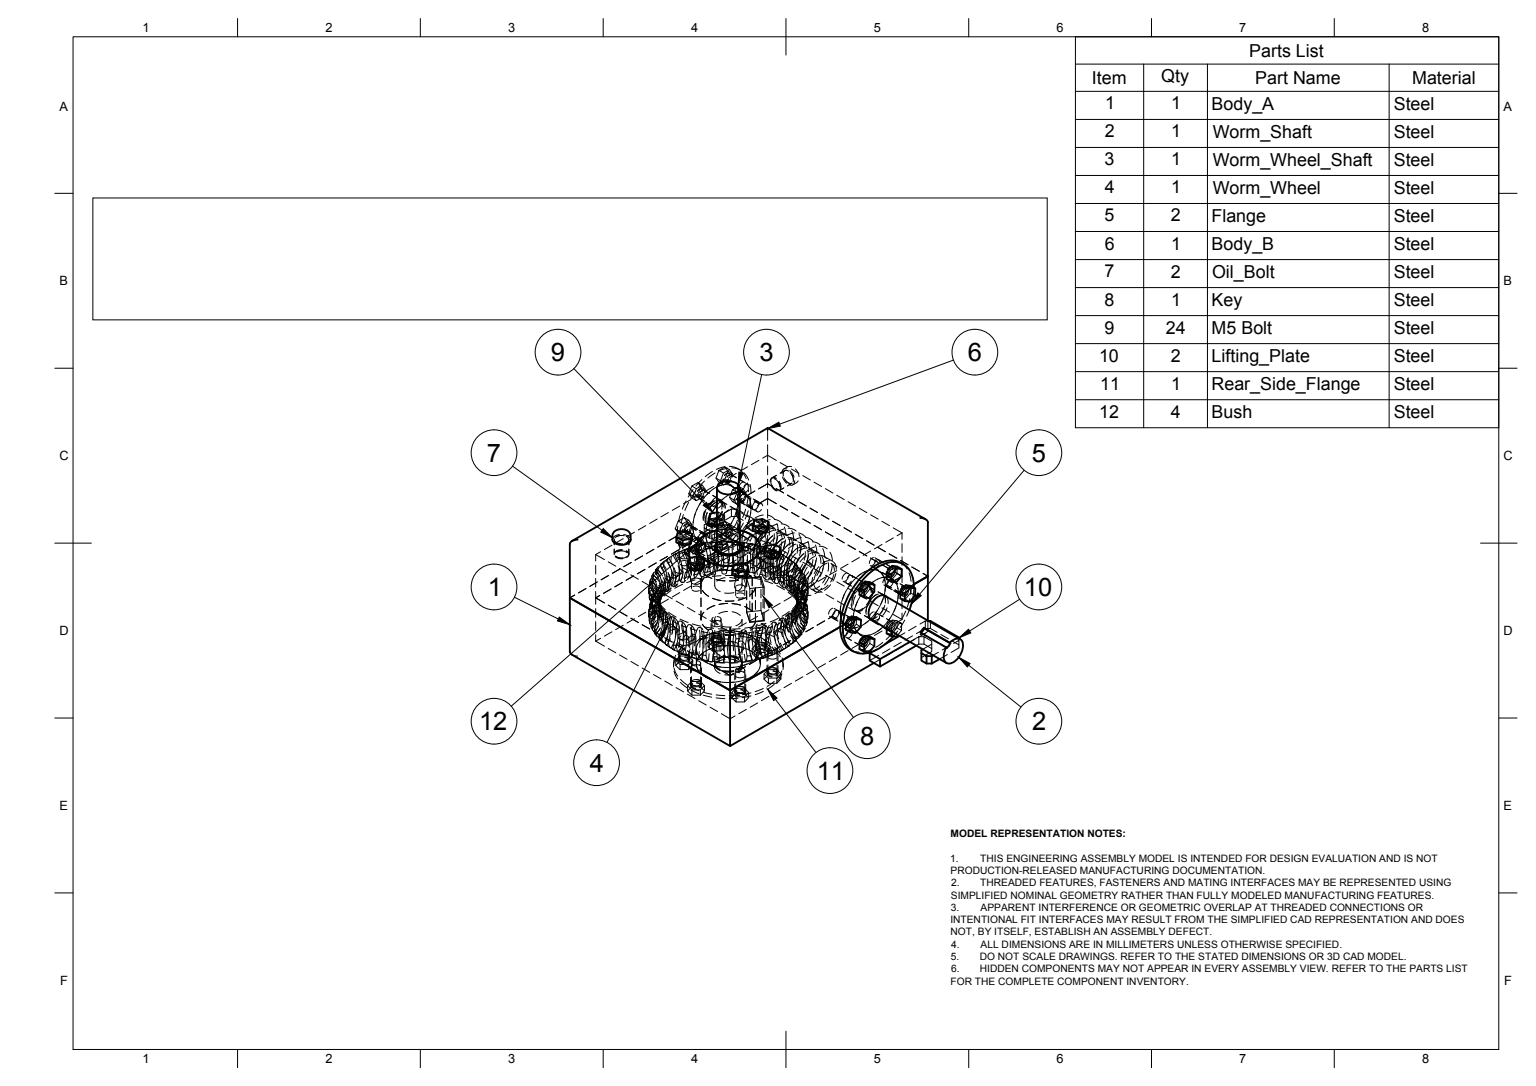
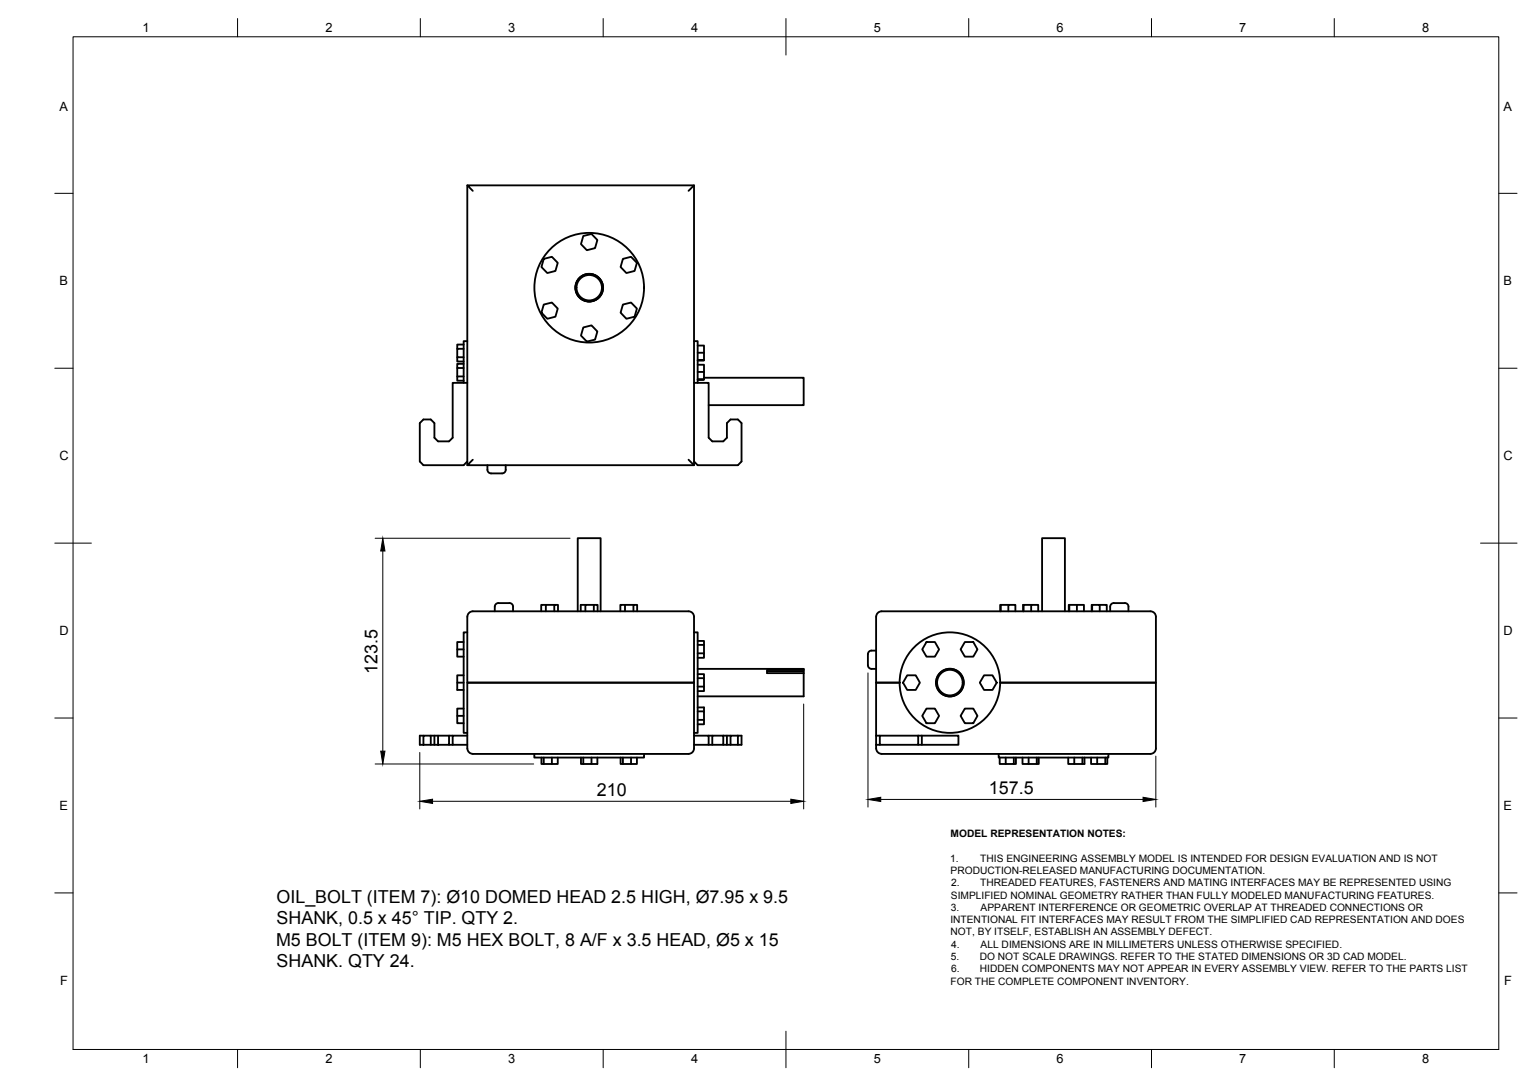
ISO-10303-21;
HEADER;
/* Generated by software containing ST-Developer
 * from STEP Tools, Inc. (www.steptools.com) 
 */

FILE_DESCRIPTION(
/* description */ ('STEP AP214'),
/* implementation_level */ '2;1');

FILE_NAME(
/* name */ 'MAS-619',
/* time_stamp */ '2026-10-05T13:15:56-07:00',
/* author */ (''),
/* organization */ (''),
/* preprocessor_version */ 'ST-DEVELOPER v20.2',
/* originating_system */ 'Autodesk Translation Framework v15.15.0.0',
/* authorisation */ '');

FILE_SCHEMA (('AUTOMOTIVE_DESIGN { 1 0 10303 214 3 1 1 }'));
ENDSEC;

DATA;
#10=MECHANICAL_DESIGN_GEOMETRIC_PRESENTATION_REPRESENTATION('',(#1345,#1346,
#1347,#1348,#1349,#1350,#1351,#1352,#1353,#1354,#1355,#1356),#37881);
#11=ITEM_DEFINED_TRANSFORMATION($,$,#10965,#11849);
#12=ITEM_DEFINED_TRANSFORMATION($,$,#11041,#11850);
#13=ITEM_DEFINED_TRANSFORMATION($,$,#11080,#11851);
#14=ITEM_DEFINED_TRANSFORMATION($,$,#11110,#11852);
#15=ITEM_DEFINED_TRANSFORMATION($,$,#11767,#11853);
#16=ITEM_DEFINED_TRANSFORMATION($,$,#11607,#11854);
#17=ITEM_DEFINED_TRANSFORMATION($,$,#11794,#11855);
#18=ITEM_DEFINED_TRANSFORMATION($,$,#11689,#11856);
#19=ITEM_DEFINED_TRANSFORMATION($,$,#11810,#11857);
#20=ITEM_DEFINED_TRANSFORMATION($,$,#11823,#11858);
#21=ITEM_DEFINED_TRANSFORMATION($,$,#11740,#11859);
#22=ITEM_DEFINED_TRANSFORMATION($,$,#11840,#11860);
#23=ITEM_DEFINED_TRANSFORMATION($,$,#11767,#11861);
#24=ITEM_DEFINED_TRANSFORMATION($,$,#11794,#11862);
#25=ITEM_DEFINED_TRANSFORMATION($,$,#11810,#11863);
#26=ITEM_DEFINED_TRANSFORMATION($,$,#11810,#11864);
#27=ITEM_DEFINED_TRANSFORMATION($,$,#11810,#11865);
#28=ITEM_DEFINED_TRANSFORMATION($,$,#11810,#11866);
#29=ITEM_DEFINED_TRANSFORMATION($,$,#11810,#11867);
#30=ITEM_DEFINED_TRANSFORMATION($,$,#11810,#11868);
#31=ITEM_DEFINED_TRANSFORMATION($,$,#11810,#11869);
#32=ITEM_DEFINED_TRANSFORMATION($,$,#11810,#11870);
#33=ITEM_DEFINED_TRANSFORMATION($,$,#11810,#11871);
#34=ITEM_DEFINED_TRANSFORMATION($,$,#11810,#11872);
#35=ITEM_DEFINED_TRANSFORMATION($,$,#11810,#11873);
#36=ITEM_DEFINED_TRANSFORMATION($,$,#11810,#11874);
#37=ITEM_DEFINED_TRANSFORMATION($,$,#11810,#11875);
#38=ITEM_DEFINED_TRANSFORMATION($,$,#11810,#11876);
#39=ITEM_DEFINED_TRANSFORMATION($,$,#11810,#11877);
#40=ITEM_DEFINED_TRANSFORMATION($,$,#11810,#11878);
#41=ITEM_DEFINED_TRANSFORMATION($,$,#11810,#11879);
#42=ITEM_DEFINED_TRANSFORMATION($,$,#11810,#11880);
#43=ITEM_DEFINED_TRANSFORMATION($,$,#11810,#11881);
#44=ITEM_DEFINED_TRANSFORMATION($,$,#11810,#11882);
#45=ITEM_DEFINED_TRANSFORMATION($,$,#11810,#11883);
#46=ITEM_DEFINED_TRANSFORMATION($,$,#11810,#11884);
#47=ITEM_DEFINED_TRANSFORMATION($,$,#11810,#11885);
#48=ITEM_DEFINED_TRANSFORMATION($,$,#11823,#11886);
#49=ITEM_DEFINED_TRANSFORMATION($,$,#11840,#11887);
#50=ITEM_DEFINED_TRANSFORMATION($,$,#11840,#11888);
#51=ITEM_DEFINED_TRANSFORMATION($,$,#11840,#11889);
#52=(
REPRESENTATION_RELATIONSHIP($,$,#37954,#37953)
REPRESENTATION_RELATIONSHIP_WITH_TRANSFORMATION(#11)
SHAPE_REPRESENTATION_RELATIONSHIP()
);
#53=(
REPRESENTATION_RELATIONSHIP($,$,#37955,#37953)
REPRESENTATION_RELATIONSHIP_WITH_TRANSFORMATION(#12)
SHAPE_REPRESENTATION_RELATIONSHIP()
);
#54=(
REPRESENTATION_RELATIONSHIP($,$,#37956,#37953)
REPRESENTATION_RELATIONSHIP_WITH_TRANSFORMATION(#13)
SHAPE_REPRESENTATION_RELATIONSHIP()
);
#55=(
REPRESENTATION_RELATIONSHIP($,$,#37957,#37953)
REPRESENTATION_RELATIONSHIP_WITH_TRANSFORMATION(#14)
SHAPE_REPRESENTATION_RELATIONSHIP()
);
#56=(
REPRESENTATION_RELATIONSHIP($,$,#37961,#37953)
REPRESENTATION_RELATIONSHIP_WITH_TRANSFORMATION(#15)
SHAPE_REPRESENTATION_RELATIONSHIP()
);
#57=(
REPRESENTATION_RELATIONSHIP($,$,#37958,#37953)
REPRESENTATION_RELATIONSHIP_WITH_TRANSFORMATION(#16)
SHAPE_REPRESENTATION_RELATIONSHIP()
);
#58=(
REPRESENTATION_RELATIONSHIP($,$,#37962,#37953)
REPRESENTATION_RELATIONSHIP_WITH_TRANSFORMATION(#17)
SHAPE_REPRESENTATION_RELATIONSHIP()
);
#59=(
REPRESENTATION_RELATIONSHIP($,$,#37959,#37953)
REPRESENTATION_RELATIONSHIP_WITH_TRANSFORMATION(#18)
SHAPE_REPRESENTATION_RELATIONSHIP()
);
#60=(
REPRESENTATION_RELATIONSHIP($,$,#37963,#37953)
REPRESENTATION_RELATIONSHIP_WITH_TRANSFORMATION(#19)
SHAPE_REPRESENTATION_RELATIONSHIP()
);
#61=(
REPRESENTATION_RELATIONSHIP($,$,#37964,#37953)
REPRESENTATION_RELATIONSHIP_WITH_TRANSFORMATION(#20)
SHAPE_REPRESENTATION_RELATIONSHIP()
);
#62=(
REPRESENTATION_RELATIONSHIP($,$,#37960,#37953)
REPRESENTATION_RELATIONSHIP_WITH_TRANSFORMATION(#21)
SHAPE_REPRESENTATION_RELATIONSHIP()
);
#63=(
REPRESENTATION_RELATIONSHIP($,$,#37965,#37953)
REPRESENTATION_RELATIONSHIP_WITH_TRANSFORMATION(#22)
SHAPE_REPRESENTATION_RELATIONSHIP()
);
#64=(
REPRESENTATION_RELATIONSHIP($,$,#37961,#37953)
REPRESENTATION_RELATIONSHIP_WITH_TRANSFORMATION(#23)
SHAPE_REPRESENTATION_RELATIONSHIP()
);
#65=(
REPRESENTATION_RELATIONSHIP($,$,#37962,#37953)
REPRESENTATION_RELATIONSHIP_WITH_TRANSFORMATION(#24)
SHAPE_REPRESENTATION_RELATIONSHIP()
);
#66=(
REPRESENTATION_RELATIONSHIP($,$,#37963,#37953)
REPRESENTATION_RELATIONSHIP_WITH_TRANSFORMATION(#25)
SHAPE_REPRESENTATION_RELATIONSHIP()
);
#67=(
REPRESENTATION_RELATIONSHIP($,$,#37963,#37953)
REPRESENTATION_RELATIONSHIP_WITH_TRANSFORMATION(#26)
SHAPE_REPRESENTATION_RELATIONSHIP()
);
#68=(
REPRESENTATION_RELATIONSHIP($,$,#37963,#37953)
REPRESENTATION_RELATIONSHIP_WITH_TRANSFORMATION(#27)
SHAPE_REPRESENTATION_RELATIONSHIP()
);
#69=(
REPRESENTATION_RELATIONSHIP($,$,#37963,#37953)
REPRESENTATION_RELATIONSHIP_WITH_TRANSFORMATION(#28)
SHAPE_REPRESENTATION_RELATIONSHIP()
);
#70=(
REPRESENTATION_RELATIONSHIP($,$,#37963,#37953)
REPRESENTATION_RELATIONSHIP_WITH_TRANSFORMATION(#29)
SHAPE_REPRESENTATION_RELATIONSHIP()
);
#71=(
REPRESENTATION_RELATIONSHIP($,$,#37963,#37953)
REPRESENTATION_RELATIONSHIP_WITH_TRANSFORMATION(#30)
SHAPE_REPRESENTATION_RELATIONSHIP()
);
#72=(
REPRESENTATION_RELATIONSHIP($,$,#37963,#37953)
REPRESENTATION_RELATIONSHIP_WITH_TRANSFORMATION(#31)
SHAPE_REPRESENTATION_RELATIONSHIP()
);
#73=(
REPRESENTATION_RELATIONSHIP($,$,#37963,#37953)
REPRESENTATION_RELATIONSHIP_WITH_TRANSFORMATION(#32)
SHAPE_REPRESENTATION_RELATIONSHIP()
);
#74=(
REPRESENTATION_RELATIONSHIP($,$,#37963,#37953)
REPRESENTATION_RELATIONSHIP_WITH_TRANSFORMATION(#33)
SHAPE_REPRESENTATION_RELATIONSHIP()
);
#75=(
REPRESENTATION_RELATIONSHIP($,$,#37963,#37953)
REPRESENTATION_RELATIONSHIP_WITH_TRANSFORMATION(#34)
SHAPE_REPRESENTATION_RELATIONSHIP()
);
#76=(
REPRESENTATION_RELATIONSHIP($,$,#37963,#37953)
REPRESENTATION_RELATIONSHIP_WITH_TRANSFORMATION(#35)
SHAPE_REPRESENTATION_RELATIONSHIP()
);
#77=(
REPRESENTATION_RELATIONSHIP($,$,#37963,#37953)
REPRESENTATION_RELATIONSHIP_WITH_TRANSFORMATION(#36)
SHAPE_REPRESENTATION_RELATIONSHIP()
);
#78=(
REPRESENTATION_RELATIONSHIP($,$,#37963,#37953)
REPRESENTATION_RELATIONSHIP_WITH_TRANSFORMATION(#37)
SHAPE_REPRESENTATION_RELATIONSHIP()
);
#79=(
REPRESENTATION_RELATIONSHIP($,$,#37963,#37953)
REPRESENTATION_RELATIONSHIP_WITH_TRANSFORMATION(#38)
SHAPE_REPRESENTATION_RELATIONSHIP()
);
#80=(
REPRESENTATION_RELATIONSHIP($,$,#37963,#37953)
REPRESENTATION_RELATIONSHIP_WITH_TRANSFORMATION(#39)
SHAPE_REPRESENTATION_RELATIONSHIP()
);
#81=(
REPRESENTATION_RELATIONSHIP($,$,#37963,#37953)
REPRESENTATION_RELATIONSHIP_WITH_TRANSFORMATION(#40)
SHAPE_REPRESENTATION_RELATIONSHIP()
);
#82=(
REPRESENTATION_RELATIONSHIP($,$,#37963,#37953)
REPRESENTATION_RELATIONSHIP_WITH_TRANSFORMATION(#41)
SHAPE_REPRESENTATION_RELATIONSHIP()
);
#83=(
REPRESENTATION_RELATIONSHIP($,$,#37963,#37953)
REPRESENTATION_RELATIONSHIP_WITH_TRANSFORMATION(#42)
SHAPE_REPRESENTATION_RELATIONSHIP()
);
#84=(
REPRESENTATION_RELATIONSHIP($,$,#37963,#37953)
REPRESENTATION_RELATIONSHIP_WITH_TRANSFORMATION(#43)
SHAPE_REPRESENTATION_RELATIONSHIP()
);
#85=(
REPRESENTATION_RELATIONSHIP($,$,#37963,#37953)
REPRESENTATION_RELATIONSHIP_WITH_TRANSFORMATION(#44)
SHAPE_REPRESENTATION_RELATIONSHIP()
);
#86=(
REPRESENTATION_RELATIONSHIP($,$,#37963,#37953)
REPRESENTATION_RELATIONSHIP_WITH_TRANSFORMATION(#45)
SHAPE_REPRESENTATION_RELATIONSHIP()
);
#87=(
REPRESENTATION_RELATIONSHIP($,$,#37963,#37953)
REPRESENTATION_RELATIONSHIP_WITH_TRANSFORMATION(#46)
SHAPE_REPRESENTATION_RELATIONSHIP()
);
#88=(
REPRESENTATION_RELATIONSHIP($,$,#37963,#37953)
REPRESENTATION_RELATIONSHIP_WITH_TRANSFORMATION(#47)
SHAPE_REPRESENTATION_RELATIONSHIP()
);
#89=(
REPRESENTATION_RELATIONSHIP($,$,#37964,#37953)
REPRESENTATION_RELATIONSHIP_WITH_TRANSFORMATION(#48)
SHAPE_REPRESENTATION_RELATIONSHIP()
);
#90=(
REPRESENTATION_RELATIONSHIP($,$,#37965,#37953)
REPRESENTATION_RELATIONSHIP_WITH_TRANSFORMATION(#49)
SHAPE_REPRESENTATION_RELATIONSHIP()
);
#91=(
REPRESENTATION_RELATIONSHIP($,$,#37965,#37953)
REPRESENTATION_RELATIONSHIP_WITH_TRANSFORMATION(#50)
SHAPE_REPRESENTATION_RELATIONSHIP()
);
#92=(
REPRESENTATION_RELATIONSHIP($,$,#37965,#37953)
REPRESENTATION_RELATIONSHIP_WITH_TRANSFORMATION(#51)
SHAPE_REPRESENTATION_RELATIONSHIP()
);
#93=CONTEXT_DEPENDENT_SHAPE_REPRESENTATION(#52,#37912);
#94=CONTEXT_DEPENDENT_SHAPE_REPRESENTATION(#53,#37913);
#95=CONTEXT_DEPENDENT_SHAPE_REPRESENTATION(#54,#37914);
#96=CONTEXT_DEPENDENT_SHAPE_REPRESENTATION(#55,#37915);
#97=CONTEXT_DEPENDENT_SHAPE_REPRESENTATION(#56,#37916);
#98=CONTEXT_DEPENDENT_SHAPE_REPRESENTATION(#57,#37917);
#99=CONTEXT_DEPENDENT_SHAPE_REPRESENTATION(#58,#37918);
#100=CONTEXT_DEPENDENT_SHAPE_REPRESENTATION(#59,#37919);
#101=CONTEXT_DEPENDENT_SHAPE_REPRESENTATION(#60,#37920);
#102=CONTEXT_DEPENDENT_SHAPE_REPRESENTATION(#61,#37921);
#103=CONTEXT_DEPENDENT_SHAPE_REPRESENTATION(#62,#37922);
#104=CONTEXT_DEPENDENT_SHAPE_REPRESENTATION(#63,#37923);
#105=CONTEXT_DEPENDENT_SHAPE_REPRESENTATION(#64,#37924);
#106=CONTEXT_DEPENDENT_SHAPE_REPRESENTATION(#65,#37925);
#107=CONTEXT_DEPENDENT_SHAPE_REPRESENTATION(#66,#37926);
#108=CONTEXT_DEPENDENT_SHAPE_REPRESENTATION(#67,#37927);
#109=CONTEXT_DEPENDENT_SHAPE_REPRESENTATION(#68,#37928);
#110=CONTEXT_DEPENDENT_SHAPE_REPRESENTATION(#69,#37929);
#111=CONTEXT_DEPENDENT_SHAPE_REPRESENTATION(#70,#37930);
#112=CONTEXT_DEPENDENT_SHAPE_REPRESENTATION(#71,#37931);
#113=CONTEXT_DEPENDENT_SHAPE_REPRESENTATION(#72,#37932);
#114=CONTEXT_DEPENDENT_SHAPE_REPRESENTATION(#73,#37933);
#115=CONTEXT_DEPENDENT_SHAPE_REPRESENTATION(#74,#37934);
#116=CONTEXT_DEPENDENT_SHAPE_REPRESENTATION(#75,#37935);
#117=CONTEXT_DEPENDENT_SHAPE_REPRESENTATION(#76,#37936);
#118=CONTEXT_DEPENDENT_SHAPE_REPRESENTATION(#77,#37937);
#119=CONTEXT_DEPENDENT_SHAPE_REPRESENTATION(#78,#37938);
#120=CONTEXT_DEPENDENT_SHAPE_REPRESENTATION(#79,#37939);
#121=CONTEXT_DEPENDENT_SHAPE_REPRESENTATION(#80,#37940);
#122=CONTEXT_DEPENDENT_SHAPE_REPRESENTATION(#81,#37941);
#123=CONTEXT_DEPENDENT_SHAPE_REPRESENTATION(#82,#37942);
#124=CONTEXT_DEPENDENT_SHAPE_REPRESENTATION(#83,#37943);
#125=CONTEXT_DEPENDENT_SHAPE_REPRESENTATION(#84,#37944);
#126=CONTEXT_DEPENDENT_SHAPE_REPRESENTATION(#85,#37945);
#127=CONTEXT_DEPENDENT_SHAPE_REPRESENTATION(#86,#37946);
#128=CONTEXT_DEPENDENT_SHAPE_REPRESENTATION(#87,#37947);
#129=CONTEXT_DEPENDENT_SHAPE_REPRESENTATION(#88,#37948);
#130=CONTEXT_DEPENDENT_SHAPE_REPRESENTATION(#89,#37949);
#131=CONTEXT_DEPENDENT_SHAPE_REPRESENTATION(#90,#37950);
#132=CONTEXT_DEPENDENT_SHAPE_REPRESENTATION(#91,#37951);
#133=CONTEXT_DEPENDENT_SHAPE_REPRESENTATION(#92,#37952);
#134=NEXT_ASSEMBLY_USAGE_OCCURRENCE('Body_A:1','Body_A:1','Body_A:1',#37967,
#37968,'Body_A:1');
#135=NEXT_ASSEMBLY_USAGE_OCCURRENCE('Worm_Shaft:1','Worm_Shaft:1',
'Worm_Shaft:1',#37967,#37969,'Worm_Shaft:1');
#136=NEXT_ASSEMBLY_USAGE_OCCURRENCE('Worm_Wheel_Shaft:1',
'Worm_Wheel_Shaft:1','Worm_Wheel_Shaft:1',#37967,#37970,
'Worm_Wheel_Shaft:1');
#137=NEXT_ASSEMBLY_USAGE_OCCURRENCE('Worm_Wheel:1','Worm_Wheel:1',
'Worm_Wheel:1',#37967,#37971,'Worm_Wheel:1');
#138=NEXT_ASSEMBLY_USAGE_OCCURRENCE('Flange:1','Flange:1','Flange:1',#37967,
#37975,'Flange:1');
#139=NEXT_ASSEMBLY_USAGE_OCCURRENCE('Body_B:1','Body_B:1','Body_B:1',#37967,
#37972,'Body_B:1');
#140=NEXT_ASSEMBLY_USAGE_OCCURRENCE('Oil_Bolt:1','Oil_Bolt:1',
'Oil_Bolt:1',#37967,#37976,'Oil_Bolt:1');
#141=NEXT_ASSEMBLY_USAGE_OCCURRENCE('Key:1','Key:1','Key:1',#37967,#37973,
'Key:1');
#142=NEXT_ASSEMBLY_USAGE_OCCURRENCE('M5 Bolt:1','M5 Bolt:1','M5 Bolt:1',
#37967,#37977,'M5 Bolt:1');
#143=NEXT_ASSEMBLY_USAGE_OCCURRENCE('Lifting_Plate:1','Lifting_Plate:1',
'Lifting_Plate:1',#37967,#37978,'Lifting_Plate:1');
#144=NEXT_ASSEMBLY_USAGE_OCCURRENCE('Rear_Side_Flange:1',
'Rear_Side_Flange:1','Rear_Side_Flange:1',#37967,#37974,
'Rear_Side_Flange:1');
#145=NEXT_ASSEMBLY_USAGE_OCCURRENCE('Bush:1','Bush:1','Bush:1',#37967,#37979,
'Bush:1');
#146=NEXT_ASSEMBLY_USAGE_OCCURRENCE('Flange:2','Flange:2','Flange:2',#37967,
#37975,'Flange:2');
#147=NEXT_ASSEMBLY_USAGE_OCCURRENCE('Oil_Bolt:2','Oil_Bolt:2',
'Oil_Bolt:2',#37967,#37976,'Oil_Bolt:2');
#148=NEXT_ASSEMBLY_USAGE_OCCURRENCE('M5 Bolt:2','M5 Bolt:2','M5 Bolt:2',
#37967,#37977,'M5 Bolt:2');
#149=NEXT_ASSEMBLY_USAGE_OCCURRENCE('M5 Bolt:3','M5 Bolt:3','M5 Bolt:3',
#37967,#37977,'M5 Bolt:3');
#150=NEXT_ASSEMBLY_USAGE_OCCURRENCE('M5 Bolt:4','M5 Bolt:4','M5 Bolt:4',
#37967,#37977,'M5 Bolt:4');
#151=NEXT_ASSEMBLY_USAGE_OCCURRENCE('M5 Bolt:5','M5 Bolt:5','M5 Bolt:5',
#37967,#37977,'M5 Bolt:5');
#152=NEXT_ASSEMBLY_USAGE_OCCURRENCE('M5 Bolt:6','M5 Bolt:6','M5 Bolt:6',
#37967,#37977,'M5 Bolt:6');
#153=NEXT_ASSEMBLY_USAGE_OCCURRENCE('M5 Bolt:7','M5 Bolt:7','M5 Bolt:7',
#37967,#37977,'M5 Bolt:7');
#154=NEXT_ASSEMBLY_USAGE_OCCURRENCE('M5 Bolt:8','M5 Bolt:8','M5 Bolt:8',
#37967,#37977,'M5 Bolt:8');
#155=NEXT_ASSEMBLY_USAGE_OCCURRENCE('M5 Bolt:9','M5 Bolt:9','M5 Bolt:9',
#37967,#37977,'M5 Bolt:9');
#156=NEXT_ASSEMBLY_USAGE_OCCURRENCE('M5 Bolt:10','M5 Bolt:10',
'M5 Bolt:10',#37967,#37977,'M5 Bolt:10');
#157=NEXT_ASSEMBLY_USAGE_OCCURRENCE('M5 Bolt:11','M5 Bolt:11',
'M5 Bolt:11',#37967,#37977,'M5 Bolt:11');
#158=NEXT_ASSEMBLY_USAGE_OCCURRENCE('M5 Bolt:12','M5 Bolt:12',
'M5 Bolt:12',#37967,#37977,'M5 Bolt:12');
#159=NEXT_ASSEMBLY_USAGE_OCCURRENCE('M5 Bolt:13','M5 Bolt:13',
'M5 Bolt:13',#37967,#37977,'M5 Bolt:13');
#160=NEXT_ASSEMBLY_USAGE_OCCURRENCE('M5 Bolt:14','M5 Bolt:14',
'M5 Bolt:14',#37967,#37977,'M5 Bolt:14');
#161=NEXT_ASSEMBLY_USAGE_OCCURRENCE('M5 Bolt:15','M5 Bolt:15',
'M5 Bolt:15',#37967,#37977,'M5 Bolt:15');
#162=NEXT_ASSEMBLY_USAGE_OCCURRENCE('M5 Bolt:16','M5 Bolt:16',
'M5 Bolt:16',#37967,#37977,'M5 Bolt:16');
#163=NEXT_ASSEMBLY_USAGE_OCCURRENCE('M5 Bolt:17','M5 Bolt:17',
'M5 Bolt:17',#37967,#37977,'M5 Bolt:17');
#164=NEXT_ASSEMBLY_USAGE_OCCURRENCE('M5 Bolt:18','M5 Bolt:18',
'M5 Bolt:18',#37967,#37977,'M5 Bolt:18');
#165=NEXT_ASSEMBLY_USAGE_OCCURRENCE('M5 Bolt:19','M5 Bolt:19',
'M5 Bolt:19',#37967,#37977,'M5 Bolt:19');
#166=NEXT_ASSEMBLY_USAGE_OCCURRENCE('M5 Bolt:20','M5 Bolt:20',
'M5 Bolt:20',#37967,#37977,'M5 Bolt:20');
#167=NEXT_ASSEMBLY_USAGE_OCCURRENCE('M5 Bolt:21','M5 Bolt:21',
'M5 Bolt:21',#37967,#37977,'M5 Bolt:21');
#168=NEXT_ASSEMBLY_USAGE_OCCURRENCE('M5 Bolt:22','M5 Bolt:22',
'M5 Bolt:22',#37967,#37977,'M5 Bolt:22');
#169=NEXT_ASSEMBLY_USAGE_OCCURRENCE('M5 Bolt:23','M5 Bolt:23',
'M5 Bolt:23',#37967,#37977,'M5 Bolt:23');
#170=NEXT_ASSEMBLY_USAGE_OCCURRENCE('M5 Bolt:24','M5 Bolt:24',
'M5 Bolt:24',#37967,#37977,'M5 Bolt:24');
#171=NEXT_ASSEMBLY_USAGE_OCCURRENCE('Lifting_Plate:2','Lifting_Plate:2',
'Lifting_Plate:2',#37967,#37978,'Lifting_Plate:2');
#172=NEXT_ASSEMBLY_USAGE_OCCURRENCE('Bush:2','Bush:2','Bush:2',#37967,#37979,
'Bush:2');
#173=NEXT_ASSEMBLY_USAGE_OCCURRENCE('Bush:3','Bush:3','Bush:3',#37967,#37979,
'Bush:3');
#174=NEXT_ASSEMBLY_USAGE_OCCURRENCE('Bush:4','Bush:4','Bush:4',#37967,#37979,
'Bush:4');
#175=SPHERICAL_SURFACE('',#11699,0.5);
#176=SPHERICAL_SURFACE('',#11702,0.5);
#177=SPHERICAL_SURFACE('',#11719,0.5);
#178=SPHERICAL_SURFACE('',#11721,0.5);
#179=SPHERICAL_SURFACE('',#11723,0.5);
#180=SPHERICAL_SURFACE('',#11725,0.5);
#181=SPHERICAL_SURFACE('',#11735,0.5);
#182=SPHERICAL_SURFACE('',#11737,0.5);
#183=TOROIDAL_SURFACE('',#11111,52.,10.5);
#184=TOROIDAL_SURFACE('',#11114,52.,10.5);
#185=TOROIDAL_SURFACE('',#11117,52.,10.5);
#186=TOROIDAL_SURFACE('',#11120,52.,10.5);
#187=TOROIDAL_SURFACE('',#11123,52.,10.5);
#188=TOROIDAL_SURFACE('',#11126,52.,10.5);
#189=TOROIDAL_SURFACE('',#11129,52.,10.5);
#190=TOROIDAL_SURFACE('',#11132,52.,10.5);
#191=TOROIDAL_SURFACE('',#11135,52.,10.5);
#192=TOROIDAL_SURFACE('',#11138,52.,10.5);
#193=TOROIDAL_SURFACE('',#11141,52.,10.5);
#194=TOROIDAL_SURFACE('',#11144,52.,10.5);
#195=TOROIDAL_SURFACE('',#11147,52.,10.5);
#196=TOROIDAL_SURFACE('',#11150,52.,10.5);
#197=TOROIDAL_SURFACE('',#11153,52.,10.5);
#198=TOROIDAL_SURFACE('',#11156,52.,10.5);
#199=TOROIDAL_SURFACE('',#11159,52.,10.5);
#200=TOROIDAL_SURFACE('',#11162,52.,10.5);
#201=TOROIDAL_SURFACE('',#11165,52.,10.5);
#202=TOROIDAL_SURFACE('',#11168,52.,10.5);
#203=TOROIDAL_SURFACE('',#11171,52.,10.5);
#204=TOROIDAL_SURFACE('',#11174,52.,10.5);
#205=TOROIDAL_SURFACE('',#11177,52.,10.5);
#206=TOROIDAL_SURFACE('',#11180,52.,10.5);
#207=TOROIDAL_SURFACE('',#11183,52.,10.5);
#208=TOROIDAL_SURFACE('',#11186,52.,10.5);
#209=TOROIDAL_SURFACE('',#11189,52.,10.5);
#210=TOROIDAL_SURFACE('',#11192,52.,10.5);
#211=TOROIDAL_SURFACE('',#11195,52.,10.5);
#212=TOROIDAL_SURFACE('',#11198,52.,10.5);
#213=TOROIDAL_SURFACE('',#11201,52.,10.5);
#214=TOROIDAL_SURFACE('',#11204,52.,10.5);
#215=TOROIDAL_SURFACE('',#11207,52.,10.5);
#216=TOROIDAL_SURFACE('',#11210,52.,10.5);
#217=TOROIDAL_SURFACE('',#11213,52.,10.5);
#218=TOROIDAL_SURFACE('',#11216,52.,10.5);
#219=TOROIDAL_SURFACE('',#11219,52.,10.5);
#220=TOROIDAL_SURFACE('',#11222,52.,10.5);
#221=TOROIDAL_SURFACE('',#11225,52.,10.5);
#222=TOROIDAL_SURFACE('',#11228,52.,10.5);
#223=TOROIDAL_SURFACE('',#11231,52.,10.5);
#224=TOROIDAL_SURFACE('',#11234,52.,10.5);
#225=TOROIDAL_SURFACE('',#11237,52.,10.5);
#226=TOROIDAL_SURFACE('',#11240,52.,10.5);
#227=TOROIDAL_SURFACE('',#11798,3.,2.);
#228=(
BOUNDED_CURVE()
B_SPLINE_CURVE(2,(#15162,#15163,#15164,#15165,#15166,#15167,#15168,#15169,
#15170,#15171,#15172,#15173,#15174,#15175,#15176,#15177,#15178,#15179,#15180,
#15181,#15182,#15183,#15184,#15185,#15186,#15187,#15188,#15189,#15190,#15191,
#15192,#15193,#15194,#15195,#15196,#15197,#15198,#15199,#15200,#15201,#15202,
#15203,#15204,#15205,#15206,#15207,#15208,#15209,#15210,#15211,#15212,#15213,
#15214,#15215,#15216,#15217,#15218,#15219,#15220,#15221,#15222,#15223,#15224,
#15225,#15226,#15227,#15228,#15229,#15230,#15231,#15232,#15233,#15234,#15235,
#15236,#15237,#15238,#15239,#15240,#15241,#15242,#15243,#15244,#15245,#15246,
#15247,#15248,#15249,#15250,#15251,#15252,#15253,#15254,#15255,#15256,#15257,
#15258,#15259,#15260,#15261,#15262,#15263,#15264,#15265,#15266,#15267,#15268,
#15269,#15270,#15271,#15272,#15273,#15274),.UNSPECIFIED.,.F.,.F.)
B_SPLINE_CURVE_WITH_KNOTS((3,2,2,2,2,2,2,2,2,2,2,2,2,2,2,2,2,2,2,2,2,2,
2,2,2,2,2,2,2,2,2,2,2,2,2,2,2,2,2,2,2,2,2,2,2,2,2,2,2,2,2,2,2,2,2,2,3),
(0.,0.0178571428571429,0.0357142857142857,0.0535714285714286,0.0714285714285714,
0.0892857142857143,0.107142857142857,0.125,0.142857142857143,0.160714285714286,
0.178571428571429,0.196428571428571,0.214285714285714,0.232142857142857,
0.25,0.267857142857143,0.285714285714286,0.303571428571429,0.321428571428571,
0.339285714285714,0.357142857142857,0.375,0.392857142857143,0.410714285714286,
0.428571428571429,0.446428571428571,0.464285714285714,0.482142857142857,
0.5,0.517857142857143,0.535714285714286,0.553571428571429,0.571428571428571,
0.589285714285714,0.607142857142857,0.625,0.642857142857143,0.660714285714286,
0.678571428571429,0.696428571428571,0.714285714285714,0.732142857142857,
0.75,0.767857142857143,0.785714285714286,0.803571428571429,0.821428571428571,
0.839285714285714,0.857142857142857,0.875,0.892857142857143,0.910714285714286,
0.928571428571429,0.946428571428571,0.964285714285714,0.982142857142857,
1.),.UNSPECIFIED.)
CURVE()
GEOMETRIC_REPRESENTATION_ITEM()
RATIONAL_B_SPLINE_CURVE((1.,0.974927912181824,1.,0.974927912181824,1.,0.974927912181824,
1.,0.974927912181824,1.,0.974927912181824,1.,0.974927912181824,1.,0.974927912181824,
1.,0.974927912181824,1.,0.974927912181824,1.,0.974927912181824,1.,0.974927912181824,
1.,0.974927912181824,1.,0.974927912181824,1.,0.974927912181824,1.,0.974927912181824,
1.,0.974927912181824,1.,0.974927912181824,1.,0.974927912181824,1.,0.974927912181824,
1.,0.974927912181824,1.,0.974927912181824,1.,0.974927912181824,1.,0.974927912181824,
1.,0.974927912181824,1.,0.974927912181824,1.,0.974927912181824,1.,0.974927912181824,
1.,0.974927912181824,1.,0.974927912181824,1.,0.974927912181824,1.,0.974927912181824,
1.,0.974927912181824,1.,0.974927912181824,1.,0.974927912181824,1.,0.974927912181824,
1.,0.974927912181824,1.,0.974927912181824,1.,0.974927912181824,1.,0.974927912181824,
1.,0.974927912181824,1.,0.974927912181824,1.,0.974927912181824,1.,0.974927912181824,
1.,0.974927912181824,1.,0.974927912181824,1.,0.974927912181824,1.,0.974927912181824,
1.,0.974927912181824,1.,0.974927912181824,1.,0.974927912181824,1.,0.974927912181824,
1.,0.974927912181824,1.,0.974927912181824,1.,0.974927912181824,1.,0.974927912181824,
1.,0.974927912181824,1.))
REPRESENTATION_ITEM('')
);
#229=(
BOUNDED_CURVE()
B_SPLINE_CURVE(2,(#15729,#15730,#15731,#15732,#15733,#15734,#15735,#15736,
#15737,#15738,#15739,#15740,#15741,#15742,#15743,#15744,#15745,#15746,#15747,
#15748,#15749,#15750,#15751,#15752,#15753,#15754,#15755,#15756,#15757,#15758,
#15759,#15760,#15761,#15762,#15763,#15764,#15765,#15766,#15767,#15768,#15769,
#15770,#15771,#15772,#15773,#15774,#15775,#15776,#15777,#15778,#15779,#15780,
#15781,#15782,#15783,#15784,#15785,#15786,#15787,#15788,#15789,#15790,#15791,
#15792,#15793,#15794,#15795,#15796,#15797,#15798,#15799,#15800,#15801,#15802,
#15803,#15804,#15805,#15806,#15807,#15808,#15809,#15810,#15811,#15812,#15813,
#15814,#15815,#15816,#15817,#15818,#15819,#15820,#15821,#15822,#15823,#15824,
#15825,#15826,#15827,#15828,#15829,#15830,#15831,#15832,#15833,#15834,#15835,
#15836,#15837,#15838,#15839,#15840,#15841),.UNSPECIFIED.,.F.,.F.)
B_SPLINE_CURVE_WITH_KNOTS((3,2,2,2,2,2,2,2,2,2,2,2,2,2,2,2,2,2,2,2,2,2,
2,2,2,2,2,2,2,2,2,2,2,2,2,2,2,2,2,2,2,2,2,2,2,2,2,2,2,2,2,2,2,2,2,2,3),
(0.,0.0178571428571429,0.0357142857142857,0.0535714285714286,0.0714285714285714,
0.0892857142857143,0.107142857142857,0.125,0.142857142857143,0.160714285714286,
0.178571428571429,0.196428571428571,0.214285714285714,0.232142857142857,
0.25,0.267857142857143,0.285714285714286,0.303571428571429,0.321428571428571,
0.339285714285714,0.357142857142857,0.375,0.392857142857143,0.410714285714286,
0.428571428571429,0.446428571428571,0.464285714285714,0.482142857142857,
0.5,0.517857142857143,0.535714285714286,0.553571428571429,0.571428571428571,
0.589285714285714,0.607142857142857,0.625,0.642857142857143,0.660714285714286,
0.678571428571429,0.696428571428571,0.714285714285714,0.732142857142857,
0.75,0.767857142857143,0.785714285714286,0.803571428571429,0.821428571428571,
0.839285714285714,0.857142857142857,0.875,0.892857142857143,0.910714285714286,
0.928571428571429,0.946428571428571,0.964285714285714,0.982142857142857,
1.),.UNSPECIFIED.)
CURVE()
GEOMETRIC_REPRESENTATION_ITEM()
RATIONAL_B_SPLINE_CURVE((1.,0.974927912181824,1.,0.974927912181824,1.,0.974927912181824,
1.,0.974927912181824,1.,0.974927912181824,1.,0.974927912181824,1.,0.974927912181824,
1.,0.974927912181824,1.,0.974927912181824,1.,0.974927912181824,1.,0.974927912181824,
1.,0.974927912181824,1.,0.974927912181824,1.,0.974927912181824,1.,0.974927912181824,
1.,0.974927912181824,1.,0.974927912181824,1.,0.974927912181824,1.,0.974927912181824,
1.,0.974927912181824,1.,0.974927912181824,1.,0.974927912181824,1.,0.974927912181824,
1.,0.974927912181824,1.,0.974927912181824,1.,0.974927912181824,1.,0.974927912181824,
1.,0.974927912181824,1.,0.974927912181824,1.,0.974927912181824,1.,0.974927912181824,
1.,0.974927912181824,1.,0.974927912181824,1.,0.974927912181824,1.,0.974927912181824,
1.,0.974927912181824,1.,0.974927912181824,1.,0.974927912181824,1.,0.974927912181824,
1.,0.974927912181824,1.,0.974927912181824,1.,0.974927912181824,1.,0.974927912181824,
1.,0.974927912181824,1.,0.974927912181824,1.,0.974927912181824,1.,0.974927912181824,
1.,0.974927912181824,1.,0.974927912181824,1.,0.974927912181824,1.,0.974927912181824,
1.,0.974927912181824,1.,0.974927912181824,1.,0.974927912181824,1.,0.974927912181824,
1.,0.974927912181824,1.))
REPRESENTATION_ITEM('')
);
#230=(
BOUNDED_CURVE()
B_SPLINE_CURVE(2,(#16301,#16302,#16303,#16304,#16305,#16306,#16307,#16308,
#16309,#16310,#16311,#16312,#16313,#16314,#16315,#16316,#16317,#16318,#16319,
#16320,#16321,#16322,#16323,#16324,#16325,#16326,#16327,#16328,#16329,#16330,
#16331,#16332,#16333,#16334,#16335,#16336,#16337,#16338,#16339,#16340,#16341,
#16342,#16343,#16344,#16345,#16346,#16347,#16348,#16349,#16350,#16351,#16352,
#16353,#16354,#16355,#16356,#16357,#16358,#16359,#16360,#16361,#16362,#16363,
#16364,#16365,#16366,#16367,#16368,#16369,#16370,#16371,#16372,#16373,#16374,
#16375,#16376,#16377,#16378,#16379,#16380,#16381,#16382,#16383,#16384,#16385,
#16386,#16387,#16388,#16389,#16390,#16391,#16392,#16393,#16394,#16395,#16396,
#16397,#16398,#16399,#16400,#16401,#16402,#16403,#16404,#16405,#16406,#16407,
#16408,#16409,#16410,#16411,#16412,#16413),.UNSPECIFIED.,.F.,.F.)
B_SPLINE_CURVE_WITH_KNOTS((3,2,2,2,2,2,2,2,2,2,2,2,2,2,2,2,2,2,2,2,2,2,
2,2,2,2,2,2,2,2,2,2,2,2,2,2,2,2,2,2,2,2,2,2,2,2,2,2,2,2,2,2,2,2,2,2,3),
(0.,0.0178571428571429,0.0357142857142857,0.0535714285714286,0.0714285714285714,
0.0892857142857143,0.107142857142857,0.125,0.142857142857143,0.160714285714286,
0.178571428571429,0.196428571428571,0.214285714285714,0.232142857142857,
0.25,0.267857142857143,0.285714285714286,0.303571428571429,0.321428571428571,
0.339285714285714,0.357142857142857,0.375,0.392857142857143,0.410714285714286,
0.428571428571429,0.446428571428571,0.464285714285714,0.482142857142857,
0.5,0.517857142857143,0.535714285714286,0.553571428571429,0.571428571428571,
0.589285714285714,0.607142857142857,0.625,0.642857142857143,0.660714285714286,
0.678571428571429,0.696428571428571,0.714285714285714,0.732142857142857,
0.75,0.767857142857143,0.785714285714286,0.803571428571429,0.821428571428571,
0.839285714285714,0.857142857142857,0.875,0.892857142857143,0.910714285714286,
0.928571428571429,0.946428571428571,0.964285714285714,0.982142857142857,
1.),.UNSPECIFIED.)
CURVE()
GEOMETRIC_REPRESENTATION_ITEM()
RATIONAL_B_SPLINE_CURVE((1.,0.974927912181824,1.,0.974927912181824,1.,0.974927912181824,
1.,0.974927912181824,1.,0.974927912181824,1.,0.974927912181824,1.,0.974927912181824,
1.,0.974927912181824,1.,0.974927912181824,1.,0.974927912181824,1.,0.974927912181824,
1.,0.974927912181824,1.,0.974927912181824,1.,0.974927912181824,1.,0.974927912181824,
1.,0.974927912181824,1.,0.974927912181824,1.,0.974927912181824,1.,0.974927912181824,
1.,0.974927912181824,1.,0.974927912181824,1.,0.974927912181824,1.,0.974927912181824,
1.,0.974927912181824,1.,0.974927912181824,1.,0.974927912181824,1.,0.974927912181824,
1.,0.974927912181824,1.,0.974927912181824,1.,0.974927912181824,1.,0.974927912181824,
1.,0.974927912181824,1.,0.974927912181824,1.,0.974927912181824,1.,0.974927912181824,
1.,0.974927912181824,1.,0.974927912181824,1.,0.974927912181824,1.,0.974927912181824,
1.,0.974927912181824,1.,0.974927912181824,1.,0.974927912181824,1.,0.974927912181824,
1.,0.974927912181824,1.,0.974927912181824,1.,0.974927912181824,1.,0.974927912181824,
1.,0.974927912181824,1.,0.974927912181824,1.,0.974927912181824,1.,0.974927912181824,
1.,0.974927912181824,1.,0.974927912181824,1.,0.974927912181824,1.,0.974927912181824,
1.,0.974927912181824,1.))
REPRESENTATION_ITEM('')
);
#231=(
BOUNDED_CURVE()
B_SPLINE_CURVE(2,(#16866,#16867,#16868,#16869,#16870,#16871,#16872,#16873,
#16874,#16875,#16876,#16877,#16878,#16879,#16880,#16881,#16882,#16883,#16884,
#16885,#16886,#16887,#16888,#16889,#16890,#16891,#16892,#16893,#16894,#16895,
#16896,#16897,#16898,#16899,#16900,#16901,#16902,#16903,#16904,#16905,#16906,
#16907,#16908,#16909,#16910,#16911,#16912,#16913,#16914,#16915,#16916,#16917,
#16918,#16919,#16920,#16921,#16922,#16923,#16924,#16925,#16926,#16927,#16928,
#16929,#16930,#16931,#16932,#16933,#16934,#16935,#16936,#16937,#16938,#16939,
#16940,#16941,#16942,#16943,#16944,#16945,#16946,#16947,#16948,#16949,#16950,
#16951,#16952,#16953,#16954,#16955,#16956,#16957,#16958,#16959,#16960,#16961,
#16962,#16963,#16964,#16965,#16966,#16967,#16968,#16969,#16970,#16971,#16972,
#16973,#16974,#16975,#16976,#16977,#16978),.UNSPECIFIED.,.F.,.F.)
B_SPLINE_CURVE_WITH_KNOTS((3,2,2,2,2,2,2,2,2,2,2,2,2,2,2,2,2,2,2,2,2,2,
2,2,2,2,2,2,2,2,2,2,2,2,2,2,2,2,2,2,2,2,2,2,2,2,2,2,2,2,2,2,2,2,2,2,3),
(0.,0.0178571428571429,0.0357142857142857,0.0535714285714286,0.0714285714285714,
0.0892857142857143,0.107142857142857,0.125,0.142857142857143,0.160714285714286,
0.178571428571429,0.196428571428571,0.214285714285714,0.232142857142857,
0.25,0.267857142857143,0.285714285714286,0.303571428571429,0.321428571428571,
0.339285714285714,0.357142857142857,0.375,0.392857142857143,0.410714285714286,
0.428571428571429,0.446428571428571,0.464285714285714,0.482142857142857,
0.5,0.517857142857143,0.535714285714286,0.553571428571429,0.571428571428571,
0.589285714285714,0.607142857142857,0.625,0.642857142857143,0.660714285714286,
0.678571428571429,0.696428571428571,0.714285714285714,0.732142857142857,
0.75,0.767857142857143,0.785714285714286,0.803571428571429,0.821428571428571,
0.839285714285714,0.857142857142857,0.875,0.892857142857143,0.910714285714286,
0.928571428571429,0.946428571428571,0.964285714285714,0.982142857142857,
1.),.UNSPECIFIED.)
CURVE()
GEOMETRIC_REPRESENTATION_ITEM()
RATIONAL_B_SPLINE_CURVE((1.,0.974927912181824,1.,0.974927912181824,1.,0.974927912181824,
1.,0.974927912181824,1.,0.974927912181824,1.,0.974927912181824,1.,0.974927912181824,
1.,0.974927912181824,1.,0.974927912181824,1.,0.974927912181824,1.,0.974927912181824,
1.,0.974927912181824,1.,0.974927912181824,1.,0.974927912181824,1.,0.974927912181824,
1.,0.974927912181824,1.,0.974927912181824,1.,0.974927912181824,1.,0.974927912181824,
1.,0.974927912181824,1.,0.974927912181824,1.,0.974927912181824,1.,0.974927912181824,
1.,0.974927912181824,1.,0.974927912181824,1.,0.974927912181824,1.,0.974927912181824,
1.,0.974927912181824,1.,0.974927912181824,1.,0.974927912181824,1.,0.974927912181824,
1.,0.974927912181824,1.,0.974927912181824,1.,0.974927912181824,1.,0.974927912181824,
1.,0.974927912181824,1.,0.974927912181824,1.,0.974927912181824,1.,0.974927912181824,
1.,0.974927912181824,1.,0.974927912181824,1.,0.974927912181824,1.,0.974927912181824,
1.,0.974927912181824,1.,0.974927912181824,1.,0.974927912181824,1.,0.974927912181824,
1.,0.974927912181824,1.,0.974927912181824,1.,0.974927912181824,1.,0.974927912181824,
1.,0.974927912181824,1.,0.974927912181824,1.,0.974927912181824,1.,0.974927912181824,
1.,0.974927912181824,1.))
REPRESENTATION_ITEM('')
);
#232=(
BOUNDED_CURVE()
B_SPLINE_CURVE(2,(#22947,#22948,#22949,#22950,#22951),.UNSPECIFIED.,.F.,
 .F.)
B_SPLINE_CURVE_WITH_KNOTS((3,2,3),(0.,0.25,0.459577358091282),
 .UNSPECIFIED.)
CURVE()
GEOMETRIC_REPRESENTATION_ITEM()
RATIONAL_B_SPLINE_CURVE((1.,0.974927912181824,1.,0.978981832292936,0.9932031210656))
REPRESENTATION_ITEM('')
);
#233=(
BOUNDED_CURVE()
B_SPLINE_CURVE(3,(#23082,#23083,#23084,#23085,#23086,#23087,#23088,#23089),
 .UNSPECIFIED.,.F.,.F.)
B_SPLINE_CURVE_WITH_KNOTS((4,2,2,4),(0.0783698293107414,0.308777371982556,
0.539184914655036,0.563918778704656),.UNSPECIFIED.)
CURVE()
GEOMETRIC_REPRESENTATION_ITEM()
RATIONAL_B_SPLINE_CURVE((1.,1.,1.,1.,1.,1.,1.,1.))
REPRESENTATION_ITEM('')
);
#234=(
BOUNDED_CURVE()
B_SPLINE_CURVE(2,(#23313,#23314,#23315,#23316,#23317),.UNSPECIFIED.,.F.,
 .F.)
B_SPLINE_CURVE_WITH_KNOTS((3,2,3),(0.,0.25,0.459577358091282),
 .UNSPECIFIED.)
CURVE()
GEOMETRIC_REPRESENTATION_ITEM()
RATIONAL_B_SPLINE_CURVE((1.,0.974927912181824,1.,0.978981832292936,0.9932031210656))
REPRESENTATION_ITEM('')
);
#235=(
BOUNDED_CURVE()
B_SPLINE_CURVE(2,(#23485,#23486,#23487,#23488,#23489),.UNSPECIFIED.,.F.,
 .F.)
B_SPLINE_CURVE_WITH_KNOTS((3,2,3),(0.,0.25,0.459577358091281),
 .UNSPECIFIED.)
CURVE()
GEOMETRIC_REPRESENTATION_ITEM()
RATIONAL_B_SPLINE_CURVE((1.,0.974927912181824,1.,0.978981832292936,0.9932031210656))
REPRESENTATION_ITEM('')
);
#236=(
BOUNDED_CURVE()
B_SPLINE_CURVE(2,(#23568,#23569,#23570,#23571,#23572),.UNSPECIFIED.,.F.,
 .F.)
B_SPLINE_CURVE_WITH_KNOTS((3,2,3),(0.,0.25,0.460808762537663),
 .UNSPECIFIED.)
CURVE()
GEOMETRIC_REPRESENTATION_ITEM()
RATIONAL_B_SPLINE_CURVE((1.,0.974927912181824,1.,0.978858336771259,0.993371456448429))
REPRESENTATION_ITEM('')
);
#237=(
BOUNDED_CURVE()
B_SPLINE_CURVE(2,(#23610,#23611,#23612,#23613,#23614),.UNSPECIFIED.,.F.,
 .F.)
B_SPLINE_CURVE_WITH_KNOTS((3,2,3),(0.,0.25,0.459577358091282),
 .UNSPECIFIED.)
CURVE()
GEOMETRIC_REPRESENTATION_ITEM()
RATIONAL_B_SPLINE_CURVE((1.,0.974927912181824,1.,0.978981832292936,0.9932031210656))
REPRESENTATION_ITEM('')
);
#238=(
BOUNDED_CURVE()
B_SPLINE_CURVE(2,(#23782,#23783,#23784,#23785,#23786),.UNSPECIFIED.,.F.,
 .F.)
B_SPLINE_CURVE_WITH_KNOTS((3,2,3),(0.,0.25,0.459577358091282),
 .UNSPECIFIED.)
CURVE()
GEOMETRIC_REPRESENTATION_ITEM()
RATIONAL_B_SPLINE_CURVE((1.,0.974927912181824,1.,0.978981832292936,0.9932031210656))
REPRESENTATION_ITEM('')
);
#239=(
BOUNDED_CURVE()
B_SPLINE_CURVE(2,(#23954,#23955,#23956,#23957,#23958),.UNSPECIFIED.,.F.,
 .F.)
B_SPLINE_CURVE_WITH_KNOTS((3,2,3),(0.,0.25,0.459577358091282),
 .UNSPECIFIED.)
CURVE()
GEOMETRIC_REPRESENTATION_ITEM()
RATIONAL_B_SPLINE_CURVE((1.,0.974927912181824,1.,0.978981832292936,0.9932031210656))
REPRESENTATION_ITEM('')
);
#240=(
BOUNDED_CURVE()
B_SPLINE_CURVE(2,(#24126,#24127,#24128,#24129,#24130),.UNSPECIFIED.,.F.,
 .F.)
B_SPLINE_CURVE_WITH_KNOTS((3,2,3),(0.,0.25,0.459577358091283),
 .UNSPECIFIED.)
CURVE()
GEOMETRIC_REPRESENTATION_ITEM()
RATIONAL_B_SPLINE_CURVE((1.,0.974927912181824,1.,0.978981832292936,0.9932031210656))
REPRESENTATION_ITEM('')
);
#241=(
BOUNDED_CURVE()
B_SPLINE_CURVE(2,(#24298,#24299,#24300,#24301,#24302),.UNSPECIFIED.,.F.,
 .F.)
B_SPLINE_CURVE_WITH_KNOTS((3,2,3),(0.,0.25,0.459577358091282),
 .UNSPECIFIED.)
CURVE()
GEOMETRIC_REPRESENTATION_ITEM()
RATIONAL_B_SPLINE_CURVE((1.,0.974927912181824,1.,0.978981832292936,0.9932031210656))
REPRESENTATION_ITEM('')
);
#242=(
BOUNDED_CURVE()
B_SPLINE_CURVE(2,(#24470,#24471,#24472,#24473,#24474),.UNSPECIFIED.,.F.,
 .F.)
B_SPLINE_CURVE_WITH_KNOTS((3,2,3),(0.,0.25,0.459577358091282),
 .UNSPECIFIED.)
CURVE()
GEOMETRIC_REPRESENTATION_ITEM()
RATIONAL_B_SPLINE_CURVE((1.,0.974927912181824,1.,0.978981832292936,0.9932031210656))
REPRESENTATION_ITEM('')
);
#243=(
BOUNDED_CURVE()
B_SPLINE_CURVE(2,(#24642,#24643,#24644,#24645,#24646),.UNSPECIFIED.,.F.,
 .F.)
B_SPLINE_CURVE_WITH_KNOTS((3,2,3),(0.,0.25,0.459577358091282),
 .UNSPECIFIED.)
CURVE()
GEOMETRIC_REPRESENTATION_ITEM()
RATIONAL_B_SPLINE_CURVE((1.,0.974927912181824,1.,0.978981832292936,0.9932031210656))
REPRESENTATION_ITEM('')
);
#244=(
BOUNDED_CURVE()
B_SPLINE_CURVE(2,(#24814,#24815,#24816,#24817,#24818),.UNSPECIFIED.,.F.,
 .F.)
B_SPLINE_CURVE_WITH_KNOTS((3,2,3),(0.,0.25,0.459577358091282),
 .UNSPECIFIED.)
CURVE()
GEOMETRIC_REPRESENTATION_ITEM()
RATIONAL_B_SPLINE_CURVE((1.,0.974927912181824,1.,0.978981832292936,0.9932031210656))
REPRESENTATION_ITEM('')
);
#245=(
BOUNDED_CURVE()
B_SPLINE_CURVE(2,(#24986,#24987,#24988,#24989,#24990),.UNSPECIFIED.,.F.,
 .F.)
B_SPLINE_CURVE_WITH_KNOTS((3,2,3),(0.,0.25,0.459577358091283),
 .UNSPECIFIED.)
CURVE()
GEOMETRIC_REPRESENTATION_ITEM()
RATIONAL_B_SPLINE_CURVE((1.,0.974927912181824,1.,0.978981832292936,0.9932031210656))
REPRESENTATION_ITEM('')
);
#246=(
BOUNDED_CURVE()
B_SPLINE_CURVE(2,(#25069,#25070,#25071,#25072,#25073),.UNSPECIFIED.,.F.,
 .F.)
B_SPLINE_CURVE_WITH_KNOTS((3,2,3),(0.,0.25,0.460808762537663),
 .UNSPECIFIED.)
CURVE()
GEOMETRIC_REPRESENTATION_ITEM()
RATIONAL_B_SPLINE_CURVE((1.,0.974927912181824,1.,0.978858336771258,0.993371456448429))
REPRESENTATION_ITEM('')
);
#247=(
BOUNDED_CURVE()
B_SPLINE_CURVE(2,(#25111,#25112,#25113,#25114,#25115),.UNSPECIFIED.,.F.,
 .F.)
B_SPLINE_CURVE_WITH_KNOTS((3,2,3),(0.,0.25,0.459577358091282),
 .UNSPECIFIED.)
CURVE()
GEOMETRIC_REPRESENTATION_ITEM()
RATIONAL_B_SPLINE_CURVE((1.,0.974927912181824,1.,0.978981832292936,0.9932031210656))
REPRESENTATION_ITEM('')
);
#248=(
BOUNDED_CURVE()
B_SPLINE_CURVE(2,(#25283,#25284,#25285,#25286,#25287),.UNSPECIFIED.,.F.,
 .F.)
B_SPLINE_CURVE_WITH_KNOTS((3,2,3),(0.,0.25,0.459577358091282),
 .UNSPECIFIED.)
CURVE()
GEOMETRIC_REPRESENTATION_ITEM()
RATIONAL_B_SPLINE_CURVE((1.,0.974927912181824,1.,0.978981832292936,0.9932031210656))
REPRESENTATION_ITEM('')
);
#249=(
BOUNDED_CURVE()
B_SPLINE_CURVE(2,(#25455,#25456,#25457,#25458,#25459),.UNSPECIFIED.,.F.,
 .F.)
B_SPLINE_CURVE_WITH_KNOTS((3,2,3),(0.,0.25,0.459577358091283),
 .UNSPECIFIED.)
CURVE()
GEOMETRIC_REPRESENTATION_ITEM()
RATIONAL_B_SPLINE_CURVE((1.,0.974927912181824,1.,0.978981832292936,0.9932031210656))
REPRESENTATION_ITEM('')
);
#250=(
BOUNDED_CURVE()
B_SPLINE_CURVE(2,(#25537,#25538,#25539,#25540,#25541),.UNSPECIFIED.,.F.,
 .F.)
B_SPLINE_CURVE_WITH_KNOTS((3,2,3),(0.,0.0714285714285714,0.131307816597586),
 .UNSPECIFIED.)
CURVE()
GEOMETRIC_REPRESENTATION_ITEM()
RATIONAL_B_SPLINE_CURVE((1.,0.974927912181824,1.,0.978981832292909,0.993203121065636))
REPRESENTATION_ITEM('')
);
#251=(
BOUNDED_CURVE()
B_SPLINE_CURVE(2,(#25581,#25582,#25583,#25584,#25585),.UNSPECIFIED.,.F.,
 .F.)
B_SPLINE_CURVE_WITH_KNOTS((3,2,3),(0.,0.0714285714285714,0.131659646439332),
 .UNSPECIFIED.)
CURVE()
GEOMETRIC_REPRESENTATION_ITEM()
RATIONAL_B_SPLINE_CURVE((1.,0.974927912181824,1.,0.978858336771259,0.993371456448429))
REPRESENTATION_ITEM('')
);
#252=(
BOUNDED_CURVE()
B_SPLINE_CURVE(2,(#25752,#25753,#25754,#25755,#25756),.UNSPECIFIED.,.F.,
 .F.)
B_SPLINE_CURVE_WITH_KNOTS((3,2,3),(0.,0.25,0.459577358091283),
 .UNSPECIFIED.)
CURVE()
GEOMETRIC_REPRESENTATION_ITEM()
RATIONAL_B_SPLINE_CURVE((1.,0.974927912181824,1.,0.978981832292936,0.9932031210656))
REPRESENTATION_ITEM('')
);
#253=(
BOUNDED_CURVE()
B_SPLINE_CURVE(2,(#25924,#25925,#25926,#25927,#25928),.UNSPECIFIED.,.F.,
 .F.)
B_SPLINE_CURVE_WITH_KNOTS((3,2,3),(0.,0.25,0.459577358091282),
 .UNSPECIFIED.)
CURVE()
GEOMETRIC_REPRESENTATION_ITEM()
RATIONAL_B_SPLINE_CURVE((1.,0.974927912181824,1.,0.978981832292936,0.9932031210656))
REPRESENTATION_ITEM('')
);
#254=(
BOUNDED_CURVE()
B_SPLINE_CURVE(2,(#26096,#26097,#26098,#26099,#26100),.UNSPECIFIED.,.F.,
 .F.)
B_SPLINE_CURVE_WITH_KNOTS((3,2,3),(0.,0.25,0.459577358091282),
 .UNSPECIFIED.)
CURVE()
GEOMETRIC_REPRESENTATION_ITEM()
RATIONAL_B_SPLINE_CURVE((1.,0.974927912181824,1.,0.978981832292936,0.9932031210656))
REPRESENTATION_ITEM('')
);
#255=(
BOUNDED_CURVE()
B_SPLINE_CURVE(2,(#26268,#26269,#26270,#26271,#26272),.UNSPECIFIED.,.F.,
 .F.)
B_SPLINE_CURVE_WITH_KNOTS((3,2,3),(0.,0.25,0.459577358091282),
 .UNSPECIFIED.)
CURVE()
GEOMETRIC_REPRESENTATION_ITEM()
RATIONAL_B_SPLINE_CURVE((1.,0.974927912181824,1.,0.978981832292936,0.9932031210656))
REPRESENTATION_ITEM('')
);
#256=(
BOUNDED_CURVE()
B_SPLINE_CURVE(2,(#26440,#26441,#26442,#26443,#26444),.UNSPECIFIED.,.F.,
 .F.)
B_SPLINE_CURVE_WITH_KNOTS((3,2,3),(0.,0.25,0.459577358091282),
 .UNSPECIFIED.)
CURVE()
GEOMETRIC_REPRESENTATION_ITEM()
RATIONAL_B_SPLINE_CURVE((1.,0.974927912181824,1.,0.978981832292936,0.9932031210656))
REPRESENTATION_ITEM('')
);
#257=(
BOUNDED_CURVE()
B_SPLINE_CURVE(2,(#26612,#26613,#26614,#26615,#26616),.UNSPECIFIED.,.F.,
 .F.)
B_SPLINE_CURVE_WITH_KNOTS((3,2,3),(0.,0.25,0.459577358091282),
 .UNSPECIFIED.)
CURVE()
GEOMETRIC_REPRESENTATION_ITEM()
RATIONAL_B_SPLINE_CURVE((1.,0.974927912181824,1.,0.978981832292936,0.9932031210656))
REPRESENTATION_ITEM('')
);
#258=(
BOUNDED_CURVE()
B_SPLINE_CURVE(2,(#26784,#26785,#26786,#26787,#26788),.UNSPECIFIED.,.F.,
 .F.)
B_SPLINE_CURVE_WITH_KNOTS((3,2,3),(0.,0.25,0.459577358091282),
 .UNSPECIFIED.)
CURVE()
GEOMETRIC_REPRESENTATION_ITEM()
RATIONAL_B_SPLINE_CURVE((1.,0.974927912181824,1.,0.978981832292936,0.9932031210656))
REPRESENTATION_ITEM('')
);
#259=(
BOUNDED_CURVE()
B_SPLINE_CURVE(2,(#26956,#26957,#26958,#26959,#26960),.UNSPECIFIED.,.F.,
 .F.)
B_SPLINE_CURVE_WITH_KNOTS((3,2,3),(0.,0.25,0.459577358091282),
 .UNSPECIFIED.)
CURVE()
GEOMETRIC_REPRESENTATION_ITEM()
RATIONAL_B_SPLINE_CURVE((1.,0.974927912181824,1.,0.978981832292936,0.9932031210656))
REPRESENTATION_ITEM('')
);
#260=(
BOUNDED_CURVE()
B_SPLINE_CURVE(2,(#27128,#27129,#27130,#27131,#27132),.UNSPECIFIED.,.F.,
 .F.)
B_SPLINE_CURVE_WITH_KNOTS((3,2,3),(0.,0.25,0.459577358091283),
 .UNSPECIFIED.)
CURVE()
GEOMETRIC_REPRESENTATION_ITEM()
RATIONAL_B_SPLINE_CURVE((1.,0.974927912181824,1.,0.978981832292936,0.9932031210656))
REPRESENTATION_ITEM('')
);
#261=(
BOUNDED_CURVE()
B_SPLINE_CURVE(2,(#27211,#27212,#27213,#27214,#27215),.UNSPECIFIED.,.F.,
 .F.)
B_SPLINE_CURVE_WITH_KNOTS((3,2,3),(0.,0.25,0.460808762537664),
 .UNSPECIFIED.)
CURVE()
GEOMETRIC_REPRESENTATION_ITEM()
RATIONAL_B_SPLINE_CURVE((1.,0.974927912181824,1.,0.978858336771258,0.993371456448429))
REPRESENTATION_ITEM('')
);
#262=(
BOUNDED_CURVE()
B_SPLINE_CURVE(2,(#27253,#27254,#27255,#27256,#27257),.UNSPECIFIED.,.F.,
 .F.)
B_SPLINE_CURVE_WITH_KNOTS((3,2,3),(0.,0.25,0.459577358091283),
 .UNSPECIFIED.)
CURVE()
GEOMETRIC_REPRESENTATION_ITEM()
RATIONAL_B_SPLINE_CURVE((1.,0.974927912181824,1.,0.978981832292936,0.9932031210656))
REPRESENTATION_ITEM('')
);
#263=(
BOUNDED_CURVE()
B_SPLINE_CURVE(2,(#27336,#27337,#27338,#27339,#27340),.UNSPECIFIED.,.F.,
 .F.)
B_SPLINE_CURVE_WITH_KNOTS((3,2,3),(0.,0.25,0.460808762537663),
 .UNSPECIFIED.)
CURVE()
GEOMETRIC_REPRESENTATION_ITEM()
RATIONAL_B_SPLINE_CURVE((1.,0.974927912181824,1.,0.978858336771258,0.993371456448429))
REPRESENTATION_ITEM('')
);
#264=(
BOUNDED_CURVE()
B_SPLINE_CURVE(2,(#27378,#27379,#27380,#27381,#27382),.UNSPECIFIED.,.F.,
 .F.)
B_SPLINE_CURVE_WITH_KNOTS((3,2,3),(0.,0.25,0.459577358091282),
 .UNSPECIFIED.)
CURVE()
GEOMETRIC_REPRESENTATION_ITEM()
RATIONAL_B_SPLINE_CURVE((1.,0.974927912181824,1.,0.978981832292936,0.9932031210656))
REPRESENTATION_ITEM('')
);
#265=(
BOUNDED_CURVE()
B_SPLINE_CURVE(2,(#27550,#27551,#27552,#27553,#27554),.UNSPECIFIED.,.F.,
 .F.)
B_SPLINE_CURVE_WITH_KNOTS((3,2,3),(0.,0.25,0.459577358091282),
 .UNSPECIFIED.)
CURVE()
GEOMETRIC_REPRESENTATION_ITEM()
RATIONAL_B_SPLINE_CURVE((1.,0.974927912181824,1.,0.978981832292936,0.9932031210656))
REPRESENTATION_ITEM('')
);
#266=(
BOUNDED_CURVE()
B_SPLINE_CURVE(2,(#27722,#27723,#27724,#27725,#27726),.UNSPECIFIED.,.F.,
 .F.)
B_SPLINE_CURVE_WITH_KNOTS((3,2,3),(0.,0.25,0.459577358091282),
 .UNSPECIFIED.)
CURVE()
GEOMETRIC_REPRESENTATION_ITEM()
RATIONAL_B_SPLINE_CURVE((1.,0.974927912181824,1.,0.978981832292936,0.9932031210656))
REPRESENTATION_ITEM('')
);
#267=(
BOUNDED_CURVE()
B_SPLINE_CURVE(2,(#27894,#27895,#27896,#27897,#27898),.UNSPECIFIED.,.F.,
 .F.)
B_SPLINE_CURVE_WITH_KNOTS((3,2,3),(0.,0.25,0.459577358091282),
 .UNSPECIFIED.)
CURVE()
GEOMETRIC_REPRESENTATION_ITEM()
RATIONAL_B_SPLINE_CURVE((1.,0.974927912181824,1.,0.978981832292936,0.9932031210656))
REPRESENTATION_ITEM('')
);
#268=(
BOUNDED_CURVE()
B_SPLINE_CURVE(2,(#28066,#28067,#28068,#28069,#28070),.UNSPECIFIED.,.F.,
 .F.)
B_SPLINE_CURVE_WITH_KNOTS((3,2,3),(0.,0.25,0.459577358091282),
 .UNSPECIFIED.)
CURVE()
GEOMETRIC_REPRESENTATION_ITEM()
RATIONAL_B_SPLINE_CURVE((1.,0.974927912181824,1.,0.978981832292936,0.9932031210656))
REPRESENTATION_ITEM('')
);
#269=(
BOUNDED_CURVE()
B_SPLINE_CURVE(2,(#28238,#28239,#28240,#28241,#28242),.UNSPECIFIED.,.F.,
 .F.)
B_SPLINE_CURVE_WITH_KNOTS((3,2,3),(0.,0.25,0.459577358091282),
 .UNSPECIFIED.)
CURVE()
GEOMETRIC_REPRESENTATION_ITEM()
RATIONAL_B_SPLINE_CURVE((1.,0.974927912181824,1.,0.978981832292936,0.9932031210656))
REPRESENTATION_ITEM('')
);
#270=(
BOUNDED_CURVE()
B_SPLINE_CURVE(2,(#28410,#28411,#28412,#28413,#28414),.UNSPECIFIED.,.F.,
 .F.)
B_SPLINE_CURVE_WITH_KNOTS((3,2,3),(0.,0.25,0.459577358091283),
 .UNSPECIFIED.)
CURVE()
GEOMETRIC_REPRESENTATION_ITEM()
RATIONAL_B_SPLINE_CURVE((1.,0.974927912181824,1.,0.978981832292936,0.9932031210656))
REPRESENTATION_ITEM('')
);
#271=(
BOUNDED_CURVE()
B_SPLINE_CURVE(2,(#28493,#28494,#28495,#28496,#28497),.UNSPECIFIED.,.F.,
 .F.)
B_SPLINE_CURVE_WITH_KNOTS((3,2,3),(0.,0.25,0.460808762537662),
 .UNSPECIFIED.)
CURVE()
GEOMETRIC_REPRESENTATION_ITEM()
RATIONAL_B_SPLINE_CURVE((1.,0.974927912181824,1.,0.978858336771259,0.993371456448429))
REPRESENTATION_ITEM('')
);
#272=(
BOUNDED_CURVE()
B_SPLINE_CURVE(2,(#28535,#28536,#28537,#28538,#28539),.UNSPECIFIED.,.F.,
 .F.)
B_SPLINE_CURVE_WITH_KNOTS((3,2,3),(0.,0.25,0.459577358091282),
 .UNSPECIFIED.)
CURVE()
GEOMETRIC_REPRESENTATION_ITEM()
RATIONAL_B_SPLINE_CURVE((1.,0.974927912181824,1.,0.978981832292936,0.9932031210656))
REPRESENTATION_ITEM('')
);
#273=(
BOUNDED_CURVE()
B_SPLINE_CURVE(2,(#28618,#28619,#28620,#28621,#28622),.UNSPECIFIED.,.F.,
 .F.)
B_SPLINE_CURVE_WITH_KNOTS((3,2,3),(0.,0.25,0.460808762537662),
 .UNSPECIFIED.)
CURVE()
GEOMETRIC_REPRESENTATION_ITEM()
RATIONAL_B_SPLINE_CURVE((1.,0.974927912181824,1.,0.978858336771259,0.993371456448429))
REPRESENTATION_ITEM('')
);
#274=(
BOUNDED_CURVE()
B_SPLINE_CURVE(2,(#28660,#28661,#28662,#28663,#28664),.UNSPECIFIED.,.F.,
 .F.)
B_SPLINE_CURVE_WITH_KNOTS((3,2,3),(0.,0.25,0.459577358091282),
 .UNSPECIFIED.)
CURVE()
GEOMETRIC_REPRESENTATION_ITEM()
RATIONAL_B_SPLINE_CURVE((1.,0.974927912181824,1.,0.978981832292936,0.9932031210656))
REPRESENTATION_ITEM('')
);
#275=(
BOUNDED_CURVE()
B_SPLINE_CURVE(2,(#28832,#28833,#28834,#28835,#28836),.UNSPECIFIED.,.F.,
 .F.)
B_SPLINE_CURVE_WITH_KNOTS((3,2,3),(0.,0.25,0.459577358091282),
 .UNSPECIFIED.)
CURVE()
GEOMETRIC_REPRESENTATION_ITEM()
RATIONAL_B_SPLINE_CURVE((1.,0.974927912181824,1.,0.978981832292936,0.9932031210656))
REPRESENTATION_ITEM('')
);
#276=(
BOUNDED_CURVE()
B_SPLINE_CURVE(2,(#29004,#29005,#29006,#29007,#29008),.UNSPECIFIED.,.F.,
 .F.)
B_SPLINE_CURVE_WITH_KNOTS((3,2,3),(0.,0.25,0.459577358091281),
 .UNSPECIFIED.)
CURVE()
GEOMETRIC_REPRESENTATION_ITEM()
RATIONAL_B_SPLINE_CURVE((1.,0.974927912181824,1.,0.978981832292936,0.9932031210656))
REPRESENTATION_ITEM('')
);
#277=(
BOUNDED_CURVE()
B_SPLINE_CURVE(2,(#29086,#29087,#29088,#29089,#29090),.UNSPECIFIED.,.F.,
 .F.)
B_SPLINE_CURVE_WITH_KNOTS((3,2,3),(0.,0.0714285714285714,0.131307816597586),
 .UNSPECIFIED.)
CURVE()
GEOMETRIC_REPRESENTATION_ITEM()
RATIONAL_B_SPLINE_CURVE((1.,0.974927912181824,1.,0.978981832292909,0.993203121065636))
REPRESENTATION_ITEM('')
);
#278=(
BOUNDED_CURVE()
B_SPLINE_CURVE(2,(#29130,#29131,#29132,#29133,#29134),.UNSPECIFIED.,.F.,
 .F.)
B_SPLINE_CURVE_WITH_KNOTS((3,2,3),(0.,0.0714285714285714,0.131659646439332),
 .UNSPECIFIED.)
CURVE()
GEOMETRIC_REPRESENTATION_ITEM()
RATIONAL_B_SPLINE_CURVE((1.,0.974927912181824,1.,0.978858336771259,0.993371456448429))
REPRESENTATION_ITEM('')
);
#279=(
BOUNDED_CURVE()
B_SPLINE_CURVE(2,(#29301,#29302,#29303,#29304,#29305),.UNSPECIFIED.,.F.,
 .F.)
B_SPLINE_CURVE_WITH_KNOTS((3,2,3),(0.,0.25,0.459577358091283),
 .UNSPECIFIED.)
CURVE()
GEOMETRIC_REPRESENTATION_ITEM()
RATIONAL_B_SPLINE_CURVE((1.,0.974927912181824,1.,0.978981832292936,0.9932031210656))
REPRESENTATION_ITEM('')
);
#280=(
BOUNDED_CURVE()
B_SPLINE_CURVE(2,(#29473,#29474,#29475,#29476,#29477),.UNSPECIFIED.,.F.,
 .F.)
B_SPLINE_CURVE_WITH_KNOTS((3,2,3),(0.,0.25,0.459577358091283),
 .UNSPECIFIED.)
CURVE()
GEOMETRIC_REPRESENTATION_ITEM()
RATIONAL_B_SPLINE_CURVE((1.,0.974927912181824,1.,0.978981832292936,0.9932031210656))
REPRESENTATION_ITEM('')
);
#281=(
BOUNDED_CURVE()
B_SPLINE_CURVE(2,(#29645,#29646,#29647,#29648,#29649),.UNSPECIFIED.,.F.,
 .F.)
B_SPLINE_CURVE_WITH_KNOTS((3,2,3),(0.,0.25,0.459577358091282),
 .UNSPECIFIED.)
CURVE()
GEOMETRIC_REPRESENTATION_ITEM()
RATIONAL_B_SPLINE_CURVE((1.,0.974927912181824,1.,0.978981832292936,0.9932031210656))
REPRESENTATION_ITEM('')
);
#282=(
BOUNDED_CURVE()
B_SPLINE_CURVE(2,(#29817,#29818,#29819,#29820,#29821),.UNSPECIFIED.,.F.,
 .F.)
B_SPLINE_CURVE_WITH_KNOTS((3,2,3),(0.,0.25,0.459577358091283),
 .UNSPECIFIED.)
CURVE()
GEOMETRIC_REPRESENTATION_ITEM()
RATIONAL_B_SPLINE_CURVE((1.,0.974927912181824,1.,0.978981832292936,0.9932031210656))
REPRESENTATION_ITEM('')
);
#283=(
BOUNDED_CURVE()
B_SPLINE_CURVE(2,(#29989,#29990,#29991,#29992,#29993),.UNSPECIFIED.,.F.,
 .F.)
B_SPLINE_CURVE_WITH_KNOTS((3,2,3),(0.,0.25,0.459577358091282),
 .UNSPECIFIED.)
CURVE()
GEOMETRIC_REPRESENTATION_ITEM()
RATIONAL_B_SPLINE_CURVE((1.,0.974927912181824,1.,0.978981832292936,0.9932031210656))
REPRESENTATION_ITEM('')
);
#284=(
BOUNDED_CURVE()
B_SPLINE_CURVE(2,(#30072,#30073,#30074,#30075,#30076),.UNSPECIFIED.,.F.,
 .F.)
B_SPLINE_CURVE_WITH_KNOTS((3,2,3),(0.,0.25,0.460808762537663),
 .UNSPECIFIED.)
CURVE()
GEOMETRIC_REPRESENTATION_ITEM()
RATIONAL_B_SPLINE_CURVE((1.,0.974927912181824,1.,0.978858336771258,0.993371456448429))
REPRESENTATION_ITEM('')
);
#285=(
BOUNDED_CURVE()
B_SPLINE_CURVE(2,(#30114,#30115,#30116,#30117,#30118),.UNSPECIFIED.,.F.,
 .F.)
B_SPLINE_CURVE_WITH_KNOTS((3,2,3),(0.,0.25,0.459577358091282),
 .UNSPECIFIED.)
CURVE()
GEOMETRIC_REPRESENTATION_ITEM()
RATIONAL_B_SPLINE_CURVE((1.,0.974927912181824,1.,0.978981832292936,0.9932031210656))
REPRESENTATION_ITEM('')
);
#286=(
BOUNDED_CURVE()
B_SPLINE_CURVE(3,(#30215,#30216,#30217,#30218,#30219,#30220,#30221,#30222),
 .UNSPECIFIED.,.F.,.F.)
B_SPLINE_CURVE_WITH_KNOTS((4,2,2,4),(0.0783698352504338,0.308777376437326,
0.539184917624882,0.563918781515205),.UNSPECIFIED.)
CURVE()
GEOMETRIC_REPRESENTATION_ITEM()
RATIONAL_B_SPLINE_CURVE((1.,1.,1.,1.,1.,1.,1.,1.))
REPRESENTATION_ITEM('')
);
#287=(
BOUNDED_CURVE()
B_SPLINE_CURVE(3,(#30375,#30376,#30377,#30378,#30379,#30380,#30381,#30382),
 .UNSPECIFIED.,.F.,.F.)
B_SPLINE_CURVE_WITH_KNOTS((4,2,2,4),(0.0783698388401176,0.308777379129589,
0.539184919419725,0.563918783213387),.UNSPECIFIED.)
CURVE()
GEOMETRIC_REPRESENTATION_ITEM()
RATIONAL_B_SPLINE_CURVE((1.,1.,1.,1.,1.,1.,1.,1.))
REPRESENTATION_ITEM('')
);
#288=(
BOUNDED_CURVE()
B_SPLINE_CURVE(3,(#30721,#30722,#30723,#30724,#30725,#30726,#30727,#30728),
 .UNSPECIFIED.,.F.,.F.)
B_SPLINE_CURVE_WITH_KNOTS((4,2,2,4),(0.0783698481609191,0.30877738612019,
0.539184924080125,0.563918787623825),.UNSPECIFIED.)
CURVE()
GEOMETRIC_REPRESENTATION_ITEM()
RATIONAL_B_SPLINE_CURVE((1.,1.,1.,1.,1.,1.,1.,1.))
REPRESENTATION_ITEM('')
);
#289=(
BOUNDED_CURVE()
B_SPLINE_CURVE(3,(#30881,#30882,#30883,#30884,#30885,#30886,#30887,#30888),
 .UNSPECIFIED.,.F.,.F.)
B_SPLINE_CURVE_WITH_KNOTS((4,2,2,4),(0.0783698504851113,0.308777387863334,
0.539184925242222,0.563918788723451),.UNSPECIFIED.)
CURVE()
GEOMETRIC_REPRESENTATION_ITEM()
RATIONAL_B_SPLINE_CURVE((1.,1.,1.,1.,1.,1.,1.,1.))
REPRESENTATION_ITEM('')
);
#290=(
BOUNDED_CURVE()
B_SPLINE_CURVE(3,(#31041,#31042,#31043,#31044,#31045,#31046,#31047,#31048),
 .UNSPECIFIED.,.F.,.F.)
B_SPLINE_CURVE_WITH_KNOTS((4,2,2,4),(0.0783698504851048,0.308777387863329,
0.539184925242218,0.563918788723618),.UNSPECIFIED.)
CURVE()
GEOMETRIC_REPRESENTATION_ITEM()
RATIONAL_B_SPLINE_CURVE((1.,1.,1.,1.,1.,1.,1.,1.))
REPRESENTATION_ITEM('')
);
#291=(
BOUNDED_CURVE()
B_SPLINE_CURVE(3,(#31201,#31202,#31203,#31204,#31205,#31206,#31207,#31208),
 .UNSPECIFIED.,.F.,.F.)
B_SPLINE_CURVE_WITH_KNOTS((4,2,2,4),(0.0783698481609166,0.308777386120188,
0.539184924080124,0.563918787623731),.UNSPECIFIED.)
CURVE()
GEOMETRIC_REPRESENTATION_ITEM()
RATIONAL_B_SPLINE_CURVE((1.,1.,1.,1.,1.,1.,1.,1.))
REPRESENTATION_ITEM('')
);
#292=(
BOUNDED_CURVE()
B_SPLINE_CURVE(3,(#31361,#31362,#31363,#31364,#31365,#31366,#31367,#31368),
 .UNSPECIFIED.,.F.,.F.)
B_SPLINE_CURVE_WITH_KNOTS((4,2,2,4),(0.0783698437311068,0.308777382797831,
0.539184921865219,0.56391878552778),.UNSPECIFIED.)
CURVE()
GEOMETRIC_REPRESENTATION_ITEM()
RATIONAL_B_SPLINE_CURVE((1.,1.,1.,1.,1.,1.,1.,1.))
REPRESENTATION_ITEM('')
);
#293=(
BOUNDED_CURVE()
B_SPLINE_CURVE(3,(#31521,#31522,#31523,#31524,#31525,#31526,#31527,#31528),
 .UNSPECIFIED.,.F.,.F.)
B_SPLINE_CURVE_WITH_KNOTS((4,2,2,4),(0.078369838840124,0.308777379129593,
0.539184919419728,0.563918783213485),.UNSPECIFIED.)
CURVE()
GEOMETRIC_REPRESENTATION_ITEM()
RATIONAL_B_SPLINE_CURVE((1.,1.,1.,1.,1.,1.,1.,1.))
REPRESENTATION_ITEM('')
);
#294=(
BOUNDED_CURVE()
B_SPLINE_CURVE(3,(#31681,#31682,#31683,#31684,#31685,#31686,#31687,#31688),
 .UNSPECIFIED.,.F.,.F.)
B_SPLINE_CURVE_WITH_KNOTS((4,2,2,4),(0.0783698352504276,0.308777376437321,
0.539184917624879,0.563918781514921),.UNSPECIFIED.)
CURVE()
GEOMETRIC_REPRESENTATION_ITEM()
RATIONAL_B_SPLINE_CURVE((1.,1.,1.,1.,1.,1.,1.,1.))
REPRESENTATION_ITEM('')
);
#295=(
BOUNDED_CURVE()
B_SPLINE_CURVE(3,(#31841,#31842,#31843,#31844,#31845,#31846,#31847,#31848),
 .UNSPECIFIED.,.F.,.F.)
B_SPLINE_CURVE_WITH_KNOTS((4,2,2,4),(0.0783698293107417,0.308777371982557,
0.539184914655036,0.563918778704716),.UNSPECIFIED.)
CURVE()
GEOMETRIC_REPRESENTATION_ITEM()
RATIONAL_B_SPLINE_CURVE((1.,1.,1.,1.,1.,1.,1.,1.))
REPRESENTATION_ITEM('')
);
#296=(
BOUNDED_CURVE()
B_SPLINE_CURVE(3,(#32187,#32188,#32189,#32190,#32191,#32192,#32193,#32194),
 .UNSPECIFIED.,.F.,.F.)
B_SPLINE_CURVE_WITH_KNOTS((4,2,2,4),(0.0783698388401176,0.308777379129589,
0.539184919419725,0.563918783213641),.UNSPECIFIED.)
CURVE()
GEOMETRIC_REPRESENTATION_ITEM()
RATIONAL_B_SPLINE_CURVE((1.,1.,1.,1.,1.,1.,1.,1.))
REPRESENTATION_ITEM('')
);
#297=(
BOUNDED_CURVE()
B_SPLINE_CURVE(3,(#32347,#32348,#32349,#32350,#32351,#32352,#32353,#32354),
 .UNSPECIFIED.,.F.,.F.)
B_SPLINE_CURVE_WITH_KNOTS((4,2,2,4),(0.0783698437311062,0.30877738279783,
0.539184921865219,0.563918785528064),.UNSPECIFIED.)
CURVE()
GEOMETRIC_REPRESENTATION_ITEM()
RATIONAL_B_SPLINE_CURVE((1.,1.,1.,1.,1.,1.,1.,1.))
REPRESENTATION_ITEM('')
);
#298=(
BOUNDED_CURVE()
B_SPLINE_CURVE(3,(#32499,#32500,#32501,#32502,#32503,#32504,#32505,#32506),
 .UNSPECIFIED.,.F.,.F.)
B_SPLINE_CURVE_WITH_KNOTS((4,2,2,4),(0.0783698481609152,0.308777386120187,
0.539184924080123,0.563918787623673),.UNSPECIFIED.)
CURVE()
GEOMETRIC_REPRESENTATION_ITEM()
RATIONAL_B_SPLINE_CURVE((1.,1.,1.,1.,1.,1.,1.,1.))
REPRESENTATION_ITEM('')
);
#299=(
BOUNDED_CURVE()
B_SPLINE_CURVE(3,(#32667,#32668,#32669,#32670,#32671,#32672,#32673,#32674),
 .UNSPECIFIED.,.F.,.F.)
B_SPLINE_CURVE_WITH_KNOTS((4,2,2,4),(0.0783698504851105,0.308777387863333,
0.539184925242221,0.563918788723755),.UNSPECIFIED.)
CURVE()
GEOMETRIC_REPRESENTATION_ITEM()
RATIONAL_B_SPLINE_CURVE((1.,1.,1.,1.,1.,1.,1.,1.))
REPRESENTATION_ITEM('')
);
#300=(
BOUNDED_CURVE()
B_SPLINE_CURVE(3,(#32827,#32828,#32829,#32830,#32831,#32832,#32833,#32834),
 .UNSPECIFIED.,.F.,.F.)
B_SPLINE_CURVE_WITH_KNOTS((4,2,2,4),(0.0783698504851009,0.308777387863326,
0.539184925242216,0.563918788723615),.UNSPECIFIED.)
CURVE()
GEOMETRIC_REPRESENTATION_ITEM()
RATIONAL_B_SPLINE_CURVE((1.,1.,1.,1.,1.,1.,1.,1.))
REPRESENTATION_ITEM('')
);
#301=(
BOUNDED_CURVE()
B_SPLINE_CURVE(3,(#32987,#32988,#32989,#32990,#32991,#32992,#32993,#32994),
 .UNSPECIFIED.,.F.,.F.)
B_SPLINE_CURVE_WITH_KNOTS((4,2,2,4),(0.0783698481609159,0.308777386120187,
0.539184924080124,0.563918787623773),.UNSPECIFIED.)
CURVE()
GEOMETRIC_REPRESENTATION_ITEM()
RATIONAL_B_SPLINE_CURVE((1.,1.,1.,1.,1.,1.,1.,1.))
REPRESENTATION_ITEM('')
);
#302=(
BOUNDED_CURVE()
B_SPLINE_CURVE(3,(#33147,#33148,#33149,#33150,#33151,#33152,#33153,#33154),
 .UNSPECIFIED.,.F.,.F.)
B_SPLINE_CURVE_WITH_KNOTS((4,2,2,4),(0.0783698437310911,0.308777382797819,
0.539184921865211,0.563918785527635),.UNSPECIFIED.)
CURVE()
GEOMETRIC_REPRESENTATION_ITEM()
RATIONAL_B_SPLINE_CURVE((1.,1.,1.,1.,1.,1.,1.,1.))
REPRESENTATION_ITEM('')
);
#303=(
BOUNDED_CURVE()
B_SPLINE_CURVE(3,(#33307,#33308,#33309,#33310,#33311,#33312,#33313,#33314),
 .UNSPECIFIED.,.F.,.F.)
B_SPLINE_CURVE_WITH_KNOTS((4,2,2,4),(0.0783698388401225,0.308777379129592,
0.539184919419727,0.563918783213193),.UNSPECIFIED.)
CURVE()
GEOMETRIC_REPRESENTATION_ITEM()
RATIONAL_B_SPLINE_CURVE((1.,1.,1.,1.,1.,1.,1.,1.))
REPRESENTATION_ITEM('')
);
#304=(
BOUNDED_CURVE()
B_SPLINE_CURVE(3,(#33467,#33468,#33469,#33470,#33471,#33472,#33473,#33474),
 .UNSPECIFIED.,.F.,.F.)
B_SPLINE_CURVE_WITH_KNOTS((4,2,2,4),(0.078369835250435,0.308777376437327,
0.539184917624883,0.563918781515067),.UNSPECIFIED.)
CURVE()
GEOMETRIC_REPRESENTATION_ITEM()
RATIONAL_B_SPLINE_CURVE((1.,1.,1.,1.,1.,1.,1.,1.))
REPRESENTATION_ITEM('')
);
#305=(
BOUNDED_CURVE()
B_SPLINE_CURVE(3,(#33627,#33628,#33629,#33630,#33631,#33632,#33633,#33634),
 .UNSPECIFIED.,.F.,.F.)
B_SPLINE_CURVE_WITH_KNOTS((4,2,2,4),(0.0783698293107414,0.308777371982556,
0.539184914655036,0.563918778704657),.UNSPECIFIED.)
CURVE()
GEOMETRIC_REPRESENTATION_ITEM()
RATIONAL_B_SPLINE_CURVE((1.,1.,1.,1.,1.,1.,1.,1.))
REPRESENTATION_ITEM('')
);
#306=(
BOUNDED_CURVE()
B_SPLINE_CURVE(3,(#33787,#33788,#33789,#33790,#33791,#33792,#33793,#33794),
 .UNSPECIFIED.,.F.,.F.)
B_SPLINE_CURVE_WITH_KNOTS((4,2,2,4),(0.0783698352504223,0.308777376437317,
0.539184917624877,0.563918781514814),.UNSPECIFIED.)
CURVE()
GEOMETRIC_REPRESENTATION_ITEM()
RATIONAL_B_SPLINE_CURVE((1.,1.,1.,1.,1.,1.,1.,1.))
REPRESENTATION_ITEM('')
);
#307=(
BOUNDED_CURVE()
B_SPLINE_CURVE(3,(#33947,#33948,#33949,#33950,#33951,#33952,#33953,#33954),
 .UNSPECIFIED.,.F.,.F.)
B_SPLINE_CURVE_WITH_KNOTS((4,2,2,4),(0.0783698388401235,0.308777379129593,
0.539184919419728,0.563918783213176),.UNSPECIFIED.)
CURVE()
GEOMETRIC_REPRESENTATION_ITEM()
RATIONAL_B_SPLINE_CURVE((1.,1.,1.,1.,1.,1.,1.,1.))
REPRESENTATION_ITEM('')
);
#308=(
BOUNDED_CURVE()
B_SPLINE_CURVE(3,(#34479,#34480,#34481,#34482,#34483,#34484,#34485,#34486),
 .UNSPECIFIED.,.F.,.F.)
B_SPLINE_CURVE_WITH_KNOTS((4,2,2,4),(0.0783698504850856,0.308777387863315,
0.539184925242209,0.56391878872357),.UNSPECIFIED.)
CURVE()
GEOMETRIC_REPRESENTATION_ITEM()
RATIONAL_B_SPLINE_CURVE((1.,1.,1.,1.,1.,1.,1.,1.))
REPRESENTATION_ITEM('')
);
#309=(
BOUNDED_CURVE()
B_SPLINE_CURVE(3,(#34639,#34640,#34641,#34642,#34643,#34644,#34645,#34646),
 .UNSPECIFIED.,.F.,.F.)
B_SPLINE_CURVE_WITH_KNOTS((4,2,2,4),(0.0783698504851055,0.30877738786333,
0.539184925242219,0.563918788723501),.UNSPECIFIED.)
CURVE()
GEOMETRIC_REPRESENTATION_ITEM()
RATIONAL_B_SPLINE_CURVE((1.,1.,1.,1.,1.,1.,1.,1.))
REPRESENTATION_ITEM('')
);
#310=(
BOUNDED_CURVE()
B_SPLINE_CURVE(3,(#34799,#34800,#34801,#34802,#34803,#34804,#34805,#34806),
 .UNSPECIFIED.,.F.,.F.)
B_SPLINE_CURVE_WITH_KNOTS((4,2,2,4),(0.0783698481609002,0.308777386120176,
0.539184924080116,0.563918787623726),.UNSPECIFIED.)
CURVE()
GEOMETRIC_REPRESENTATION_ITEM()
RATIONAL_B_SPLINE_CURVE((1.,1.,1.,1.,1.,1.,1.,1.))
REPRESENTATION_ITEM('')
);
#311=(
BOUNDED_CURVE()
B_SPLINE_CURVE(3,(#34959,#34960,#34961,#34962,#34963,#34964,#34965,#34966),
 .UNSPECIFIED.,.F.,.F.)
B_SPLINE_CURVE_WITH_KNOTS((4,2,2,4),(0.0783698437310988,0.308777382797825,
0.539184921865215,0.563918785527758),.UNSPECIFIED.)
CURVE()
GEOMETRIC_REPRESENTATION_ITEM()
RATIONAL_B_SPLINE_CURVE((1.,1.,1.,1.,1.,1.,1.,1.))
REPRESENTATION_ITEM('')
);
#312=(
BOUNDED_CURVE()
B_SPLINE_CURVE(3,(#35119,#35120,#35121,#35122,#35123,#35124,#35125,#35126),
 .UNSPECIFIED.,.F.,.F.)
B_SPLINE_CURVE_WITH_KNOTS((4,2,2,4),(0.078369838840116,0.308777379129587,
0.539184919419724,0.563918783213258),.UNSPECIFIED.)
CURVE()
GEOMETRIC_REPRESENTATION_ITEM()
RATIONAL_B_SPLINE_CURVE((1.,1.,1.,1.,1.,1.,1.,1.))
REPRESENTATION_ITEM('')
);
#313=(
BOUNDED_CURVE()
B_SPLINE_CURVE(3,(#35279,#35280,#35281,#35282,#35283,#35284,#35285,#35286),
 .UNSPECIFIED.,.F.,.F.)
B_SPLINE_CURVE_WITH_KNOTS((4,2,2,4),(0.0783698352504284,0.308777376437322,
0.53918491762488,0.563918781514946),.UNSPECIFIED.)
CURVE()
GEOMETRIC_REPRESENTATION_ITEM()
RATIONAL_B_SPLINE_CURVE((1.,1.,1.,1.,1.,1.,1.,1.))
REPRESENTATION_ITEM('')
);
#314=(
BOUNDED_CURVE()
B_SPLINE_CURVE(3,(#35811,#35812,#35813,#35814,#35815,#35816,#35817,#35818),
 .UNSPECIFIED.,.F.,.F.)
B_SPLINE_CURVE_WITH_KNOTS((4,2,2,4),(0.078369838840114,0.308777379129586,
0.539184919419723,0.56391878321367),.UNSPECIFIED.)
CURVE()
GEOMETRIC_REPRESENTATION_ITEM()
RATIONAL_B_SPLINE_CURVE((1.,1.,1.,1.,1.,1.,1.,1.))
REPRESENTATION_ITEM('')
);
#315=(
BOUNDED_CURVE()
B_SPLINE_CURVE(3,(#35971,#35972,#35973,#35974,#35975,#35976,#35977,#35978),
 .UNSPECIFIED.,.F.,.F.)
B_SPLINE_CURVE_WITH_KNOTS((4,2,2,4),(0.078369843731106,0.30877738279783,
0.539184921865219,0.563918785527521),.UNSPECIFIED.)
CURVE()
GEOMETRIC_REPRESENTATION_ITEM()
RATIONAL_B_SPLINE_CURVE((1.,1.,1.,1.,1.,1.,1.,1.))
REPRESENTATION_ITEM('')
);
#316=(
BOUNDED_CURVE()
B_SPLINE_CURVE(3,(#36123,#36124,#36125,#36126,#36127,#36128,#36129,#36130),
 .UNSPECIFIED.,.F.,.F.)
B_SPLINE_CURVE_WITH_KNOTS((4,2,2,4),(0.0783698481609171,0.308777386120188,
0.539184924080125,0.563918787623751),.UNSPECIFIED.)
CURVE()
GEOMETRIC_REPRESENTATION_ITEM()
RATIONAL_B_SPLINE_CURVE((1.,1.,1.,1.,1.,1.,1.,1.))
REPRESENTATION_ITEM('')
);
#317=(
BOUNDED_CURVE()
B_SPLINE_CURVE(3,(#36291,#36292,#36293,#36294,#36295,#36296,#36297,#36298),
 .UNSPECIFIED.,.F.,.F.)
B_SPLINE_CURVE_WITH_KNOTS((4,2,2,4),(0.0783698504850854,0.308777387863314,
0.539184925242208,0.563918788723659),.UNSPECIFIED.)
CURVE()
GEOMETRIC_REPRESENTATION_ITEM()
RATIONAL_B_SPLINE_CURVE((1.,1.,1.,1.,1.,1.,1.,1.))
REPRESENTATION_ITEM('')
);
#318=(
BOUNDED_CURVE()
B_SPLINE_CURVE(3,(#36451,#36452,#36453,#36454,#36455,#36456,#36457,#36458),
 .UNSPECIFIED.,.F.,.F.)
B_SPLINE_CURVE_WITH_KNOTS((4,2,2,4),(0.0783698504851048,0.308777387863329,
0.539184925242218,0.563918788723504),.UNSPECIFIED.)
CURVE()
GEOMETRIC_REPRESENTATION_ITEM()
RATIONAL_B_SPLINE_CURVE((1.,1.,1.,1.,1.,1.,1.,1.))
REPRESENTATION_ITEM('')
);
#319=(
BOUNDED_CURVE()
B_SPLINE_CURVE(3,(#36611,#36612,#36613,#36614,#36615,#36616,#36617,#36618),
 .UNSPECIFIED.,.F.,.F.)
B_SPLINE_CURVE_WITH_KNOTS((4,2,2,4),(0.0783698481609187,0.30877738612019,
0.539184924080125,0.563918787623611),.UNSPECIFIED.)
CURVE()
GEOMETRIC_REPRESENTATION_ITEM()
RATIONAL_B_SPLINE_CURVE((1.,1.,1.,1.,1.,1.,1.,1.))
REPRESENTATION_ITEM('')
);
#320=(
BOUNDED_CURVE()
B_SPLINE_CURVE(3,(#36771,#36772,#36773,#36774,#36775,#36776,#36777,#36778),
 .UNSPECIFIED.,.F.,.F.)
B_SPLINE_CURVE_WITH_KNOTS((4,2,2,4),(0.0783698437311103,0.308777382797833,
0.539184921865221,0.563918785527852),.UNSPECIFIED.)
CURVE()
GEOMETRIC_REPRESENTATION_ITEM()
RATIONAL_B_SPLINE_CURVE((1.,1.,1.,1.,1.,1.,1.,1.))
REPRESENTATION_ITEM('')
);
#321=(
BOUNDED_CURVE()
B_SPLINE_CURVE(3,(#36931,#36932,#36933,#36934,#36935,#36936,#36937,#36938),
 .UNSPECIFIED.,.F.,.F.)
B_SPLINE_CURVE_WITH_KNOTS((4,2,2,4),(0.0783698388401129,0.308777379129585,
0.539184919419723,0.563918783213525),.UNSPECIFIED.)
CURVE()
GEOMETRIC_REPRESENTATION_ITEM()
RATIONAL_B_SPLINE_CURVE((1.,1.,1.,1.,1.,1.,1.,1.))
REPRESENTATION_ITEM('')
);
#322=(
BOUNDED_SURFACE()
B_SPLINE_SURFACE(1,2,((#14934,#14935,#14936,#14937,#14938,#14939,#14940,
#14941,#14942,#14943,#14944,#14945,#14946,#14947,#14948,#14949,#14950,#14951,
#14952,#14953,#14954,#14955,#14956,#14957,#14958,#14959,#14960,#14961,#14962,
#14963,#14964,#14965,#14966,#14967,#14968,#14969,#14970,#14971,#14972,#14973,
#14974,#14975,#14976,#14977,#14978,#14979,#14980,#14981,#14982,#14983,#14984,
#14985,#14986,#14987,#14988,#14989,#14990,#14991,#14992,#14993,#14994,#14995,
#14996,#14997,#14998,#14999,#15000,#15001,#15002,#15003,#15004,#15005,#15006,
#15007,#15008,#15009,#15010,#15011,#15012,#15013,#15014,#15015,#15016,#15017,
#15018,#15019,#15020,#15021,#15022,#15023,#15024,#15025,#15026,#15027,#15028,
#15029,#15030,#15031,#15032,#15033,#15034,#15035,#15036,#15037,#15038,#15039,
#15040,#15041,#15042,#15043,#15044,#15045,#15046),(#15047,#15048,#15049,
#15050,#15051,#15052,#15053,#15054,#15055,#15056,#15057,#15058,#15059,#15060,
#15061,#15062,#15063,#15064,#15065,#15066,#15067,#15068,#15069,#15070,#15071,
#15072,#15073,#15074,#15075,#15076,#15077,#15078,#15079,#15080,#15081,#15082,
#15083,#15084,#15085,#15086,#15087,#15088,#15089,#15090,#15091,#15092,#15093,
#15094,#15095,#15096,#15097,#15098,#15099,#15100,#15101,#15102,#15103,#15104,
#15105,#15106,#15107,#15108,#15109,#15110,#15111,#15112,#15113,#15114,#15115,
#15116,#15117,#15118,#15119,#15120,#15121,#15122,#15123,#15124,#15125,#15126,
#15127,#15128,#15129,#15130,#15131,#15132,#15133,#15134,#15135,#15136,#15137,
#15138,#15139,#15140,#15141,#15142,#15143,#15144,#15145,#15146,#15147,#15148,
#15149,#15150,#15151,#15152,#15153,#15154,#15155,#15156,#15157,#15158,#15159)),
 .UNSPECIFIED.,.F.,.F.,.F.)
B_SPLINE_SURFACE_WITH_KNOTS((2,2),(3,2,2,2,2,2,2,2,2,2,2,2,2,2,2,2,2,2,
2,2,2,2,2,2,2,2,2,2,2,2,2,2,2,2,2,2,2,2,2,2,2,2,2,2,2,2,2,2,2,2,2,2,2,2,
2,2,3),(0.,1.),(0.,0.0178571428571429,0.0357142857142857,0.0535714285714286,
0.0714285714285714,0.0892857142857143,0.107142857142857,0.125,0.142857142857143,
0.160714285714286,0.178571428571429,0.196428571428571,0.214285714285714,
0.232142857142857,0.25,0.267857142857143,0.285714285714286,0.303571428571429,
0.321428571428571,0.339285714285714,0.357142857142857,0.375,0.392857142857143,
0.410714285714286,0.428571428571429,0.446428571428571,0.464285714285714,
0.482142857142857,0.5,0.517857142857143,0.535714285714286,0.553571428571429,
0.571428571428571,0.589285714285714,0.607142857142857,0.625,0.642857142857143,
0.660714285714286,0.678571428571429,0.696428571428571,0.714285714285714,
0.732142857142857,0.75,0.767857142857143,0.785714285714286,0.803571428571429,
0.821428571428571,0.839285714285714,0.857142857142857,0.875,0.892857142857143,
0.910714285714286,0.928571428571429,0.946428571428571,0.964285714285714,
0.982142857142857,1.),.UNSPECIFIED.)
GEOMETRIC_REPRESENTATION_ITEM()
RATIONAL_B_SPLINE_SURFACE(((1.,0.974927912181824,1.,0.974927912181824,1.,
0.974927912181824,1.,0.974927912181824,1.,0.974927912181824,1.,0.974927912181824,
1.,0.974927912181824,1.,0.974927912181824,1.,0.974927912181824,1.,0.974927912181824,
1.,0.974927912181824,1.,0.974927912181824,1.,0.974927912181824,1.,0.974927912181824,
1.,0.974927912181824,1.,0.974927912181824,1.,0.974927912181824,1.,0.974927912181824,
1.,0.974927912181824,1.,0.974927912181824,1.,0.974927912181824,1.,0.974927912181824,
1.,0.974927912181824,1.,0.974927912181824,1.,0.974927912181824,1.,0.974927912181824,
1.,0.974927912181824,1.,0.974927912181824,1.,0.974927912181824,1.,0.974927912181824,
1.,0.974927912181824,1.,0.974927912181824,1.,0.974927912181824,1.,0.974927912181824,
1.,0.974927912181824,1.,0.974927912181824,1.,0.974927912181824,1.,0.974927912181824,
1.,0.974927912181824,1.,0.974927912181824,1.,0.974927912181824,1.,0.974927912181824,
1.,0.974927912181824,1.,0.974927912181824,1.,0.974927912181824,1.,0.974927912181824,
1.,0.974927912181824,1.,0.974927912181824,1.,0.974927912181824,1.,0.974927912181824,
1.,0.974927912181824,1.,0.974927912181824,1.,0.974927912181824,1.,0.974927912181824,
1.,0.974927912181824,1.,0.974927912181824,1.),(1.,0.974927912181824,1.,
0.974927912181824,1.,0.974927912181824,1.,0.974927912181824,1.,0.974927912181824,
1.,0.974927912181824,1.,0.974927912181824,1.,0.974927912181824,1.,0.974927912181824,
1.,0.974927912181824,1.,0.974927912181824,1.,0.974927912181824,1.,0.974927912181824,
1.,0.974927912181824,1.,0.974927912181824,1.,0.974927912181824,1.,0.974927912181824,
1.,0.974927912181824,1.,0.974927912181824,1.,0.974927912181824,1.,0.974927912181824,
1.,0.974927912181824,1.,0.974927912181824,1.,0.974927912181824,1.,0.974927912181824,
1.,0.974927912181824,1.,0.974927912181824,1.,0.974927912181824,1.,0.974927912181824,
1.,0.974927912181824,1.,0.974927912181824,1.,0.974927912181824,1.,0.974927912181824,
1.,0.974927912181824,1.,0.974927912181824,1.,0.974927912181824,1.,0.974927912181824,
1.,0.974927912181824,1.,0.974927912181824,1.,0.974927912181824,1.,0.974927912181824,
1.,0.974927912181824,1.,0.974927912181824,1.,0.974927912181824,1.,0.974927912181824,
1.,0.974927912181824,1.,0.974927912181824,1.,0.974927912181824,1.,0.974927912181824,
1.,0.974927912181824,1.,0.974927912181824,1.,0.974927912181824,1.,0.974927912181824,
1.,0.974927912181824,1.,0.974927912181824,1.,0.974927912181824,1.)))
REPRESENTATION_ITEM('')
SURFACE()
);
#323=(
BOUNDED_SURFACE()
B_SPLINE_SURFACE(3,2,((#15275,#15276,#15277,#15278,#15279,#15280,#15281,
#15282,#15283,#15284,#15285,#15286,#15287,#15288,#15289,#15290,#15291,#15292,
#15293,#15294,#15295,#15296,#15297,#15298,#15299,#15300,#15301,#15302,#15303,
#15304,#15305,#15306,#15307,#15308,#15309,#15310,#15311,#15312,#15313,#15314,
#15315,#15316,#15317,#15318,#15319,#15320,#15321,#15322,#15323,#15324,#15325,
#15326,#15327,#15328,#15329,#15330,#15331,#15332,#15333,#15334,#15335,#15336,
#15337,#15338,#15339,#15340,#15341,#15342,#15343,#15344,#15345,#15346,#15347,
#15348,#15349,#15350,#15351,#15352,#15353,#15354,#15355,#15356,#15357,#15358,
#15359,#15360,#15361,#15362,#15363,#15364,#15365,#15366,#15367,#15368,#15369,
#15370,#15371,#15372,#15373,#15374,#15375,#15376,#15377,#15378,#15379,#15380,
#15381,#15382,#15383,#15384,#15385,#15386,#15387),(#15388,#15389,#15390,
#15391,#15392,#15393,#15394,#15395,#15396,#15397,#15398,#15399,#15400,#15401,
#15402,#15403,#15404,#15405,#15406,#15407,#15408,#15409,#15410,#15411,#15412,
#15413,#15414,#15415,#15416,#15417,#15418,#15419,#15420,#15421,#15422,#15423,
#15424,#15425,#15426,#15427,#15428,#15429,#15430,#15431,#15432,#15433,#15434,
#15435,#15436,#15437,#15438,#15439,#15440,#15441,#15442,#15443,#15444,#15445,
#15446,#15447,#15448,#15449,#15450,#15451,#15452,#15453,#15454,#15455,#15456,
#15457,#15458,#15459,#15460,#15461,#15462,#15463,#15464,#15465,#15466,#15467,
#15468,#15469,#15470,#15471,#15472,#15473,#15474,#15475,#15476,#15477,#15478,
#15479,#15480,#15481,#15482,#15483,#15484,#15485,#15486,#15487,#15488,#15489,
#15490,#15491,#15492,#15493,#15494,#15495,#15496,#15497,#15498,#15499,#15500),
(#15501,#15502,#15503,#15504,#15505,#15506,#15507,#15508,#15509,#15510,
#15511,#15512,#15513,#15514,#15515,#15516,#15517,#15518,#15519,#15520,#15521,
#15522,#15523,#15524,#15525,#15526,#15527,#15528,#15529,#15530,#15531,#15532,
#15533,#15534,#15535,#15536,#15537,#15538,#15539,#15540,#15541,#15542,#15543,
#15544,#15545,#15546,#15547,#15548,#15549,#15550,#15551,#15552,#15553,#15554,
#15555,#15556,#15557,#15558,#15559,#15560,#15561,#15562,#15563,#15564,#15565,
#15566,#15567,#15568,#15569,#15570,#15571,#15572,#15573,#15574,#15575,#15576,
#15577,#15578,#15579,#15580,#15581,#15582,#15583,#15584,#15585,#15586,#15587,
#15588,#15589,#15590,#15591,#15592,#15593,#15594,#15595,#15596,#15597,#15598,
#15599,#15600,#15601,#15602,#15603,#15604,#15605,#15606,#15607,#15608,#15609,
#15610,#15611,#15612,#15613),(#15614,#15615,#15616,#15617,#15618,#15619,
#15620,#15621,#15622,#15623,#15624,#15625,#15626,#15627,#15628,#15629,#15630,
#15631,#15632,#15633,#15634,#15635,#15636,#15637,#15638,#15639,#15640,#15641,
#15642,#15643,#15644,#15645,#15646,#15647,#15648,#15649,#15650,#15651,#15652,
#15653,#15654,#15655,#15656,#15657,#15658,#15659,#15660,#15661,#15662,#15663,
#15664,#15665,#15666,#15667,#15668,#15669,#15670,#15671,#15672,#15673,#15674,
#15675,#15676,#15677,#15678,#15679,#15680,#15681,#15682,#15683,#15684,#15685,
#15686,#15687,#15688,#15689,#15690,#15691,#15692,#15693,#15694,#15695,#15696,
#15697,#15698,#15699,#15700,#15701,#15702,#15703,#15704,#15705,#15706,#15707,
#15708,#15709,#15710,#15711,#15712,#15713,#15714,#15715,#15716,#15717,#15718,
#15719,#15720,#15721,#15722,#15723,#15724,#15725,#15726)),.UNSPECIFIED.,
 .F.,.F.,.F.)
B_SPLINE_SURFACE_WITH_KNOTS((4,4),(3,2,2,2,2,2,2,2,2,2,2,2,2,2,2,2,2,2,
2,2,2,2,2,2,2,2,2,2,2,2,2,2,2,2,2,2,2,2,2,2,2,2,2,2,2,2,2,2,2,2,2,2,2,2,
2,2,3),(0.,1.),(0.,0.0178571428571429,0.0357142857142857,0.0535714285714286,
0.0714285714285714,0.0892857142857143,0.107142857142857,0.125,0.142857142857143,
0.160714285714286,0.178571428571429,0.196428571428571,0.214285714285714,
0.232142857142857,0.25,0.267857142857143,0.285714285714286,0.303571428571429,
0.321428571428571,0.339285714285714,0.357142857142857,0.375,0.392857142857143,
0.410714285714286,0.428571428571429,0.446428571428571,0.464285714285714,
0.482142857142857,0.5,0.517857142857143,0.535714285714286,0.553571428571429,
0.571428571428571,0.589285714285714,0.607142857142857,0.625,0.642857142857143,
0.660714285714286,0.678571428571429,0.696428571428571,0.714285714285714,
0.732142857142857,0.75,0.767857142857143,0.785714285714286,0.803571428571429,
0.821428571428571,0.839285714285714,0.857142857142857,0.875,0.892857142857143,
0.910714285714286,0.928571428571429,0.946428571428571,0.964285714285714,
0.982142857142857,1.),.UNSPECIFIED.)
GEOMETRIC_REPRESENTATION_ITEM()
RATIONAL_B_SPLINE_SURFACE(((1.,0.974927912181824,1.,0.974927912181824,1.,
0.974927912181824,1.,0.974927912181824,1.,0.974927912181824,1.,0.974927912181824,
1.,0.974927912181824,1.,0.974927912181824,1.,0.974927912181824,1.,0.974927912181824,
1.,0.974927912181824,1.,0.974927912181824,1.,0.974927912181824,1.,0.974927912181824,
1.,0.974927912181824,1.,0.974927912181824,1.,0.974927912181824,1.,0.974927912181824,
1.,0.974927912181824,1.,0.974927912181824,1.,0.974927912181824,1.,0.974927912181824,
1.,0.974927912181824,1.,0.974927912181824,1.,0.974927912181824,1.,0.974927912181824,
1.,0.974927912181824,1.,0.974927912181824,1.,0.974927912181824,1.,0.974927912181824,
1.,0.974927912181824,1.,0.974927912181824,1.,0.974927912181824,1.,0.974927912181824,
1.,0.974927912181824,1.,0.974927912181824,1.,0.974927912181824,1.,0.974927912181824,
1.,0.974927912181824,1.,0.974927912181824,1.,0.974927912181824,1.,0.974927912181824,
1.,0.974927912181824,1.,0.974927912181824,1.,0.974927912181824,1.,0.974927912181824,
1.,0.974927912181824,1.,0.974927912181824,1.,0.974927912181824,1.,0.974927912181824,
1.,0.974927912181824,1.,0.974927912181824,1.,0.974927912181824,1.,0.974927912181824,
1.,0.974927912181824,1.,0.974927912181824,1.),(0.49408353936993,0.481695833481332,
0.49408353936993,0.481695833481332,0.49408353936993,0.481695833481332,0.49408353936993,
0.481695833481332,0.49408353936993,0.481695833481332,0.49408353936993,0.481695833481332,
0.49408353936993,0.481695833481332,0.49408353936993,0.481695833481332,0.49408353936993,
0.481695833481332,0.49408353936993,0.481695833481332,0.49408353936993,0.481695833481332,
0.49408353936993,0.481695833481332,0.49408353936993,0.481695833481332,0.49408353936993,
0.481695833481332,0.49408353936993,0.481695833481332,0.49408353936993,0.481695833481332,
0.49408353936993,0.481695833481332,0.49408353936993,0.481695833481332,0.49408353936993,
0.481695833481332,0.49408353936993,0.481695833481332,0.49408353936993,0.481695833481332,
0.49408353936993,0.481695833481332,0.49408353936993,0.481695833481332,0.49408353936993,
0.481695833481332,0.49408353936993,0.481695833481332,0.49408353936993,0.481695833481332,
0.49408353936993,0.481695833481332,0.49408353936993,0.481695833481332,0.49408353936993,
0.481695833481332,0.49408353936993,0.481695833481332,0.49408353936993,0.481695833481332,
0.49408353936993,0.481695833481332,0.49408353936993,0.481695833481332,0.49408353936993,
0.481695833481332,0.49408353936993,0.481695833481332,0.49408353936993,0.481695833481332,
0.49408353936993,0.481695833481332,0.49408353936993,0.481695833481332,0.49408353936993,
0.481695833481332,0.49408353936993,0.481695833481332,0.49408353936993,0.481695833481332,
0.49408353936993,0.481695833481332,0.49408353936993,0.481695833481332,0.49408353936993,
0.481695833481332,0.49408353936993,0.481695833481332,0.49408353936993,0.481695833481332,
0.49408353936993,0.481695833481332,0.49408353936993,0.481695833481332,0.49408353936993,
0.481695833481332,0.49408353936993,0.481695833481332,0.49408353936993,0.481695833481332,
0.49408353936993,0.481695833481332,0.49408353936993,0.481695833481332,0.49408353936993,
0.481695833481332,0.49408353936993,0.481695833481332,0.49408353936993,0.481695833481332,
0.49408353936993),(0.49408353936993,0.481695833481332,0.49408353936993,
0.481695833481332,0.49408353936993,0.481695833481332,0.49408353936993,0.481695833481332,
0.49408353936993,0.481695833481332,0.49408353936993,0.481695833481332,0.49408353936993,
0.481695833481332,0.49408353936993,0.481695833481332,0.49408353936993,0.481695833481332,
0.49408353936993,0.481695833481332,0.49408353936993,0.481695833481332,0.49408353936993,
0.481695833481332,0.49408353936993,0.481695833481332,0.49408353936993,0.481695833481332,
0.49408353936993,0.481695833481332,0.49408353936993,0.481695833481332,0.49408353936993,
0.481695833481332,0.49408353936993,0.481695833481332,0.49408353936993,0.481695833481332,
0.49408353936993,0.481695833481332,0.49408353936993,0.481695833481332,0.49408353936993,
0.481695833481332,0.49408353936993,0.481695833481332,0.49408353936993,0.481695833481332,
0.49408353936993,0.481695833481332,0.49408353936993,0.481695833481332,0.49408353936993,
0.481695833481332,0.49408353936993,0.481695833481332,0.49408353936993,0.481695833481332,
0.49408353936993,0.481695833481332,0.49408353936993,0.481695833481332,0.49408353936993,
0.481695833481332,0.49408353936993,0.481695833481332,0.49408353936993,0.481695833481332,
0.49408353936993,0.481695833481332,0.49408353936993,0.481695833481332,0.49408353936993,
0.481695833481332,0.49408353936993,0.481695833481332,0.49408353936993,0.481695833481332,
0.49408353936993,0.481695833481332,0.49408353936993,0.481695833481332,0.49408353936993,
0.481695833481332,0.49408353936993,0.481695833481332,0.49408353936993,0.481695833481332,
0.49408353936993,0.481695833481332,0.49408353936993,0.481695833481332,0.49408353936993,
0.481695833481332,0.49408353936993,0.481695833481332,0.49408353936993,0.481695833481332,
0.49408353936993,0.481695833481332,0.49408353936993,0.481695833481332,0.49408353936993,
0.481695833481332,0.49408353936993,0.481695833481332,0.49408353936993,0.481695833481332,
0.49408353936993,0.481695833481332,0.49408353936993,0.481695833481332,0.49408353936993),
(1.,0.974927912181824,1.,0.974927912181824,1.,0.974927912181824,1.,0.974927912181824,
1.,0.974927912181824,1.,0.974927912181824,1.,0.974927912181824,1.,0.974927912181824,
1.,0.974927912181824,1.,0.974927912181824,1.,0.974927912181824,1.,0.974927912181824,
1.,0.974927912181824,1.,0.974927912181824,1.,0.974927912181824,1.,0.974927912181824,
1.,0.974927912181824,1.,0.974927912181824,1.,0.974927912181824,1.,0.974927912181824,
1.,0.974927912181824,1.,0.974927912181824,1.,0.974927912181824,1.,0.974927912181824,
1.,0.974927912181824,1.,0.974927912181824,1.,0.974927912181824,1.,0.974927912181824,
1.,0.974927912181824,1.,0.974927912181824,1.,0.974927912181824,1.,0.974927912181824,
1.,0.974927912181824,1.,0.974927912181824,1.,0.974927912181824,1.,0.974927912181824,
1.,0.974927912181824,1.,0.974927912181824,1.,0.974927912181824,1.,0.974927912181824,
1.,0.974927912181824,1.,0.974927912181824,1.,0.974927912181824,1.,0.974927912181824,
1.,0.974927912181824,1.,0.974927912181824,1.,0.974927912181824,1.,0.974927912181824,
1.,0.974927912181824,1.,0.974927912181824,1.,0.974927912181824,1.,0.974927912181824,
1.,0.974927912181824,1.,0.974927912181824,1.,0.974927912181824,1.,0.974927912181824,
1.)))
REPRESENTATION_ITEM('')
SURFACE()
);
#324=(
BOUNDED_SURFACE()
B_SPLINE_SURFACE(1,2,((#15842,#15843,#15844,#15845,#15846,#15847,#15848,
#15849,#15850,#15851,#15852,#15853,#15854,#15855,#15856,#15857,#15858,#15859,
#15860,#15861,#15862,#15863,#15864,#15865,#15866,#15867,#15868,#15869,#15870,
#15871,#15872,#15873,#15874,#15875,#15876,#15877,#15878,#15879,#15880,#15881,
#15882,#15883,#15884,#15885,#15886,#15887,#15888,#15889,#15890,#15891,#15892,
#15893,#15894,#15895,#15896,#15897,#15898,#15899,#15900,#15901,#15902,#15903,
#15904,#15905,#15906,#15907,#15908,#15909,#15910,#15911,#15912,#15913,#15914,
#15915,#15916,#15917,#15918,#15919,#15920,#15921,#15922,#15923,#15924,#15925,
#15926,#15927,#15928,#15929,#15930,#15931,#15932,#15933,#15934,#15935,#15936,
#15937,#15938,#15939,#15940,#15941,#15942,#15943,#15944,#15945,#15946,#15947,
#15948,#15949,#15950,#15951,#15952,#15953,#15954),(#15955,#15956,#15957,
#15958,#15959,#15960,#15961,#15962,#15963,#15964,#15965,#15966,#15967,#15968,
#15969,#15970,#15971,#15972,#15973,#15974,#15975,#15976,#15977,#15978,#15979,
#15980,#15981,#15982,#15983,#15984,#15985,#15986,#15987,#15988,#15989,#15990,
#15991,#15992,#15993,#15994,#15995,#15996,#15997,#15998,#15999,#16000,#16001,
#16002,#16003,#16004,#16005,#16006,#16007,#16008,#16009,#16010,#16011,#16012,
#16013,#16014,#16015,#16016,#16017,#16018,#16019,#16020,#16021,#16022,#16023,
#16024,#16025,#16026,#16027,#16028,#16029,#16030,#16031,#16032,#16033,#16034,
#16035,#16036,#16037,#16038,#16039,#16040,#16041,#16042,#16043,#16044,#16045,
#16046,#16047,#16048,#16049,#16050,#16051,#16052,#16053,#16054,#16055,#16056,
#16057,#16058,#16059,#16060,#16061,#16062,#16063,#16064,#16065,#16066,#16067)),
 .UNSPECIFIED.,.F.,.F.,.F.)
B_SPLINE_SURFACE_WITH_KNOTS((2,2),(3,2,2,2,2,2,2,2,2,2,2,2,2,2,2,2,2,2,
2,2,2,2,2,2,2,2,2,2,2,2,2,2,2,2,2,2,2,2,2,2,2,2,2,2,2,2,2,2,2,2,2,2,2,2,
2,2,3),(0.,1.),(0.,0.0178571428571429,0.0357142857142857,0.0535714285714286,
0.0714285714285714,0.0892857142857143,0.107142857142857,0.125,0.142857142857143,
0.160714285714286,0.178571428571429,0.196428571428571,0.214285714285714,
0.232142857142857,0.25,0.267857142857143,0.285714285714286,0.303571428571429,
0.321428571428571,0.339285714285714,0.357142857142857,0.375,0.392857142857143,
0.410714285714286,0.428571428571429,0.446428571428571,0.464285714285714,
0.482142857142857,0.5,0.517857142857143,0.535714285714286,0.553571428571429,
0.571428571428571,0.589285714285714,0.607142857142857,0.625,0.642857142857143,
0.660714285714286,0.678571428571429,0.696428571428571,0.714285714285714,
0.732142857142857,0.75,0.767857142857143,0.785714285714286,0.803571428571429,
0.821428571428571,0.839285714285714,0.857142857142857,0.875,0.892857142857143,
0.910714285714286,0.928571428571429,0.946428571428571,0.964285714285714,
0.982142857142857,1.),.UNSPECIFIED.)
GEOMETRIC_REPRESENTATION_ITEM()
RATIONAL_B_SPLINE_SURFACE(((1.,0.974927912181824,1.,0.974927912181824,1.,
0.974927912181824,1.,0.974927912181824,1.,0.974927912181824,1.,0.974927912181824,
1.,0.974927912181824,1.,0.974927912181824,1.,0.974927912181824,1.,0.974927912181824,
1.,0.974927912181824,1.,0.974927912181824,1.,0.974927912181824,1.,0.974927912181824,
1.,0.974927912181824,1.,0.974927912181824,1.,0.974927912181824,1.,0.974927912181824,
1.,0.974927912181824,1.,0.974927912181824,1.,0.974927912181824,1.,0.974927912181824,
1.,0.974927912181824,1.,0.974927912181824,1.,0.974927912181824,1.,0.974927912181824,
1.,0.974927912181824,1.,0.974927912181824,1.,0.974927912181824,1.,0.974927912181824,
1.,0.974927912181824,1.,0.974927912181824,1.,0.974927912181824,1.,0.974927912181824,
1.,0.974927912181824,1.,0.974927912181824,1.,0.974927912181824,1.,0.974927912181824,
1.,0.974927912181824,1.,0.974927912181824,1.,0.974927912181824,1.,0.974927912181824,
1.,0.974927912181824,1.,0.974927912181824,1.,0.974927912181824,1.,0.974927912181824,
1.,0.974927912181824,1.,0.974927912181824,1.,0.974927912181824,1.,0.974927912181824,
1.,0.974927912181824,1.,0.974927912181824,1.,0.974927912181824,1.,0.974927912181824,
1.,0.974927912181824,1.,0.974927912181824,1.),(1.,0.974927912181824,1.,
0.974927912181824,1.,0.974927912181824,1.,0.974927912181824,1.,0.974927912181824,
1.,0.974927912181824,1.,0.974927912181824,1.,0.974927912181824,1.,0.974927912181824,
1.,0.974927912181824,1.,0.974927912181824,1.,0.974927912181824,1.,0.974927912181824,
1.,0.974927912181824,1.,0.974927912181824,1.,0.974927912181824,1.,0.974927912181824,
1.,0.974927912181824,1.,0.974927912181824,1.,0.974927912181824,1.,0.974927912181824,
1.,0.974927912181824,1.,0.974927912181824,1.,0.974927912181824,1.,0.974927912181824,
1.,0.974927912181824,1.,0.974927912181824,1.,0.974927912181824,1.,0.974927912181824,
1.,0.974927912181824,1.,0.974927912181824,1.,0.974927912181824,1.,0.974927912181824,
1.,0.974927912181824,1.,0.974927912181824,1.,0.974927912181824,1.,0.974927912181824,
1.,0.974927912181824,1.,0.974927912181824,1.,0.974927912181824,1.,0.974927912181824,
1.,0.974927912181824,1.,0.974927912181824,1.,0.974927912181824,1.,0.974927912181824,
1.,0.974927912181824,1.,0.974927912181824,1.,0.974927912181824,1.,0.974927912181824,
1.,0.974927912181824,1.,0.974927912181824,1.,0.974927912181824,1.,0.974927912181824,
1.,0.974927912181824,1.,0.974927912181824,1.,0.974927912181824,1.)))
REPRESENTATION_ITEM('')
SURFACE()
);
#325=(
BOUNDED_SURFACE()
B_SPLINE_SURFACE(1,2,((#16075,#16076,#16077,#16078,#16079,#16080,#16081,
#16082,#16083,#16084,#16085,#16086,#16087,#16088,#16089,#16090,#16091,#16092,
#16093,#16094,#16095,#16096,#16097,#16098,#16099,#16100,#16101,#16102,#16103,
#16104,#16105,#16106,#16107,#16108,#16109,#16110,#16111,#16112,#16113,#16114,
#16115,#16116,#16117,#16118,#16119,#16120,#16121,#16122,#16123,#16124,#16125,
#16126,#16127,#16128,#16129,#16130,#16131,#16132,#16133,#16134,#16135,#16136,
#16137,#16138,#16139,#16140,#16141,#16142,#16143,#16144,#16145,#16146,#16147,
#16148,#16149,#16150,#16151,#16152,#16153,#16154,#16155,#16156,#16157,#16158,
#16159,#16160,#16161,#16162,#16163,#16164,#16165,#16166,#16167,#16168,#16169,
#16170,#16171,#16172,#16173,#16174,#16175,#16176,#16177,#16178,#16179,#16180,
#16181,#16182,#16183,#16184,#16185,#16186,#16187),(#16188,#16189,#16190,
#16191,#16192,#16193,#16194,#16195,#16196,#16197,#16198,#16199,#16200,#16201,
#16202,#16203,#16204,#16205,#16206,#16207,#16208,#16209,#16210,#16211,#16212,
#16213,#16214,#16215,#16216,#16217,#16218,#16219,#16220,#16221,#16222,#16223,
#16224,#16225,#16226,#16227,#16228,#16229,#16230,#16231,#16232,#16233,#16234,
#16235,#16236,#16237,#16238,#16239,#16240,#16241,#16242,#16243,#16244,#16245,
#16246,#16247,#16248,#16249,#16250,#16251,#16252,#16253,#16254,#16255,#16256,
#16257,#16258,#16259,#16260,#16261,#16262,#16263,#16264,#16265,#16266,#16267,
#16268,#16269,#16270,#16271,#16272,#16273,#16274,#16275,#16276,#16277,#16278,
#16279,#16280,#16281,#16282,#16283,#16284,#16285,#16286,#16287,#16288,#16289,
#16290,#16291,#16292,#16293,#16294,#16295,#16296,#16297,#16298,#16299,#16300)),
 .UNSPECIFIED.,.F.,.F.,.F.)
B_SPLINE_SURFACE_WITH_KNOTS((2,2),(3,2,2,2,2,2,2,2,2,2,2,2,2,2,2,2,2,2,
2,2,2,2,2,2,2,2,2,2,2,2,2,2,2,2,2,2,2,2,2,2,2,2,2,2,2,2,2,2,2,2,2,2,2,2,
2,2,3),(0.,1.),(0.,0.0178571428571429,0.0357142857142857,0.0535714285714286,
0.0714285714285714,0.0892857142857143,0.107142857142857,0.125,0.142857142857143,
0.160714285714286,0.178571428571429,0.196428571428571,0.214285714285714,
0.232142857142857,0.25,0.267857142857143,0.285714285714286,0.303571428571429,
0.321428571428571,0.339285714285714,0.357142857142857,0.375,0.392857142857143,
0.410714285714286,0.428571428571429,0.446428571428571,0.464285714285714,
0.482142857142857,0.5,0.517857142857143,0.535714285714286,0.553571428571429,
0.571428571428571,0.589285714285714,0.607142857142857,0.625,0.642857142857143,
0.660714285714286,0.678571428571429,0.696428571428571,0.714285714285714,
0.732142857142857,0.75,0.767857142857143,0.785714285714286,0.803571428571429,
0.821428571428571,0.839285714285714,0.857142857142857,0.875,0.892857142857143,
0.910714285714286,0.928571428571429,0.946428571428571,0.964285714285714,
0.982142857142857,1.),.UNSPECIFIED.)
GEOMETRIC_REPRESENTATION_ITEM()
RATIONAL_B_SPLINE_SURFACE(((1.,0.974927912181824,1.,0.974927912181824,1.,
0.974927912181824,1.,0.974927912181824,1.,0.974927912181824,1.,0.974927912181824,
1.,0.974927912181824,1.,0.974927912181824,1.,0.974927912181824,1.,0.974927912181824,
1.,0.974927912181824,1.,0.974927912181824,1.,0.974927912181824,1.,0.974927912181824,
1.,0.974927912181824,1.,0.974927912181824,1.,0.974927912181824,1.,0.974927912181824,
1.,0.974927912181824,1.,0.974927912181824,1.,0.974927912181824,1.,0.974927912181824,
1.,0.974927912181824,1.,0.974927912181824,1.,0.974927912181824,1.,0.974927912181824,
1.,0.974927912181824,1.,0.974927912181824,1.,0.974927912181824,1.,0.974927912181824,
1.,0.974927912181824,1.,0.974927912181824,1.,0.974927912181824,1.,0.974927912181824,
1.,0.974927912181824,1.,0.974927912181824,1.,0.974927912181824,1.,0.974927912181824,
1.,0.974927912181824,1.,0.974927912181824,1.,0.974927912181824,1.,0.974927912181824,
1.,0.974927912181824,1.,0.974927912181824,1.,0.974927912181824,1.,0.974927912181824,
1.,0.974927912181824,1.,0.974927912181824,1.,0.974927912181824,1.,0.974927912181824,
1.,0.974927912181824,1.,0.974927912181824,1.,0.974927912181824,1.,0.974927912181824,
1.,0.974927912181824,1.,0.974927912181824,1.),(1.,0.974927912181824,1.,
0.974927912181824,1.,0.974927912181824,1.,0.974927912181824,1.,0.974927912181824,
1.,0.974927912181824,1.,0.974927912181824,1.,0.974927912181824,1.,0.974927912181824,
1.,0.974927912181824,1.,0.974927912181824,1.,0.974927912181824,1.,0.974927912181824,
1.,0.974927912181824,1.,0.974927912181824,1.,0.974927912181824,1.,0.974927912181824,
1.,0.974927912181824,1.,0.974927912181824,1.,0.974927912181824,1.,0.974927912181824,
1.,0.974927912181824,1.,0.974927912181824,1.,0.974927912181824,1.,0.974927912181824,
1.,0.974927912181824,1.,0.974927912181824,1.,0.974927912181824,1.,0.974927912181824,
1.,0.974927912181824,1.,0.974927912181824,1.,0.974927912181824,1.,0.974927912181824,
1.,0.974927912181824,1.,0.974927912181824,1.,0.974927912181824,1.,0.974927912181824,
1.,0.974927912181824,1.,0.974927912181824,1.,0.974927912181824,1.,0.974927912181824,
1.,0.974927912181824,1.,0.974927912181824,1.,0.974927912181824,1.,0.974927912181824,
1.,0.974927912181824,1.,0.974927912181824,1.,0.974927912181824,1.,0.974927912181824,
1.,0.974927912181824,1.,0.974927912181824,1.,0.974927912181824,1.,0.974927912181824,
1.,0.974927912181824,1.,0.974927912181824,1.,0.974927912181824,1.)))
REPRESENTATION_ITEM('')
SURFACE()
);
#326=(
BOUNDED_SURFACE()
B_SPLINE_SURFACE(3,2,((#16414,#16415,#16416,#16417,#16418,#16419,#16420,
#16421,#16422,#16423,#16424,#16425,#16426,#16427,#16428,#16429,#16430,#16431,
#16432,#16433,#16434,#16435,#16436,#16437,#16438,#16439,#16440,#16441,#16442,
#16443,#16444,#16445,#16446,#16447,#16448,#16449,#16450,#16451,#16452,#16453,
#16454,#16455,#16456,#16457,#16458,#16459,#16460,#16461,#16462,#16463,#16464,
#16465,#16466,#16467,#16468,#16469,#16470,#16471,#16472,#16473,#16474,#16475,
#16476,#16477,#16478,#16479,#16480,#16481,#16482,#16483,#16484,#16485,#16486,
#16487,#16488,#16489,#16490,#16491,#16492,#16493,#16494,#16495,#16496,#16497,
#16498,#16499,#16500,#16501,#16502,#16503,#16504,#16505,#16506,#16507,#16508,
#16509,#16510,#16511,#16512,#16513,#16514,#16515,#16516,#16517,#16518,#16519,
#16520,#16521,#16522,#16523,#16524,#16525,#16526),(#16527,#16528,#16529,
#16530,#16531,#16532,#16533,#16534,#16535,#16536,#16537,#16538,#16539,#16540,
#16541,#16542,#16543,#16544,#16545,#16546,#16547,#16548,#16549,#16550,#16551,
#16552,#16553,#16554,#16555,#16556,#16557,#16558,#16559,#16560,#16561,#16562,
#16563,#16564,#16565,#16566,#16567,#16568,#16569,#16570,#16571,#16572,#16573,
#16574,#16575,#16576,#16577,#16578,#16579,#16580,#16581,#16582,#16583,#16584,
#16585,#16586,#16587,#16588,#16589,#16590,#16591,#16592,#16593,#16594,#16595,
#16596,#16597,#16598,#16599,#16600,#16601,#16602,#16603,#16604,#16605,#16606,
#16607,#16608,#16609,#16610,#16611,#16612,#16613,#16614,#16615,#16616,#16617,
#16618,#16619,#16620,#16621,#16622,#16623,#16624,#16625,#16626,#16627,#16628,
#16629,#16630,#16631,#16632,#16633,#16634,#16635,#16636,#16637,#16638,#16639),
(#16640,#16641,#16642,#16643,#16644,#16645,#16646,#16647,#16648,#16649,
#16650,#16651,#16652,#16653,#16654,#16655,#16656,#16657,#16658,#16659,#16660,
#16661,#16662,#16663,#16664,#16665,#16666,#16667,#16668,#16669,#16670,#16671,
#16672,#16673,#16674,#16675,#16676,#16677,#16678,#16679,#16680,#16681,#16682,
#16683,#16684,#16685,#16686,#16687,#16688,#16689,#16690,#16691,#16692,#16693,
#16694,#16695,#16696,#16697,#16698,#16699,#16700,#16701,#16702,#16703,#16704,
#16705,#16706,#16707,#16708,#16709,#16710,#16711,#16712,#16713,#16714,#16715,
#16716,#16717,#16718,#16719,#16720,#16721,#16722,#16723,#16724,#16725,#16726,
#16727,#16728,#16729,#16730,#16731,#16732,#16733,#16734,#16735,#16736,#16737,
#16738,#16739,#16740,#16741,#16742,#16743,#16744,#16745,#16746,#16747,#16748,
#16749,#16750,#16751,#16752),(#16753,#16754,#16755,#16756,#16757,#16758,
#16759,#16760,#16761,#16762,#16763,#16764,#16765,#16766,#16767,#16768,#16769,
#16770,#16771,#16772,#16773,#16774,#16775,#16776,#16777,#16778,#16779,#16780,
#16781,#16782,#16783,#16784,#16785,#16786,#16787,#16788,#16789,#16790,#16791,
#16792,#16793,#16794,#16795,#16796,#16797,#16798,#16799,#16800,#16801,#16802,
#16803,#16804,#16805,#16806,#16807,#16808,#16809,#16810,#16811,#16812,#16813,
#16814,#16815,#16816,#16817,#16818,#16819,#16820,#16821,#16822,#16823,#16824,
#16825,#16826,#16827,#16828,#16829,#16830,#16831,#16832,#16833,#16834,#16835,
#16836,#16837,#16838,#16839,#16840,#16841,#16842,#16843,#16844,#16845,#16846,
#16847,#16848,#16849,#16850,#16851,#16852,#16853,#16854,#16855,#16856,#16857,
#16858,#16859,#16860,#16861,#16862,#16863,#16864,#16865)),.UNSPECIFIED.,
 .F.,.F.,.F.)
B_SPLINE_SURFACE_WITH_KNOTS((4,4),(3,2,2,2,2,2,2,2,2,2,2,2,2,2,2,2,2,2,
2,2,2,2,2,2,2,2,2,2,2,2,2,2,2,2,2,2,2,2,2,2,2,2,2,2,2,2,2,2,2,2,2,2,2,2,
2,2,3),(0.,1.),(0.,0.0178571428571429,0.0357142857142857,0.0535714285714286,
0.0714285714285714,0.0892857142857143,0.107142857142857,0.125,0.142857142857143,
0.160714285714286,0.178571428571429,0.196428571428571,0.214285714285714,
0.232142857142857,0.25,0.267857142857143,0.285714285714286,0.303571428571429,
0.321428571428571,0.339285714285714,0.357142857142857,0.375,0.392857142857143,
0.410714285714286,0.428571428571429,0.446428571428571,0.464285714285714,
0.482142857142857,0.5,0.517857142857143,0.535714285714286,0.553571428571429,
0.571428571428571,0.589285714285714,0.607142857142857,0.625,0.642857142857143,
0.660714285714286,0.678571428571429,0.696428571428571,0.714285714285714,
0.732142857142857,0.75,0.767857142857143,0.785714285714286,0.803571428571429,
0.821428571428571,0.839285714285714,0.857142857142857,0.875,0.892857142857143,
0.910714285714286,0.928571428571429,0.946428571428571,0.964285714285714,
0.982142857142857,1.),.UNSPECIFIED.)
GEOMETRIC_REPRESENTATION_ITEM()
RATIONAL_B_SPLINE_SURFACE(((1.,0.974927912181824,1.,0.974927912181824,1.,
0.974927912181824,1.,0.974927912181824,1.,0.974927912181824,1.,0.974927912181824,
1.,0.974927912181824,1.,0.974927912181824,1.,0.974927912181824,1.,0.974927912181824,
1.,0.974927912181824,1.,0.974927912181824,1.,0.974927912181824,1.,0.974927912181824,
1.,0.974927912181824,1.,0.974927912181824,1.,0.974927912181824,1.,0.974927912181824,
1.,0.974927912181824,1.,0.974927912181824,1.,0.974927912181824,1.,0.974927912181824,
1.,0.974927912181824,1.,0.974927912181824,1.,0.974927912181824,1.,0.974927912181824,
1.,0.974927912181824,1.,0.974927912181824,1.,0.974927912181824,1.,0.974927912181824,
1.,0.974927912181824,1.,0.974927912181824,1.,0.974927912181824,1.,0.974927912181824,
1.,0.974927912181824,1.,0.974927912181824,1.,0.974927912181824,1.,0.974927912181824,
1.,0.974927912181824,1.,0.974927912181824,1.,0.974927912181824,1.,0.974927912181824,
1.,0.974927912181824,1.,0.974927912181824,1.,0.974927912181824,1.,0.974927912181824,
1.,0.974927912181824,1.,0.974927912181824,1.,0.974927912181824,1.,0.974927912181824,
1.,0.974927912181824,1.,0.974927912181824,1.,0.974927912181824,1.,0.974927912181824,
1.,0.974927912181824,1.,0.974927912181824,1.),(0.49408353936993,0.481695833481332,
0.49408353936993,0.481695833481332,0.49408353936993,0.481695833481332,0.49408353936993,
0.481695833481332,0.49408353936993,0.481695833481332,0.49408353936993,0.481695833481332,
0.49408353936993,0.481695833481332,0.49408353936993,0.481695833481332,0.49408353936993,
0.481695833481332,0.49408353936993,0.481695833481332,0.49408353936993,0.481695833481332,
0.49408353936993,0.481695833481332,0.49408353936993,0.481695833481332,0.49408353936993,
0.481695833481332,0.49408353936993,0.481695833481332,0.49408353936993,0.481695833481332,
0.49408353936993,0.481695833481332,0.49408353936993,0.481695833481332,0.49408353936993,
0.481695833481332,0.49408353936993,0.481695833481332,0.49408353936993,0.481695833481332,
0.49408353936993,0.481695833481332,0.49408353936993,0.481695833481332,0.49408353936993,
0.481695833481332,0.49408353936993,0.481695833481332,0.49408353936993,0.481695833481332,
0.49408353936993,0.481695833481332,0.49408353936993,0.481695833481332,0.49408353936993,
0.481695833481332,0.49408353936993,0.481695833481332,0.49408353936993,0.481695833481332,
0.49408353936993,0.481695833481332,0.49408353936993,0.481695833481332,0.49408353936993,
0.481695833481332,0.49408353936993,0.481695833481332,0.49408353936993,0.481695833481332,
0.49408353936993,0.481695833481332,0.49408353936993,0.481695833481332,0.49408353936993,
0.481695833481332,0.49408353936993,0.481695833481332,0.49408353936993,0.481695833481332,
0.49408353936993,0.481695833481332,0.49408353936993,0.481695833481332,0.49408353936993,
0.481695833481332,0.49408353936993,0.481695833481332,0.49408353936993,0.481695833481332,
0.49408353936993,0.481695833481332,0.49408353936993,0.481695833481332,0.49408353936993,
0.481695833481332,0.49408353936993,0.481695833481332,0.49408353936993,0.481695833481332,
0.49408353936993,0.481695833481332,0.49408353936993,0.481695833481332,0.49408353936993,
0.481695833481332,0.49408353936993,0.481695833481332,0.49408353936993,0.481695833481332,
0.49408353936993),(0.49408353936993,0.481695833481332,0.49408353936993,
0.481695833481332,0.49408353936993,0.481695833481332,0.49408353936993,0.481695833481332,
0.49408353936993,0.481695833481332,0.49408353936993,0.481695833481332,0.49408353936993,
0.481695833481332,0.49408353936993,0.481695833481332,0.49408353936993,0.481695833481332,
0.49408353936993,0.481695833481332,0.49408353936993,0.481695833481332,0.49408353936993,
0.481695833481332,0.49408353936993,0.481695833481332,0.49408353936993,0.481695833481332,
0.49408353936993,0.481695833481332,0.49408353936993,0.481695833481332,0.49408353936993,
0.481695833481332,0.49408353936993,0.481695833481332,0.49408353936993,0.481695833481332,
0.49408353936993,0.481695833481332,0.49408353936993,0.481695833481332,0.49408353936993,
0.481695833481332,0.49408353936993,0.481695833481332,0.49408353936993,0.481695833481332,
0.49408353936993,0.481695833481332,0.49408353936993,0.481695833481332,0.49408353936993,
0.481695833481332,0.49408353936993,0.481695833481332,0.49408353936993,0.481695833481332,
0.49408353936993,0.481695833481332,0.49408353936993,0.481695833481332,0.49408353936993,
0.481695833481332,0.49408353936993,0.481695833481332,0.49408353936993,0.481695833481332,
0.49408353936993,0.481695833481332,0.49408353936993,0.481695833481332,0.49408353936993,
0.481695833481332,0.49408353936993,0.481695833481332,0.49408353936993,0.481695833481332,
0.49408353936993,0.481695833481332,0.49408353936993,0.481695833481332,0.49408353936993,
0.481695833481332,0.49408353936993,0.481695833481332,0.49408353936993,0.481695833481332,
0.49408353936993,0.481695833481332,0.49408353936993,0.481695833481332,0.49408353936993,
0.481695833481332,0.49408353936993,0.481695833481332,0.49408353936993,0.481695833481332,
0.49408353936993,0.481695833481332,0.49408353936993,0.481695833481332,0.49408353936993,
0.481695833481332,0.49408353936993,0.481695833481332,0.49408353936993,0.481695833481332,
0.49408353936993,0.481695833481332,0.49408353936993,0.481695833481332,0.49408353936993),
(1.,0.974927912181824,1.,0.974927912181824,1.,0.974927912181824,1.,0.974927912181824,
1.,0.974927912181824,1.,0.974927912181824,1.,0.974927912181824,1.,0.974927912181824,
1.,0.974927912181824,1.,0.974927912181824,1.,0.974927912181824,1.,0.974927912181824,
1.,0.974927912181824,1.,0.974927912181824,1.,0.974927912181824,1.,0.974927912181824,
1.,0.974927912181824,1.,0.974927912181824,1.,0.974927912181824,1.,0.974927912181824,
1.,0.974927912181824,1.,0.974927912181824,1.,0.974927912181824,1.,0.974927912181824,
1.,0.974927912181824,1.,0.974927912181824,1.,0.974927912181824,1.,0.974927912181824,
1.,0.974927912181824,1.,0.974927912181824,1.,0.974927912181824,1.,0.974927912181824,
1.,0.974927912181824,1.,0.974927912181824,1.,0.974927912181824,1.,0.974927912181824,
1.,0.974927912181824,1.,0.974927912181824,1.,0.974927912181824,1.,0.974927912181824,
1.,0.974927912181824,1.,0.974927912181824,1.,0.974927912181824,1.,0.974927912181824,
1.,0.974927912181824,1.,0.974927912181824,1.,0.974927912181824,1.,0.974927912181824,
1.,0.974927912181824,1.,0.974927912181824,1.,0.974927912181824,1.,0.974927912181824,
1.,0.974927912181824,1.,0.974927912181824,1.,0.974927912181824,1.,0.974927912181824,
1.)))
REPRESENTATION_ITEM('')
SURFACE()
);
#327=(
BOUNDED_SURFACE()
B_SPLINE_SURFACE(1,2,((#16979,#16980,#16981,#16982,#16983,#16984,#16985,
#16986,#16987,#16988,#16989,#16990,#16991,#16992,#16993,#16994,#16995,#16996,
#16997,#16998,#16999,#17000,#17001,#17002,#17003,#17004,#17005,#17006,#17007,
#17008,#17009,#17010,#17011,#17012,#17013,#17014,#17015,#17016,#17017,#17018,
#17019,#17020,#17021,#17022,#17023,#17024,#17025,#17026,#17027,#17028,#17029,
#17030,#17031,#17032,#17033,#17034,#17035,#17036,#17037,#17038,#17039,#17040,
#17041,#17042,#17043,#17044,#17045,#17046,#17047,#17048,#17049,#17050,#17051,
#17052,#17053,#17054,#17055,#17056,#17057,#17058,#17059,#17060,#17061,#17062,
#17063,#17064,#17065,#17066,#17067,#17068,#17069,#17070,#17071,#17072,#17073,
#17074,#17075,#17076,#17077,#17078,#17079,#17080,#17081,#17082,#17083,#17084,
#17085,#17086,#17087,#17088,#17089,#17090,#17091),(#17092,#17093,#17094,
#17095,#17096,#17097,#17098,#17099,#17100,#17101,#17102,#17103,#17104,#17105,
#17106,#17107,#17108,#17109,#17110,#17111,#17112,#17113,#17114,#17115,#17116,
#17117,#17118,#17119,#17120,#17121,#17122,#17123,#17124,#17125,#17126,#17127,
#17128,#17129,#17130,#17131,#17132,#17133,#17134,#17135,#17136,#17137,#17138,
#17139,#17140,#17141,#17142,#17143,#17144,#17145,#17146,#17147,#17148,#17149,
#17150,#17151,#17152,#17153,#17154,#17155,#17156,#17157,#17158,#17159,#17160,
#17161,#17162,#17163,#17164,#17165,#17166,#17167,#17168,#17169,#17170,#17171,
#17172,#17173,#17174,#17175,#17176,#17177,#17178,#17179,#17180,#17181,#17182,
#17183,#17184,#17185,#17186,#17187,#17188,#17189,#17190,#17191,#17192,#17193,
#17194,#17195,#17196,#17197,#17198,#17199,#17200,#17201,#17202,#17203,#17204)),
 .UNSPECIFIED.,.F.,.F.,.F.)
B_SPLINE_SURFACE_WITH_KNOTS((2,2),(3,2,2,2,2,2,2,2,2,2,2,2,2,2,2,2,2,2,
2,2,2,2,2,2,2,2,2,2,2,2,2,2,2,2,2,2,2,2,2,2,2,2,2,2,2,2,2,2,2,2,2,2,2,2,
2,2,3),(0.,1.),(0.,0.0178571428571429,0.0357142857142857,0.0535714285714286,
0.0714285714285714,0.0892857142857143,0.107142857142857,0.125,0.142857142857143,
0.160714285714286,0.178571428571429,0.196428571428571,0.214285714285714,
0.232142857142857,0.25,0.267857142857143,0.285714285714286,0.303571428571429,
0.321428571428571,0.339285714285714,0.357142857142857,0.375,0.392857142857143,
0.410714285714286,0.428571428571429,0.446428571428571,0.464285714285714,
0.482142857142857,0.5,0.517857142857143,0.535714285714286,0.553571428571429,
0.571428571428571,0.589285714285714,0.607142857142857,0.625,0.642857142857143,
0.660714285714286,0.678571428571429,0.696428571428571,0.714285714285714,
0.732142857142857,0.75,0.767857142857143,0.785714285714286,0.803571428571429,
0.821428571428571,0.839285714285714,0.857142857142857,0.875,0.892857142857143,
0.910714285714286,0.928571428571429,0.946428571428571,0.964285714285714,
0.982142857142857,1.),.UNSPECIFIED.)
GEOMETRIC_REPRESENTATION_ITEM()
RATIONAL_B_SPLINE_SURFACE(((1.,0.974927912181824,1.,0.974927912181824,1.,
0.974927912181824,1.,0.974927912181824,1.,0.974927912181824,1.,0.974927912181824,
1.,0.974927912181824,1.,0.974927912181824,1.,0.974927912181824,1.,0.974927912181824,
1.,0.974927912181824,1.,0.974927912181824,1.,0.974927912181824,1.,0.974927912181824,
1.,0.974927912181824,1.,0.974927912181824,1.,0.974927912181824,1.,0.974927912181824,
1.,0.974927912181824,1.,0.974927912181824,1.,0.974927912181824,1.,0.974927912181824,
1.,0.974927912181824,1.,0.974927912181824,1.,0.974927912181824,1.,0.974927912181824,
1.,0.974927912181824,1.,0.974927912181824,1.,0.974927912181824,1.,0.974927912181824,
1.,0.974927912181824,1.,0.974927912181824,1.,0.974927912181824,1.,0.974927912181824,
1.,0.974927912181824,1.,0.974927912181824,1.,0.974927912181824,1.,0.974927912181824,
1.,0.974927912181824,1.,0.974927912181824,1.,0.974927912181824,1.,0.974927912181824,
1.,0.974927912181824,1.,0.974927912181824,1.,0.974927912181824,1.,0.974927912181824,
1.,0.974927912181824,1.,0.974927912181824,1.,0.974927912181824,1.,0.974927912181824,
1.,0.974927912181824,1.,0.974927912181824,1.,0.974927912181824,1.,0.974927912181824,
1.,0.974927912181824,1.,0.974927912181824,1.),(1.,0.974927912181824,1.,
0.974927912181824,1.,0.974927912181824,1.,0.974927912181824,1.,0.974927912181824,
1.,0.974927912181824,1.,0.974927912181824,1.,0.974927912181824,1.,0.974927912181824,
1.,0.974927912181824,1.,0.974927912181824,1.,0.974927912181824,1.,0.974927912181824,
1.,0.974927912181824,1.,0.974927912181824,1.,0.974927912181824,1.,0.974927912181824,
1.,0.974927912181824,1.,0.974927912181824,1.,0.974927912181824,1.,0.974927912181824,
1.,0.974927912181824,1.,0.974927912181824,1.,0.974927912181824,1.,0.974927912181824,
1.,0.974927912181824,1.,0.974927912181824,1.,0.974927912181824,1.,0.974927912181824,
1.,0.974927912181824,1.,0.974927912181824,1.,0.974927912181824,1.,0.974927912181824,
1.,0.974927912181824,1.,0.974927912181824,1.,0.974927912181824,1.,0.974927912181824,
1.,0.974927912181824,1.,0.974927912181824,1.,0.974927912181824,1.,0.974927912181824,
1.,0.974927912181824,1.,0.974927912181824,1.,0.974927912181824,1.,0.974927912181824,
1.,0.974927912181824,1.,0.974927912181824,1.,0.974927912181824,1.,0.974927912181824,
1.,0.974927912181824,1.,0.974927912181824,1.,0.974927912181824,1.,0.974927912181824,
1.,0.974927912181824,1.,0.974927912181824,1.,0.974927912181824,1.)))
REPRESENTATION_ITEM('')
SURFACE()
);
#328=(
BOUNDED_SURFACE()
B_SPLINE_SURFACE(3,2,((#22854,#22855,#22856,#22857,#22858,#22859,#22860,
#22861,#22862),(#22863,#22864,#22865,#22866,#22867,#22868,#22869,#22870,
#22871),(#22872,#22873,#22874,#22875,#22876,#22877,#22878,#22879,#22880),
(#22881,#22882,#22883,#22884,#22885,#22886,#22887,#22888,#22889)),
 .UNSPECIFIED.,.F.,.F.,.F.)
B_SPLINE_SURFACE_WITH_KNOTS((4,4),(3,2,2,2,3),(0.,1.),(0.,0.25,0.5,0.75,
1.),.UNSPECIFIED.)
GEOMETRIC_REPRESENTATION_ITEM()
RATIONAL_B_SPLINE_SURFACE(((1.,0.974927912181824,1.,0.974927912181824,1.,
0.974927912181824,1.,0.974927912181824,1.),(0.833333333333332,0.812439926818185,
0.833333333333332,0.812439926818185,0.833333333333332,0.812439926818185,
0.833333333333332,0.812439926818185,0.833333333333332),(0.833333333333332,
0.812439926818185,0.833333333333332,0.812439926818185,0.833333333333332,
0.812439926818185,0.833333333333332,0.812439926818185,0.833333333333332),
(1.,0.974927912181824,1.,0.974927912181824,1.,0.974927912181824,1.,0.974927912181824,
1.)))
REPRESENTATION_ITEM('')
SURFACE()
);
#329=(
BOUNDED_SURFACE()
B_SPLINE_SURFACE(3,2,((#22952,#22953,#22954,#22955,#22956,#22957,#22958,
#22959,#22960),(#22961,#22962,#22963,#22964,#22965,#22966,#22967,#22968,
#22969),(#22970,#22971,#22972,#22973,#22974,#22975,#22976,#22977,#22978),
(#22979,#22980,#22981,#22982,#22983,#22984,#22985,#22986,#22987)),
 .UNSPECIFIED.,.F.,.F.,.F.)
B_SPLINE_SURFACE_WITH_KNOTS((4,4),(3,2,2,2,3),(0.,1.),(0.,0.25,0.5,0.75,
1.),.UNSPECIFIED.)
GEOMETRIC_REPRESENTATION_ITEM()
RATIONAL_B_SPLINE_SURFACE(((1.,0.974927912181824,1.,0.974927912181824,1.,
0.974927912181824,1.,0.974927912181824,1.),(0.987189825241073,0.962438915249418,
0.987189825241073,0.962438915249418,0.987189825241073,0.962438915249418,
0.987189825241073,0.962438915249418,0.987189825241073),(0.987189825241073,
0.962438915249418,0.987189825241073,0.962438915249418,0.987189825241073,
0.962438915249418,0.987189825241073,0.962438915249418,0.987189825241073),
(1.,0.974927912181824,1.,0.974927912181824,1.,0.974927912181824,1.,0.974927912181824,
1.)))
REPRESENTATION_ITEM('')
SURFACE()
);
#330=(
BOUNDED_SURFACE()
B_SPLINE_SURFACE(3,2,((#22989,#22990,#22991,#22992,#22993,#22994,#22995,
#22996,#22997),(#22998,#22999,#23000,#23001,#23002,#23003,#23004,#23005,
#23006),(#23007,#23008,#23009,#23010,#23011,#23012,#23013,#23014,#23015),
(#23016,#23017,#23018,#23019,#23020,#23021,#23022,#23023,#23024)),
 .UNSPECIFIED.,.F.,.F.,.F.)
B_SPLINE_SURFACE_WITH_KNOTS((4,4),(3,2,2,2,3),(0.,1.),(0.,0.25,0.5,0.75,
1.),.UNSPECIFIED.)
GEOMETRIC_REPRESENTATION_ITEM()
RATIONAL_B_SPLINE_SURFACE(((1.,0.974927912181824,1.,0.974927912181824,1.,
0.974927912181824,1.,0.974927912181824,1.),(0.987189825241073,0.962438915249418,
0.987189825241073,0.962438915249418,0.987189825241073,0.962438915249418,
0.987189825241073,0.962438915249418,0.987189825241073),(0.987189825241073,
0.962438915249418,0.987189825241073,0.962438915249418,0.987189825241073,
0.962438915249418,0.987189825241073,0.962438915249418,0.987189825241073),
(1.,0.974927912181824,1.,0.974927912181824,1.,0.974927912181824,1.,0.974927912181824,
1.)))
REPRESENTATION_ITEM('')
SURFACE()
);
#331=(
BOUNDED_SURFACE()
B_SPLINE_SURFACE(3,3,((#23026,#23027,#23028,#23029,#23030,#23031,#23032,
#23033,#23034,#23035,#23036,#23037),(#23038,#23039,#23040,#23041,#23042,
#23043,#23044,#23045,#23046,#23047,#23048,#23049),(#23050,#23051,#23052,
#23053,#23054,#23055,#23056,#23057,#23058,#23059,#23060,#23061),(#23062,
#23063,#23064,#23065,#23066,#23067,#23068,#23069,#23070,#23071,#23072,#23073)),
 .UNSPECIFIED.,.F.,.F.,.F.)
B_SPLINE_SURFACE_WITH_KNOTS((4,4),(4,2,2,2,2,4),(0.,1.),(0.,0.0783698293107414,
0.308777371982556,0.539184914655036,0.769592457327518,1.),.UNSPECIFIED.)
GEOMETRIC_REPRESENTATION_ITEM()
RATIONAL_B_SPLINE_SURFACE(((1.,1.,1.,1.,1.,1.,1.,1.,1.,1.,1.,1.),(0.833333333333332,
0.833333333333332,0.833333333333332,0.833333333333332,0.833333333333332,
0.833333333333332,0.833333333333332,0.833333333333332,0.833333333333332,
0.833333333333332,0.833333333333332,0.833333333333332),(0.833333333333332,
0.833333333333332,0.833333333333332,0.833333333333332,0.833333333333332,
0.833333333333332,0.833333333333332,0.833333333333332,0.833333333333332,
0.833333333333332,0.833333333333332,0.833333333333332),(1.,1.,1.,1.,1.,
1.,1.,1.,1.,1.,1.,1.)))
REPRESENTATION_ITEM('')
SURFACE()
);
#332=(
BOUNDED_SURFACE()
B_SPLINE_SURFACE(3,3,((#23090,#23091,#23092,#23093,#23094,#23095,#23096,
#23097,#23098,#23099,#23100,#23101),(#23102,#23103,#23104,#23105,#23106,
#23107,#23108,#23109,#23110,#23111,#23112,#23113),(#23114,#23115,#23116,
#23117,#23118,#23119,#23120,#23121,#23122,#23123,#23124,#23125),(#23126,
#23127,#23128,#23129,#23130,#23131,#23132,#23133,#23134,#23135,#23136,#23137)),
 .UNSPECIFIED.,.F.,.F.,.F.)
B_SPLINE_SURFACE_WITH_KNOTS((4,4),(4,2,2,2,2,4),(0.,1.),(0.,0.0783698293107414,
0.308777371982556,0.539184914655036,0.769592457327518,1.),.UNSPECIFIED.)
GEOMETRIC_REPRESENTATION_ITEM()
RATIONAL_B_SPLINE_SURFACE(((1.,1.,1.,1.,1.,1.,1.,1.,1.,1.,1.,1.),(0.987189825241073,
0.987189825241073,0.987189825241073,0.987189825241073,0.987189825241073,
0.987189825241073,0.987189825241073,0.987189825241073,0.987189825241073,
0.987189825241073,0.987189825241073,0.987189825241073),(0.987189825241073,
0.987189825241073,0.987189825241073,0.987189825241073,0.987189825241073,
0.987189825241073,0.987189825241073,0.987189825241073,0.987189825241073,
0.987189825241073,0.987189825241073,0.987189825241073),(1.,1.,1.,1.,1.,
1.,1.,1.,1.,1.,1.,1.)))
REPRESENTATION_ITEM('')
SURFACE()
);
#333=(
BOUNDED_SURFACE()
B_SPLINE_SURFACE(3,3,((#23138,#23139,#23140,#23141,#23142,#23143,#23144,
#23145,#23146,#23147,#23148,#23149),(#23150,#23151,#23152,#23153,#23154,
#23155,#23156,#23157,#23158,#23159,#23160,#23161),(#23162,#23163,#23164,
#23165,#23166,#23167,#23168,#23169,#23170,#23171,#23172,#23173),(#23174,
#23175,#23176,#23177,#23178,#23179,#23180,#23181,#23182,#23183,#23184,#23185)),
 .UNSPECIFIED.,.F.,.F.,.F.)
B_SPLINE_SURFACE_WITH_KNOTS((4,4),(4,2,2,2,2,4),(0.,1.),(0.,0.0783698293107414,
0.308777371982556,0.539184914655036,0.769592457327518,1.),.UNSPECIFIED.)
GEOMETRIC_REPRESENTATION_ITEM()
RATIONAL_B_SPLINE_SURFACE(((1.,1.,1.,1.,1.,1.,1.,1.,1.,1.,1.,1.),(0.987189825241073,
0.987189825241073,0.987189825241073,0.987189825241073,0.987189825241073,
0.987189825241073,0.987189825241073,0.987189825241073,0.987189825241073,
0.987189825241073,0.987189825241073,0.987189825241073),(0.987189825241073,
0.987189825241073,0.987189825241073,0.987189825241073,0.987189825241073,
0.987189825241073,0.987189825241073,0.987189825241073,0.987189825241073,
0.987189825241073,0.987189825241073,0.987189825241073),(1.,1.,1.,1.,1.,
1.,1.,1.,1.,1.,1.,1.)))
REPRESENTATION_ITEM('')
SURFACE()
);
#334=(
BOUNDED_SURFACE()
B_SPLINE_SURFACE(3,2,((#23186,#23187,#23188,#23189,#23190,#23191,#23192,
#23193,#23194),(#23195,#23196,#23197,#23198,#23199,#23200,#23201,#23202,
#23203),(#23204,#23205,#23206,#23207,#23208,#23209,#23210,#23211,#23212),
(#23213,#23214,#23215,#23216,#23217,#23218,#23219,#23220,#23221)),
 .UNSPECIFIED.,.F.,.F.,.F.)
B_SPLINE_SURFACE_WITH_KNOTS((4,4),(3,2,2,2,3),(0.,1.),(0.,0.25,0.5,0.75,
1.),.UNSPECIFIED.)
GEOMETRIC_REPRESENTATION_ITEM()
RATIONAL_B_SPLINE_SURFACE(((1.,0.974927912181824,1.,0.974927912181824,1.,
0.974927912181824,1.,0.974927912181824,1.),(0.987189825241073,0.962438915249418,
0.987189825241073,0.962438915249418,0.987189825241073,0.962438915249418,
0.987189825241073,0.962438915249418,0.987189825241073),(0.987189825241073,
0.962438915249418,0.987189825241073,0.962438915249418,0.987189825241073,
0.962438915249418,0.987189825241073,0.962438915249418,0.987189825241073),
(1.,0.974927912181824,1.,0.974927912181824,1.,0.974927912181824,1.,0.974927912181824,
1.)))
REPRESENTATION_ITEM('')
SURFACE()
);
#335=(
BOUNDED_SURFACE()
B_SPLINE_SURFACE(3,2,((#23276,#23277,#23278,#23279,#23280,#23281,#23282,
#23283,#23284),(#23285,#23286,#23287,#23288,#23289,#23290,#23291,#23292,
#23293),(#23294,#23295,#23296,#23297,#23298,#23299,#23300,#23301,#23302),
(#23303,#23304,#23305,#23306,#23307,#23308,#23309,#23310,#23311)),
 .UNSPECIFIED.,.F.,.F.,.F.)
B_SPLINE_SURFACE_WITH_KNOTS((4,4),(3,2,2,2,3),(0.,1.),(0.,0.25,0.5,0.75,
1.),.UNSPECIFIED.)
GEOMETRIC_REPRESENTATION_ITEM()
RATIONAL_B_SPLINE_SURFACE(((1.,0.974927912181824,1.,0.974927912181824,1.,
0.974927912181824,1.,0.974927912181824,1.),(0.987189825241073,0.962438915249418,
0.987189825241073,0.962438915249418,0.987189825241073,0.962438915249418,
0.987189825241073,0.962438915249418,0.987189825241073),(0.987189825241073,
0.962438915249418,0.987189825241073,0.962438915249418,0.987189825241073,
0.962438915249418,0.987189825241073,0.962438915249418,0.987189825241073),
(1.,0.974927912181824,1.,0.974927912181824,1.,0.974927912181824,1.,0.974927912181824,
1.)))
REPRESENTATION_ITEM('')
SURFACE()
);
#336=(
BOUNDED_SURFACE()
B_SPLINE_SURFACE(3,2,((#23319,#23320,#23321,#23322,#23323,#23324,#23325,
#23326,#23327),(#23328,#23329,#23330,#23331,#23332,#23333,#23334,#23335,
#23336),(#23337,#23338,#23339,#23340,#23341,#23342,#23343,#23344,#23345),
(#23346,#23347,#23348,#23349,#23350,#23351,#23352,#23353,#23354)),
 .UNSPECIFIED.,.F.,.F.,.F.)
B_SPLINE_SURFACE_WITH_KNOTS((4,4),(3,2,2,2,3),(0.,1.),(0.,0.25,0.5,0.75,
1.),.UNSPECIFIED.)
GEOMETRIC_REPRESENTATION_ITEM()
RATIONAL_B_SPLINE_SURFACE(((1.,0.974927912181824,1.,0.974927912181824,1.,
0.974927912181824,1.,0.974927912181824,1.),(0.833333333333332,0.812439926818185,
0.833333333333332,0.812439926818185,0.833333333333332,0.812439926818185,
0.833333333333332,0.812439926818185,0.833333333333332),(0.833333333333332,
0.812439926818185,0.833333333333332,0.812439926818185,0.833333333333332,
0.812439926818185,0.833333333333332,0.812439926818185,0.833333333333332),
(1.,0.974927912181824,1.,0.974927912181824,1.,0.974927912181824,1.,0.974927912181824,
1.)))
REPRESENTATION_ITEM('')
SURFACE()
);
#337=(
BOUNDED_SURFACE()
B_SPLINE_SURFACE(3,2,((#23358,#23359,#23360,#23361,#23362,#23363,#23364,
#23365,#23366),(#23367,#23368,#23369,#23370,#23371,#23372,#23373,#23374,
#23375),(#23376,#23377,#23378,#23379,#23380,#23381,#23382,#23383,#23384),
(#23385,#23386,#23387,#23388,#23389,#23390,#23391,#23392,#23393)),
 .UNSPECIFIED.,.F.,.F.,.F.)
B_SPLINE_SURFACE_WITH_KNOTS((4,4),(3,2,2,2,3),(0.,1.),(0.,0.25,0.5,0.75,
1.),.UNSPECIFIED.)
GEOMETRIC_REPRESENTATION_ITEM()
RATIONAL_B_SPLINE_SURFACE(((1.,0.974927912181824,1.,0.974927912181824,1.,
0.974927912181824,1.,0.974927912181824,1.),(0.987189825241073,0.962438915249418,
0.987189825241073,0.962438915249418,0.987189825241073,0.962438915249418,
0.987189825241073,0.962438915249418,0.987189825241073),(0.987189825241073,
0.962438915249418,0.987189825241073,0.962438915249418,0.987189825241073,
0.962438915249418,0.987189825241073,0.962438915249418,0.987189825241073),
(1.,0.974927912181824,1.,0.974927912181824,1.,0.974927912181824,1.,0.974927912181824,
1.)))
REPRESENTATION_ITEM('')
SURFACE()
);
#338=(
BOUNDED_SURFACE()
B_SPLINE_SURFACE(3,2,((#23448,#23449,#23450,#23451,#23452,#23453,#23454,
#23455,#23456),(#23457,#23458,#23459,#23460,#23461,#23462,#23463,#23464,
#23465),(#23466,#23467,#23468,#23469,#23470,#23471,#23472,#23473,#23474),
(#23475,#23476,#23477,#23478,#23479,#23480,#23481,#23482,#23483)),
 .UNSPECIFIED.,.F.,.F.,.F.)
B_SPLINE_SURFACE_WITH_KNOTS((4,4),(3,2,2,2,3),(0.,1.),(0.,0.25,0.5,0.75,
1.),.UNSPECIFIED.)
GEOMETRIC_REPRESENTATION_ITEM()
RATIONAL_B_SPLINE_SURFACE(((1.,0.974927912181824,1.,0.974927912181824,1.,
0.974927912181824,1.,0.974927912181824,1.),(0.987189825241073,0.962438915249418,
0.987189825241073,0.962438915249418,0.987189825241073,0.962438915249418,
0.987189825241073,0.962438915249418,0.987189825241073),(0.987189825241073,
0.962438915249418,0.987189825241073,0.962438915249418,0.987189825241073,
0.962438915249418,0.987189825241073,0.962438915249418,0.987189825241073),
(1.,0.974927912181824,1.,0.974927912181824,1.,0.974927912181824,1.,0.974927912181824,
1.)))
REPRESENTATION_ITEM('')
SURFACE()
);
#339=(
BOUNDED_SURFACE()
B_SPLINE_SURFACE(3,2,((#23491,#23492,#23493,#23494,#23495,#23496,#23497,
#23498,#23499),(#23500,#23501,#23502,#23503,#23504,#23505,#23506,#23507,
#23508),(#23509,#23510,#23511,#23512,#23513,#23514,#23515,#23516,#23517),
(#23518,#23519,#23520,#23521,#23522,#23523,#23524,#23525,#23526)),
 .UNSPECIFIED.,.F.,.F.,.F.)
B_SPLINE_SURFACE_WITH_KNOTS((4,4),(3,2,2,2,3),(0.,1.),(0.,0.25,0.5,0.75,
1.),.UNSPECIFIED.)
GEOMETRIC_REPRESENTATION_ITEM()
RATIONAL_B_SPLINE_SURFACE(((1.,0.974927912181824,1.,0.974927912181824,1.,
0.974927912181824,1.,0.974927912181824,1.),(0.833333333333333,0.812439926818186,
0.833333333333333,0.812439926818186,0.833333333333333,0.812439926818186,
0.833333333333333,0.812439926818186,0.833333333333333),(0.833333333333333,
0.812439926818186,0.833333333333333,0.812439926818186,0.833333333333333,
0.812439926818186,0.833333333333333,0.812439926818186,0.833333333333333),
(1.,0.974927912181824,1.,0.974927912181824,1.,0.974927912181824,1.,0.974927912181824,
1.)))
REPRESENTATION_ITEM('')
SURFACE()
);
#340=(
BOUNDED_SURFACE()
B_SPLINE_SURFACE(3,2,((#23530,#23531,#23532,#23533,#23534,#23535,#23536,
#23537,#23538),(#23539,#23540,#23541,#23542,#23543,#23544,#23545,#23546,
#23547),(#23548,#23549,#23550,#23551,#23552,#23553,#23554,#23555,#23556),
(#23557,#23558,#23559,#23560,#23561,#23562,#23563,#23564,#23565)),
 .UNSPECIFIED.,.F.,.F.,.F.)
B_SPLINE_SURFACE_WITH_KNOTS((4,4),(3,2,2,2,3),(0.,1.),(0.,0.25,0.5,0.75,
1.),.UNSPECIFIED.)
GEOMETRIC_REPRESENTATION_ITEM()
RATIONAL_B_SPLINE_SURFACE(((1.,0.974927912181824,1.,0.974927912181824,1.,
0.974927912181824,1.,0.974927912181824,1.),(0.987189825241073,0.962438915249418,
0.987189825241073,0.962438915249418,0.987189825241073,0.962438915249418,
0.987189825241073,0.962438915249418,0.987189825241073),(0.987189825241073,
0.962438915249418,0.987189825241073,0.962438915249418,0.987189825241073,
0.962438915249418,0.987189825241073,0.962438915249418,0.987189825241073),
(1.,0.974927912181824,1.,0.974927912181824,1.,0.974927912181824,1.,0.974927912181824,
1.)))
REPRESENTATION_ITEM('')
SURFACE()
);
#341=(
BOUNDED_SURFACE()
B_SPLINE_SURFACE(3,2,((#23573,#23574,#23575,#23576,#23577,#23578,#23579,
#23580,#23581),(#23582,#23583,#23584,#23585,#23586,#23587,#23588,#23589,
#23590),(#23591,#23592,#23593,#23594,#23595,#23596,#23597,#23598,#23599),
(#23600,#23601,#23602,#23603,#23604,#23605,#23606,#23607,#23608)),
 .UNSPECIFIED.,.F.,.F.,.F.)
B_SPLINE_SURFACE_WITH_KNOTS((4,4),(3,2,2,2,3),(0.,1.),(0.,0.25,0.5,0.75,
1.),.UNSPECIFIED.)
GEOMETRIC_REPRESENTATION_ITEM()
RATIONAL_B_SPLINE_SURFACE(((1.,0.974927912181824,1.,0.974927912181824,1.,
0.974927912181824,1.,0.974927912181824,1.),(0.987189825241073,0.962438915249418,
0.987189825241073,0.962438915249418,0.987189825241073,0.962438915249418,
0.987189825241073,0.962438915249418,0.987189825241073),(0.987189825241073,
0.962438915249418,0.987189825241073,0.962438915249418,0.987189825241073,
0.962438915249418,0.987189825241073,0.962438915249418,0.987189825241073),
(1.,0.974927912181824,1.,0.974927912181824,1.,0.974927912181824,1.,0.974927912181824,
1.)))
REPRESENTATION_ITEM('')
SURFACE()
);
#342=(
BOUNDED_SURFACE()
B_SPLINE_SURFACE(3,2,((#23616,#23617,#23618,#23619,#23620,#23621,#23622,
#23623,#23624),(#23625,#23626,#23627,#23628,#23629,#23630,#23631,#23632,
#23633),(#23634,#23635,#23636,#23637,#23638,#23639,#23640,#23641,#23642),
(#23643,#23644,#23645,#23646,#23647,#23648,#23649,#23650,#23651)),
 .UNSPECIFIED.,.F.,.F.,.F.)
B_SPLINE_SURFACE_WITH_KNOTS((4,4),(3,2,2,2,3),(0.,1.),(0.,0.25,0.5,0.75,
1.),.UNSPECIFIED.)
GEOMETRIC_REPRESENTATION_ITEM()
RATIONAL_B_SPLINE_SURFACE(((1.,0.974927912181824,1.,0.974927912181824,1.,
0.974927912181824,1.,0.974927912181824,1.),(0.833333333333331,0.812439926818184,
0.833333333333331,0.812439926818184,0.833333333333331,0.812439926818184,
0.833333333333331,0.812439926818184,0.833333333333331),(0.833333333333331,
0.812439926818184,0.833333333333331,0.812439926818184,0.833333333333331,
0.812439926818184,0.833333333333331,0.812439926818184,0.833333333333331),
(1.,0.974927912181824,1.,0.974927912181824,1.,0.974927912181824,1.,0.974927912181824,
1.)))
REPRESENTATION_ITEM('')
SURFACE()
);
#343=(
BOUNDED_SURFACE()
B_SPLINE_SURFACE(3,2,((#23655,#23656,#23657,#23658,#23659,#23660,#23661,
#23662,#23663),(#23664,#23665,#23666,#23667,#23668,#23669,#23670,#23671,
#23672),(#23673,#23674,#23675,#23676,#23677,#23678,#23679,#23680,#23681),
(#23682,#23683,#23684,#23685,#23686,#23687,#23688,#23689,#23690)),
 .UNSPECIFIED.,.F.,.F.,.F.)
B_SPLINE_SURFACE_WITH_KNOTS((4,4),(3,2,2,2,3),(0.,1.),(0.,0.25,0.5,0.75,
1.),.UNSPECIFIED.)
GEOMETRIC_REPRESENTATION_ITEM()
RATIONAL_B_SPLINE_SURFACE(((1.,0.974927912181824,1.,0.974927912181824,1.,
0.974927912181824,1.,0.974927912181824,1.),(0.987189825241073,0.962438915249418,
0.987189825241073,0.962438915249418,0.987189825241073,0.962438915249418,
0.987189825241073,0.962438915249418,0.987189825241073),(0.987189825241073,
0.962438915249418,0.987189825241073,0.962438915249418,0.987189825241073,
0.962438915249418,0.987189825241073,0.962438915249418,0.987189825241073),
(1.,0.974927912181824,1.,0.974927912181824,1.,0.974927912181824,1.,0.974927912181824,
1.)))
REPRESENTATION_ITEM('')
SURFACE()
);
#344=(
BOUNDED_SURFACE()
B_SPLINE_SURFACE(3,2,((#23745,#23746,#23747,#23748,#23749,#23750,#23751,
#23752,#23753),(#23754,#23755,#23756,#23757,#23758,#23759,#23760,#23761,
#23762),(#23763,#23764,#23765,#23766,#23767,#23768,#23769,#23770,#23771),
(#23772,#23773,#23774,#23775,#23776,#23777,#23778,#23779,#23780)),
 .UNSPECIFIED.,.F.,.F.,.F.)
B_SPLINE_SURFACE_WITH_KNOTS((4,4),(3,2,2,2,3),(0.,1.),(0.,0.25,0.5,0.75,
1.),.UNSPECIFIED.)
GEOMETRIC_REPRESENTATION_ITEM()
RATIONAL_B_SPLINE_SURFACE(((1.,0.974927912181824,1.,0.974927912181824,1.,
0.974927912181824,1.,0.974927912181824,1.),(0.987189825241073,0.962438915249418,
0.987189825241073,0.962438915249418,0.987189825241073,0.962438915249418,
0.987189825241073,0.962438915249418,0.987189825241073),(0.987189825241073,
0.962438915249418,0.987189825241073,0.962438915249418,0.987189825241073,
0.962438915249418,0.987189825241073,0.962438915249418,0.987189825241073),
(1.,0.974927912181824,1.,0.974927912181824,1.,0.974927912181824,1.,0.974927912181824,
1.)))
REPRESENTATION_ITEM('')
SURFACE()
);
#345=(
BOUNDED_SURFACE()
B_SPLINE_SURFACE(3,2,((#23788,#23789,#23790,#23791,#23792,#23793,#23794,
#23795,#23796),(#23797,#23798,#23799,#23800,#23801,#23802,#23803,#23804,
#23805),(#23806,#23807,#23808,#23809,#23810,#23811,#23812,#23813,#23814),
(#23815,#23816,#23817,#23818,#23819,#23820,#23821,#23822,#23823)),
 .UNSPECIFIED.,.F.,.F.,.F.)
B_SPLINE_SURFACE_WITH_KNOTS((4,4),(3,2,2,2,3),(0.,1.),(0.,0.25,0.5,0.75,
1.),.UNSPECIFIED.)
GEOMETRIC_REPRESENTATION_ITEM()
RATIONAL_B_SPLINE_SURFACE(((1.,0.974927912181824,1.,0.974927912181824,1.,
0.974927912181824,1.,0.974927912181824,1.),(0.833333333333333,0.812439926818186,
0.833333333333333,0.812439926818186,0.833333333333333,0.812439926818186,
0.833333333333333,0.812439926818186,0.833333333333333),(0.833333333333333,
0.812439926818186,0.833333333333333,0.812439926818186,0.833333333333333,
0.812439926818186,0.833333333333333,0.812439926818186,0.833333333333333),
(1.,0.974927912181824,1.,0.974927912181824,1.,0.974927912181824,1.,0.974927912181824,
1.)))
REPRESENTATION_ITEM('')
SURFACE()
);
#346=(
BOUNDED_SURFACE()
B_SPLINE_SURFACE(3,2,((#23827,#23828,#23829,#23830,#23831,#23832,#23833,
#23834,#23835),(#23836,#23837,#23838,#23839,#23840,#23841,#23842,#23843,
#23844),(#23845,#23846,#23847,#23848,#23849,#23850,#23851,#23852,#23853),
(#23854,#23855,#23856,#23857,#23858,#23859,#23860,#23861,#23862)),
 .UNSPECIFIED.,.F.,.F.,.F.)
B_SPLINE_SURFACE_WITH_KNOTS((4,4),(3,2,2,2,3),(0.,1.),(0.,0.25,0.5,0.75,
1.),.UNSPECIFIED.)
GEOMETRIC_REPRESENTATION_ITEM()
RATIONAL_B_SPLINE_SURFACE(((1.,0.974927912181824,1.,0.974927912181824,1.,
0.974927912181824,1.,0.974927912181824,1.),(0.987189825241073,0.962438915249418,
0.987189825241073,0.962438915249418,0.987189825241073,0.962438915249418,
0.987189825241073,0.962438915249418,0.987189825241073),(0.987189825241073,
0.962438915249418,0.987189825241073,0.962438915249418,0.987189825241073,
0.962438915249418,0.987189825241073,0.962438915249418,0.987189825241073),
(1.,0.974927912181824,1.,0.974927912181824,1.,0.974927912181824,1.,0.974927912181824,
1.)))
REPRESENTATION_ITEM('')
SURFACE()
);
#347=(
BOUNDED_SURFACE()
B_SPLINE_SURFACE(3,2,((#23917,#23918,#23919,#23920,#23921,#23922,#23923,
#23924,#23925),(#23926,#23927,#23928,#23929,#23930,#23931,#23932,#23933,
#23934),(#23935,#23936,#23937,#23938,#23939,#23940,#23941,#23942,#23943),
(#23944,#23945,#23946,#23947,#23948,#23949,#23950,#23951,#23952)),
 .UNSPECIFIED.,.F.,.F.,.F.)
B_SPLINE_SURFACE_WITH_KNOTS((4,4),(3,2,2,2,3),(0.,1.),(0.,0.25,0.5,0.75,
1.),.UNSPECIFIED.)
GEOMETRIC_REPRESENTATION_ITEM()
RATIONAL_B_SPLINE_SURFACE(((1.,0.974927912181824,1.,0.974927912181824,1.,
0.974927912181824,1.,0.974927912181824,1.),(0.987189825241073,0.962438915249418,
0.987189825241073,0.962438915249418,0.987189825241073,0.962438915249418,
0.987189825241073,0.962438915249418,0.987189825241073),(0.987189825241073,
0.962438915249418,0.987189825241073,0.962438915249418,0.987189825241073,
0.962438915249418,0.987189825241073,0.962438915249418,0.987189825241073),
(1.,0.974927912181824,1.,0.974927912181824,1.,0.974927912181824,1.,0.974927912181824,
1.)))
REPRESENTATION_ITEM('')
SURFACE()
);
#348=(
BOUNDED_SURFACE()
B_SPLINE_SURFACE(3,2,((#23960,#23961,#23962,#23963,#23964,#23965,#23966,
#23967,#23968),(#23969,#23970,#23971,#23972,#23973,#23974,#23975,#23976,
#23977),(#23978,#23979,#23980,#23981,#23982,#23983,#23984,#23985,#23986),
(#23987,#23988,#23989,#23990,#23991,#23992,#23993,#23994,#23995)),
 .UNSPECIFIED.,.F.,.F.,.F.)
B_SPLINE_SURFACE_WITH_KNOTS((4,4),(3,2,2,2,3),(0.,1.),(0.,0.25,0.5,0.75,
1.),.UNSPECIFIED.)
GEOMETRIC_REPRESENTATION_ITEM()
RATIONAL_B_SPLINE_SURFACE(((1.,0.974927912181824,1.,0.974927912181824,1.,
0.974927912181824,1.,0.974927912181824,1.),(0.833333333333332,0.812439926818185,
0.833333333333332,0.812439926818185,0.833333333333332,0.812439926818185,
0.833333333333332,0.812439926818185,0.833333333333332),(0.833333333333332,
0.812439926818185,0.833333333333332,0.812439926818185,0.833333333333332,
0.812439926818185,0.833333333333332,0.812439926818185,0.833333333333332),
(1.,0.974927912181824,1.,0.974927912181824,1.,0.974927912181824,1.,0.974927912181824,
1.)))
REPRESENTATION_ITEM('')
SURFACE()
);
#349=(
BOUNDED_SURFACE()
B_SPLINE_SURFACE(3,2,((#23999,#24000,#24001,#24002,#24003,#24004,#24005,
#24006,#24007),(#24008,#24009,#24010,#24011,#24012,#24013,#24014,#24015,
#24016),(#24017,#24018,#24019,#24020,#24021,#24022,#24023,#24024,#24025),
(#24026,#24027,#24028,#24029,#24030,#24031,#24032,#24033,#24034)),
 .UNSPECIFIED.,.F.,.F.,.F.)
B_SPLINE_SURFACE_WITH_KNOTS((4,4),(3,2,2,2,3),(0.,1.),(0.,0.25,0.5,0.75,
1.),.UNSPECIFIED.)
GEOMETRIC_REPRESENTATION_ITEM()
RATIONAL_B_SPLINE_SURFACE(((1.,0.974927912181824,1.,0.974927912181824,1.,
0.974927912181824,1.,0.974927912181824,1.),(0.987189825241073,0.962438915249418,
0.987189825241073,0.962438915249418,0.987189825241073,0.962438915249418,
0.987189825241073,0.962438915249418,0.987189825241073),(0.987189825241073,
0.962438915249418,0.987189825241073,0.962438915249418,0.987189825241073,
0.962438915249418,0.987189825241073,0.962438915249418,0.987189825241073),
(1.,0.974927912181824,1.,0.974927912181824,1.,0.974927912181824,1.,0.974927912181824,
1.)))
REPRESENTATION_ITEM('')
SURFACE()
);
#350=(
BOUNDED_SURFACE()
B_SPLINE_SURFACE(3,2,((#24089,#24090,#24091,#24092,#24093,#24094,#24095,
#24096,#24097),(#24098,#24099,#24100,#24101,#24102,#24103,#24104,#24105,
#24106),(#24107,#24108,#24109,#24110,#24111,#24112,#24113,#24114,#24115),
(#24116,#24117,#24118,#24119,#24120,#24121,#24122,#24123,#24124)),
 .UNSPECIFIED.,.F.,.F.,.F.)
B_SPLINE_SURFACE_WITH_KNOTS((4,4),(3,2,2,2,3),(0.,1.),(0.,0.25,0.5,0.75,
1.),.UNSPECIFIED.)
GEOMETRIC_REPRESENTATION_ITEM()
RATIONAL_B_SPLINE_SURFACE(((1.,0.974927912181824,1.,0.974927912181824,1.,
0.974927912181824,1.,0.974927912181824,1.),(0.987189825241073,0.962438915249418,
0.987189825241073,0.962438915249418,0.987189825241073,0.962438915249418,
0.987189825241073,0.962438915249418,0.987189825241073),(0.987189825241073,
0.962438915249418,0.987189825241073,0.962438915249418,0.987189825241073,
0.962438915249418,0.987189825241073,0.962438915249418,0.987189825241073),
(1.,0.974927912181824,1.,0.974927912181824,1.,0.974927912181824,1.,0.974927912181824,
1.)))
REPRESENTATION_ITEM('')
SURFACE()
);
#351=(
BOUNDED_SURFACE()
B_SPLINE_SURFACE(3,2,((#24132,#24133,#24134,#24135,#24136,#24137,#24138,
#24139,#24140),(#24141,#24142,#24143,#24144,#24145,#24146,#24147,#24148,
#24149),(#24150,#24151,#24152,#24153,#24154,#24155,#24156,#24157,#24158),
(#24159,#24160,#24161,#24162,#24163,#24164,#24165,#24166,#24167)),
 .UNSPECIFIED.,.F.,.F.,.F.)
B_SPLINE_SURFACE_WITH_KNOTS((4,4),(3,2,2,2,3),(0.,1.),(0.,0.25,0.5,0.75,
1.),.UNSPECIFIED.)
GEOMETRIC_REPRESENTATION_ITEM()
RATIONAL_B_SPLINE_SURFACE(((1.,0.974927912181824,1.,0.974927912181824,1.,
0.974927912181824,1.,0.974927912181824,1.),(0.833333333333332,0.812439926818185,
0.833333333333332,0.812439926818185,0.833333333333332,0.812439926818185,
0.833333333333332,0.812439926818185,0.833333333333332),(0.833333333333332,
0.812439926818185,0.833333333333332,0.812439926818185,0.833333333333332,
0.812439926818185,0.833333333333332,0.812439926818185,0.833333333333332),
(1.,0.974927912181824,1.,0.974927912181824,1.,0.974927912181824,1.,0.974927912181824,
1.)))
REPRESENTATION_ITEM('')
SURFACE()
);
#352=(
BOUNDED_SURFACE()
B_SPLINE_SURFACE(3,2,((#24171,#24172,#24173,#24174,#24175,#24176,#24177,
#24178,#24179),(#24180,#24181,#24182,#24183,#24184,#24185,#24186,#24187,
#24188),(#24189,#24190,#24191,#24192,#24193,#24194,#24195,#24196,#24197),
(#24198,#24199,#24200,#24201,#24202,#24203,#24204,#24205,#24206)),
 .UNSPECIFIED.,.F.,.F.,.F.)
B_SPLINE_SURFACE_WITH_KNOTS((4,4),(3,2,2,2,3),(0.,1.),(0.,0.25,0.5,0.75,
1.),.UNSPECIFIED.)
GEOMETRIC_REPRESENTATION_ITEM()
RATIONAL_B_SPLINE_SURFACE(((1.,0.974927912181824,1.,0.974927912181824,1.,
0.974927912181824,1.,0.974927912181824,1.),(0.987189825241073,0.962438915249418,
0.987189825241073,0.962438915249418,0.987189825241073,0.962438915249418,
0.987189825241073,0.962438915249418,0.987189825241073),(0.987189825241073,
0.962438915249418,0.987189825241073,0.962438915249418,0.987189825241073,
0.962438915249418,0.987189825241073,0.962438915249418,0.987189825241073),
(1.,0.974927912181824,1.,0.974927912181824,1.,0.974927912181824,1.,0.974927912181824,
1.)))
REPRESENTATION_ITEM('')
SURFACE()
);
#353=(
BOUNDED_SURFACE()
B_SPLINE_SURFACE(3,2,((#24261,#24262,#24263,#24264,#24265,#24266,#24267,
#24268,#24269),(#24270,#24271,#24272,#24273,#24274,#24275,#24276,#24277,
#24278),(#24279,#24280,#24281,#24282,#24283,#24284,#24285,#24286,#24287),
(#24288,#24289,#24290,#24291,#24292,#24293,#24294,#24295,#24296)),
 .UNSPECIFIED.,.F.,.F.,.F.)
B_SPLINE_SURFACE_WITH_KNOTS((4,4),(3,2,2,2,3),(0.,1.),(0.,0.25,0.5,0.75,
1.),.UNSPECIFIED.)
GEOMETRIC_REPRESENTATION_ITEM()
RATIONAL_B_SPLINE_SURFACE(((1.,0.974927912181824,1.,0.974927912181824,1.,
0.974927912181824,1.,0.974927912181824,1.),(0.987189825241073,0.962438915249418,
0.987189825241073,0.962438915249418,0.987189825241073,0.962438915249418,
0.987189825241073,0.962438915249418,0.987189825241073),(0.987189825241073,
0.962438915249418,0.987189825241073,0.962438915249418,0.987189825241073,
0.962438915249418,0.987189825241073,0.962438915249418,0.987189825241073),
(1.,0.974927912181824,1.,0.974927912181824,1.,0.974927912181824,1.,0.974927912181824,
1.)))
REPRESENTATION_ITEM('')
SURFACE()
);
#354=(
BOUNDED_SURFACE()
B_SPLINE_SURFACE(3,2,((#24304,#24305,#24306,#24307,#24308,#24309,#24310,
#24311,#24312),(#24313,#24314,#24315,#24316,#24317,#24318,#24319,#24320,
#24321),(#24322,#24323,#24324,#24325,#24326,#24327,#24328,#24329,#24330),
(#24331,#24332,#24333,#24334,#24335,#24336,#24337,#24338,#24339)),
 .UNSPECIFIED.,.F.,.F.,.F.)
B_SPLINE_SURFACE_WITH_KNOTS((4,4),(3,2,2,2,3),(0.,1.),(0.,0.25,0.5,0.75,
1.),.UNSPECIFIED.)
GEOMETRIC_REPRESENTATION_ITEM()
RATIONAL_B_SPLINE_SURFACE(((1.,0.974927912181824,1.,0.974927912181824,1.,
0.974927912181824,1.,0.974927912181824,1.),(0.833333333333333,0.812439926818186,
0.833333333333333,0.812439926818186,0.833333333333333,0.812439926818186,
0.833333333333333,0.812439926818186,0.833333333333333),(0.833333333333333,
0.812439926818186,0.833333333333333,0.812439926818186,0.833333333333333,
0.812439926818186,0.833333333333333,0.812439926818186,0.833333333333333),
(1.,0.974927912181824,1.,0.974927912181824,1.,0.974927912181824,1.,0.974927912181824,
1.)))
REPRESENTATION_ITEM('')
SURFACE()
);
#355=(
BOUNDED_SURFACE()
B_SPLINE_SURFACE(3,2,((#24343,#24344,#24345,#24346,#24347,#24348,#24349,
#24350,#24351),(#24352,#24353,#24354,#24355,#24356,#24357,#24358,#24359,
#24360),(#24361,#24362,#24363,#24364,#24365,#24366,#24367,#24368,#24369),
(#24370,#24371,#24372,#24373,#24374,#24375,#24376,#24377,#24378)),
 .UNSPECIFIED.,.F.,.F.,.F.)
B_SPLINE_SURFACE_WITH_KNOTS((4,4),(3,2,2,2,3),(0.,1.),(0.,0.25,0.5,0.75,
1.),.UNSPECIFIED.)
GEOMETRIC_REPRESENTATION_ITEM()
RATIONAL_B_SPLINE_SURFACE(((1.,0.974927912181824,1.,0.974927912181824,1.,
0.974927912181824,1.,0.974927912181824,1.),(0.987189825241073,0.962438915249418,
0.987189825241073,0.962438915249418,0.987189825241073,0.962438915249418,
0.987189825241073,0.962438915249418,0.987189825241073),(0.987189825241073,
0.962438915249418,0.987189825241073,0.962438915249418,0.987189825241073,
0.962438915249418,0.987189825241073,0.962438915249418,0.987189825241073),
(1.,0.974927912181824,1.,0.974927912181824,1.,0.974927912181824,1.,0.974927912181824,
1.)))
REPRESENTATION_ITEM('')
SURFACE()
);
#356=(
BOUNDED_SURFACE()
B_SPLINE_SURFACE(3,2,((#24433,#24434,#24435,#24436,#24437,#24438,#24439,
#24440,#24441),(#24442,#24443,#24444,#24445,#24446,#24447,#24448,#24449,
#24450),(#24451,#24452,#24453,#24454,#24455,#24456,#24457,#24458,#24459),
(#24460,#24461,#24462,#24463,#24464,#24465,#24466,#24467,#24468)),
 .UNSPECIFIED.,.F.,.F.,.F.)
B_SPLINE_SURFACE_WITH_KNOTS((4,4),(3,2,2,2,3),(0.,1.),(0.,0.25,0.5,0.75,
1.),.UNSPECIFIED.)
GEOMETRIC_REPRESENTATION_ITEM()
RATIONAL_B_SPLINE_SURFACE(((1.,0.974927912181824,1.,0.974927912181824,1.,
0.974927912181824,1.,0.974927912181824,1.),(0.987189825241073,0.962438915249418,
0.987189825241073,0.962438915249418,0.987189825241073,0.962438915249418,
0.987189825241073,0.962438915249418,0.987189825241073),(0.987189825241073,
0.962438915249418,0.987189825241073,0.962438915249418,0.987189825241073,
0.962438915249418,0.987189825241073,0.962438915249418,0.987189825241073),
(1.,0.974927912181824,1.,0.974927912181824,1.,0.974927912181824,1.,0.974927912181824,
1.)))
REPRESENTATION_ITEM('')
SURFACE()
);
#357=(
BOUNDED_SURFACE()
B_SPLINE_SURFACE(3,2,((#24476,#24477,#24478,#24479,#24480,#24481,#24482,
#24483,#24484),(#24485,#24486,#24487,#24488,#24489,#24490,#24491,#24492,
#24493),(#24494,#24495,#24496,#24497,#24498,#24499,#24500,#24501,#24502),
(#24503,#24504,#24505,#24506,#24507,#24508,#24509,#24510,#24511)),
 .UNSPECIFIED.,.F.,.F.,.F.)
B_SPLINE_SURFACE_WITH_KNOTS((4,4),(3,2,2,2,3),(0.,1.),(0.,0.25,0.5,0.75,
1.),.UNSPECIFIED.)
GEOMETRIC_REPRESENTATION_ITEM()
RATIONAL_B_SPLINE_SURFACE(((1.,0.974927912181824,1.,0.974927912181824,1.,
0.974927912181824,1.,0.974927912181824,1.),(0.833333333333331,0.812439926818184,
0.833333333333331,0.812439926818184,0.833333333333331,0.812439926818184,
0.833333333333331,0.812439926818184,0.833333333333331),(0.833333333333331,
0.812439926818184,0.833333333333331,0.812439926818184,0.833333333333331,
0.812439926818184,0.833333333333331,0.812439926818184,0.833333333333331),
(1.,0.974927912181824,1.,0.974927912181824,1.,0.974927912181824,1.,0.974927912181824,
1.)))
REPRESENTATION_ITEM('')
SURFACE()
);
#358=(
BOUNDED_SURFACE()
B_SPLINE_SURFACE(3,2,((#24515,#24516,#24517,#24518,#24519,#24520,#24521,
#24522,#24523),(#24524,#24525,#24526,#24527,#24528,#24529,#24530,#24531,
#24532),(#24533,#24534,#24535,#24536,#24537,#24538,#24539,#24540,#24541),
(#24542,#24543,#24544,#24545,#24546,#24547,#24548,#24549,#24550)),
 .UNSPECIFIED.,.F.,.F.,.F.)
B_SPLINE_SURFACE_WITH_KNOTS((4,4),(3,2,2,2,3),(0.,1.),(0.,0.25,0.5,0.75,
1.),.UNSPECIFIED.)
GEOMETRIC_REPRESENTATION_ITEM()
RATIONAL_B_SPLINE_SURFACE(((1.,0.974927912181824,1.,0.974927912181824,1.,
0.974927912181824,1.,0.974927912181824,1.),(0.987189825241073,0.962438915249418,
0.987189825241073,0.962438915249418,0.987189825241073,0.962438915249418,
0.987189825241073,0.962438915249418,0.987189825241073),(0.987189825241073,
0.962438915249418,0.987189825241073,0.962438915249418,0.987189825241073,
0.962438915249418,0.987189825241073,0.962438915249418,0.987189825241073),
(1.,0.974927912181824,1.,0.974927912181824,1.,0.974927912181824,1.,0.974927912181824,
1.)))
REPRESENTATION_ITEM('')
SURFACE()
);
#359=(
BOUNDED_SURFACE()
B_SPLINE_SURFACE(3,2,((#24605,#24606,#24607,#24608,#24609,#24610,#24611,
#24612,#24613),(#24614,#24615,#24616,#24617,#24618,#24619,#24620,#24621,
#24622),(#24623,#24624,#24625,#24626,#24627,#24628,#24629,#24630,#24631),
(#24632,#24633,#24634,#24635,#24636,#24637,#24638,#24639,#24640)),
 .UNSPECIFIED.,.F.,.F.,.F.)
B_SPLINE_SURFACE_WITH_KNOTS((4,4),(3,2,2,2,3),(0.,1.),(0.,0.25,0.5,0.75,
1.),.UNSPECIFIED.)
GEOMETRIC_REPRESENTATION_ITEM()
RATIONAL_B_SPLINE_SURFACE(((1.,0.974927912181824,1.,0.974927912181824,1.,
0.974927912181824,1.,0.974927912181824,1.),(0.987189825241073,0.962438915249418,
0.987189825241073,0.962438915249418,0.987189825241073,0.962438915249418,
0.987189825241073,0.962438915249418,0.987189825241073),(0.987189825241073,
0.962438915249418,0.987189825241073,0.962438915249418,0.987189825241073,
0.962438915249418,0.987189825241073,0.962438915249418,0.987189825241073),
(1.,0.974927912181824,1.,0.974927912181824,1.,0.974927912181824,1.,0.974927912181824,
1.)))
REPRESENTATION_ITEM('')
SURFACE()
);
#360=(
BOUNDED_SURFACE()
B_SPLINE_SURFACE(3,2,((#24648,#24649,#24650,#24651,#24652,#24653,#24654,
#24655,#24656),(#24657,#24658,#24659,#24660,#24661,#24662,#24663,#24664,
#24665),(#24666,#24667,#24668,#24669,#24670,#24671,#24672,#24673,#24674),
(#24675,#24676,#24677,#24678,#24679,#24680,#24681,#24682,#24683)),
 .UNSPECIFIED.,.F.,.F.,.F.)
B_SPLINE_SURFACE_WITH_KNOTS((4,4),(3,2,2,2,3),(0.,1.),(0.,0.25,0.5,0.75,
1.),.UNSPECIFIED.)
GEOMETRIC_REPRESENTATION_ITEM()
RATIONAL_B_SPLINE_SURFACE(((1.,0.974927912181824,1.,0.974927912181824,1.,
0.974927912181824,1.,0.974927912181824,1.),(0.833333333333332,0.812439926818185,
0.833333333333332,0.812439926818185,0.833333333333332,0.812439926818185,
0.833333333333332,0.812439926818185,0.833333333333332),(0.833333333333332,
0.812439926818185,0.833333333333332,0.812439926818185,0.833333333333332,
0.812439926818185,0.833333333333332,0.812439926818185,0.833333333333332),
(1.,0.974927912181824,1.,0.974927912181824,1.,0.974927912181824,1.,0.974927912181824,
1.)))
REPRESENTATION_ITEM('')
SURFACE()
);
#361=(
BOUNDED_SURFACE()
B_SPLINE_SURFACE(3,2,((#24687,#24688,#24689,#24690,#24691,#24692,#24693,
#24694,#24695),(#24696,#24697,#24698,#24699,#24700,#24701,#24702,#24703,
#24704),(#24705,#24706,#24707,#24708,#24709,#24710,#24711,#24712,#24713),
(#24714,#24715,#24716,#24717,#24718,#24719,#24720,#24721,#24722)),
 .UNSPECIFIED.,.F.,.F.,.F.)
B_SPLINE_SURFACE_WITH_KNOTS((4,4),(3,2,2,2,3),(0.,1.),(0.,0.25,0.5,0.75,
1.),.UNSPECIFIED.)
GEOMETRIC_REPRESENTATION_ITEM()
RATIONAL_B_SPLINE_SURFACE(((1.,0.974927912181824,1.,0.974927912181824,1.,
0.974927912181824,1.,0.974927912181824,1.),(0.987189825241073,0.962438915249418,
0.987189825241073,0.962438915249418,0.987189825241073,0.962438915249418,
0.987189825241073,0.962438915249418,0.987189825241073),(0.987189825241073,
0.962438915249418,0.987189825241073,0.962438915249418,0.987189825241073,
0.962438915249418,0.987189825241073,0.962438915249418,0.987189825241073),
(1.,0.974927912181824,1.,0.974927912181824,1.,0.974927912181824,1.,0.974927912181824,
1.)))
REPRESENTATION_ITEM('')
SURFACE()
);
#362=(
BOUNDED_SURFACE()
B_SPLINE_SURFACE(3,2,((#24777,#24778,#24779,#24780,#24781,#24782,#24783,
#24784,#24785),(#24786,#24787,#24788,#24789,#24790,#24791,#24792,#24793,
#24794),(#24795,#24796,#24797,#24798,#24799,#24800,#24801,#24802,#24803),
(#24804,#24805,#24806,#24807,#24808,#24809,#24810,#24811,#24812)),
 .UNSPECIFIED.,.F.,.F.,.F.)
B_SPLINE_SURFACE_WITH_KNOTS((4,4),(3,2,2,2,3),(0.,1.),(0.,0.25,0.5,0.75,
1.),.UNSPECIFIED.)
GEOMETRIC_REPRESENTATION_ITEM()
RATIONAL_B_SPLINE_SURFACE(((1.,0.974927912181824,1.,0.974927912181824,1.,
0.974927912181824,1.,0.974927912181824,1.),(0.987189825241073,0.962438915249418,
0.987189825241073,0.962438915249418,0.987189825241073,0.962438915249418,
0.987189825241073,0.962438915249418,0.987189825241073),(0.987189825241073,
0.962438915249418,0.987189825241073,0.962438915249418,0.987189825241073,
0.962438915249418,0.987189825241073,0.962438915249418,0.987189825241073),
(1.,0.974927912181824,1.,0.974927912181824,1.,0.974927912181824,1.,0.974927912181824,
1.)))
REPRESENTATION_ITEM('')
SURFACE()
);
#363=(
BOUNDED_SURFACE()
B_SPLINE_SURFACE(3,2,((#24820,#24821,#24822,#24823,#24824,#24825,#24826,
#24827,#24828),(#24829,#24830,#24831,#24832,#24833,#24834,#24835,#24836,
#24837),(#24838,#24839,#24840,#24841,#24842,#24843,#24844,#24845,#24846),
(#24847,#24848,#24849,#24850,#24851,#24852,#24853,#24854,#24855)),
 .UNSPECIFIED.,.F.,.F.,.F.)
B_SPLINE_SURFACE_WITH_KNOTS((4,4),(3,2,2,2,3),(0.,1.),(0.,0.25,0.5,0.75,
1.),.UNSPECIFIED.)
GEOMETRIC_REPRESENTATION_ITEM()
RATIONAL_B_SPLINE_SURFACE(((1.,0.974927912181824,1.,0.974927912181824,1.,
0.974927912181824,1.,0.974927912181824,1.),(0.833333333333332,0.812439926818185,
0.833333333333332,0.812439926818185,0.833333333333332,0.812439926818185,
0.833333333333332,0.812439926818185,0.833333333333332),(0.833333333333332,
0.812439926818185,0.833333333333332,0.812439926818185,0.833333333333332,
0.812439926818185,0.833333333333332,0.812439926818185,0.833333333333332),
(1.,0.974927912181824,1.,0.974927912181824,1.,0.974927912181824,1.,0.974927912181824,
1.)))
REPRESENTATION_ITEM('')
SURFACE()
);
#364=(
BOUNDED_SURFACE()
B_SPLINE_SURFACE(3,2,((#24859,#24860,#24861,#24862,#24863,#24864,#24865,
#24866,#24867),(#24868,#24869,#24870,#24871,#24872,#24873,#24874,#24875,
#24876),(#24877,#24878,#24879,#24880,#24881,#24882,#24883,#24884,#24885),
(#24886,#24887,#24888,#24889,#24890,#24891,#24892,#24893,#24894)),
 .UNSPECIFIED.,.F.,.F.,.F.)
B_SPLINE_SURFACE_WITH_KNOTS((4,4),(3,2,2,2,3),(0.,1.),(0.,0.25,0.5,0.75,
1.),.UNSPECIFIED.)
GEOMETRIC_REPRESENTATION_ITEM()
RATIONAL_B_SPLINE_SURFACE(((1.,0.974927912181824,1.,0.974927912181824,1.,
0.974927912181824,1.,0.974927912181824,1.),(0.987189825241073,0.962438915249418,
0.987189825241073,0.962438915249418,0.987189825241073,0.962438915249418,
0.987189825241073,0.962438915249418,0.987189825241073),(0.987189825241073,
0.962438915249418,0.987189825241073,0.962438915249418,0.987189825241073,
0.962438915249418,0.987189825241073,0.962438915249418,0.987189825241073),
(1.,0.974927912181824,1.,0.974927912181824,1.,0.974927912181824,1.,0.974927912181824,
1.)))
REPRESENTATION_ITEM('')
SURFACE()
);
#365=(
BOUNDED_SURFACE()
B_SPLINE_SURFACE(3,2,((#24949,#24950,#24951,#24952,#24953,#24954,#24955,
#24956,#24957),(#24958,#24959,#24960,#24961,#24962,#24963,#24964,#24965,
#24966),(#24967,#24968,#24969,#24970,#24971,#24972,#24973,#24974,#24975),
(#24976,#24977,#24978,#24979,#24980,#24981,#24982,#24983,#24984)),
 .UNSPECIFIED.,.F.,.F.,.F.)
B_SPLINE_SURFACE_WITH_KNOTS((4,4),(3,2,2,2,3),(0.,1.),(0.,0.25,0.5,0.75,
1.),.UNSPECIFIED.)
GEOMETRIC_REPRESENTATION_ITEM()
RATIONAL_B_SPLINE_SURFACE(((1.,0.974927912181824,1.,0.974927912181824,1.,
0.974927912181824,1.,0.974927912181824,1.),(0.987189825241073,0.962438915249418,
0.987189825241073,0.962438915249418,0.987189825241073,0.962438915249418,
0.987189825241073,0.962438915249418,0.987189825241073),(0.987189825241073,
0.962438915249418,0.987189825241073,0.962438915249418,0.987189825241073,
0.962438915249418,0.987189825241073,0.962438915249418,0.987189825241073),
(1.,0.974927912181824,1.,0.974927912181824,1.,0.974927912181824,1.,0.974927912181824,
1.)))
REPRESENTATION_ITEM('')
SURFACE()
);
#366=(
BOUNDED_SURFACE()
B_SPLINE_SURFACE(3,2,((#24992,#24993,#24994,#24995,#24996,#24997,#24998,
#24999,#25000),(#25001,#25002,#25003,#25004,#25005,#25006,#25007,#25008,
#25009),(#25010,#25011,#25012,#25013,#25014,#25015,#25016,#25017,#25018),
(#25019,#25020,#25021,#25022,#25023,#25024,#25025,#25026,#25027)),
 .UNSPECIFIED.,.F.,.F.,.F.)
B_SPLINE_SURFACE_WITH_KNOTS((4,4),(3,2,2,2,3),(0.,1.),(0.,0.25,0.5,0.75,
1.),.UNSPECIFIED.)
GEOMETRIC_REPRESENTATION_ITEM()
RATIONAL_B_SPLINE_SURFACE(((1.,0.974927912181824,1.,0.974927912181824,1.,
0.974927912181824,1.,0.974927912181824,1.),(0.833333333333332,0.812439926818185,
0.833333333333332,0.812439926818185,0.833333333333332,0.812439926818185,
0.833333333333332,0.812439926818185,0.833333333333332),(0.833333333333332,
0.812439926818185,0.833333333333332,0.812439926818185,0.833333333333332,
0.812439926818185,0.833333333333332,0.812439926818185,0.833333333333332),
(1.,0.974927912181824,1.,0.974927912181824,1.,0.974927912181824,1.,0.974927912181824,
1.)))
REPRESENTATION_ITEM('')
SURFACE()
);
#367=(
BOUNDED_SURFACE()
B_SPLINE_SURFACE(3,2,((#25031,#25032,#25033,#25034,#25035,#25036,#25037,
#25038,#25039),(#25040,#25041,#25042,#25043,#25044,#25045,#25046,#25047,
#25048),(#25049,#25050,#25051,#25052,#25053,#25054,#25055,#25056,#25057),
(#25058,#25059,#25060,#25061,#25062,#25063,#25064,#25065,#25066)),
 .UNSPECIFIED.,.F.,.F.,.F.)
B_SPLINE_SURFACE_WITH_KNOTS((4,4),(3,2,2,2,3),(0.,1.),(0.,0.25,0.5,0.75,
1.),.UNSPECIFIED.)
GEOMETRIC_REPRESENTATION_ITEM()
RATIONAL_B_SPLINE_SURFACE(((1.,0.974927912181824,1.,0.974927912181824,1.,
0.974927912181824,1.,0.974927912181824,1.),(0.987189825241073,0.962438915249418,
0.987189825241073,0.962438915249418,0.987189825241073,0.962438915249418,
0.987189825241073,0.962438915249418,0.987189825241073),(0.987189825241073,
0.962438915249418,0.987189825241073,0.962438915249418,0.987189825241073,
0.962438915249418,0.987189825241073,0.962438915249418,0.987189825241073),
(1.,0.974927912181824,1.,0.974927912181824,1.,0.974927912181824,1.,0.974927912181824,
1.)))
REPRESENTATION_ITEM('')
SURFACE()
);
#368=(
BOUNDED_SURFACE()
B_SPLINE_SURFACE(3,2,((#25074,#25075,#25076,#25077,#25078,#25079,#25080,
#25081,#25082),(#25083,#25084,#25085,#25086,#25087,#25088,#25089,#25090,
#25091),(#25092,#25093,#25094,#25095,#25096,#25097,#25098,#25099,#25100),
(#25101,#25102,#25103,#25104,#25105,#25106,#25107,#25108,#25109)),
 .UNSPECIFIED.,.F.,.F.,.F.)
B_SPLINE_SURFACE_WITH_KNOTS((4,4),(3,2,2,2,3),(0.,1.),(0.,0.25,0.5,0.75,
1.),.UNSPECIFIED.)
GEOMETRIC_REPRESENTATION_ITEM()
RATIONAL_B_SPLINE_SURFACE(((1.,0.974927912181824,1.,0.974927912181824,1.,
0.974927912181824,1.,0.974927912181824,1.),(0.987189825241073,0.962438915249418,
0.987189825241073,0.962438915249418,0.987189825241073,0.962438915249418,
0.987189825241073,0.962438915249418,0.987189825241073),(0.987189825241073,
0.962438915249418,0.987189825241073,0.962438915249418,0.987189825241073,
0.962438915249418,0.987189825241073,0.962438915249418,0.987189825241073),
(1.,0.974927912181824,1.,0.974927912181824,1.,0.974927912181824,1.,0.974927912181824,
1.)))
REPRESENTATION_ITEM('')
SURFACE()
);
#369=(
BOUNDED_SURFACE()
B_SPLINE_SURFACE(3,2,((#25117,#25118,#25119,#25120,#25121,#25122,#25123,
#25124,#25125),(#25126,#25127,#25128,#25129,#25130,#25131,#25132,#25133,
#25134),(#25135,#25136,#25137,#25138,#25139,#25140,#25141,#25142,#25143),
(#25144,#25145,#25146,#25147,#25148,#25149,#25150,#25151,#25152)),
 .UNSPECIFIED.,.F.,.F.,.F.)
B_SPLINE_SURFACE_WITH_KNOTS((4,4),(3,2,2,2,3),(0.,1.),(0.,0.25,0.5,0.75,
1.),.UNSPECIFIED.)
GEOMETRIC_REPRESENTATION_ITEM()
RATIONAL_B_SPLINE_SURFACE(((1.,0.974927912181824,1.,0.974927912181824,1.,
0.974927912181824,1.,0.974927912181824,1.),(0.833333333333332,0.812439926818185,
0.833333333333332,0.812439926818185,0.833333333333332,0.812439926818185,
0.833333333333332,0.812439926818185,0.833333333333332),(0.833333333333332,
0.812439926818185,0.833333333333332,0.812439926818185,0.833333333333332,
0.812439926818185,0.833333333333332,0.812439926818185,0.833333333333332),
(1.,0.974927912181824,1.,0.974927912181824,1.,0.974927912181824,1.,0.974927912181824,
1.)))
REPRESENTATION_ITEM('')
SURFACE()
);
#370=(
BOUNDED_SURFACE()
B_SPLINE_SURFACE(3,2,((#25156,#25157,#25158,#25159,#25160,#25161,#25162,
#25163,#25164),(#25165,#25166,#25167,#25168,#25169,#25170,#25171,#25172,
#25173),(#25174,#25175,#25176,#25177,#25178,#25179,#25180,#25181,#25182),
(#25183,#25184,#25185,#25186,#25187,#25188,#25189,#25190,#25191)),
 .UNSPECIFIED.,.F.,.F.,.F.)
B_SPLINE_SURFACE_WITH_KNOTS((4,4),(3,2,2,2,3),(0.,1.),(0.,0.25,0.5,0.75,
1.),.UNSPECIFIED.)
GEOMETRIC_REPRESENTATION_ITEM()
RATIONAL_B_SPLINE_SURFACE(((1.,0.974927912181824,1.,0.974927912181824,1.,
0.974927912181824,1.,0.974927912181824,1.),(0.987189825241073,0.962438915249418,
0.987189825241073,0.962438915249418,0.987189825241073,0.962438915249418,
0.987189825241073,0.962438915249418,0.987189825241073),(0.987189825241073,
0.962438915249418,0.987189825241073,0.962438915249418,0.987189825241073,
0.962438915249418,0.987189825241073,0.962438915249418,0.987189825241073),
(1.,0.974927912181824,1.,0.974927912181824,1.,0.974927912181824,1.,0.974927912181824,
1.)))
REPRESENTATION_ITEM('')
SURFACE()
);
#371=(
BOUNDED_SURFACE()
B_SPLINE_SURFACE(3,2,((#25246,#25247,#25248,#25249,#25250,#25251,#25252,
#25253,#25254),(#25255,#25256,#25257,#25258,#25259,#25260,#25261,#25262,
#25263),(#25264,#25265,#25266,#25267,#25268,#25269,#25270,#25271,#25272),
(#25273,#25274,#25275,#25276,#25277,#25278,#25279,#25280,#25281)),
 .UNSPECIFIED.,.F.,.F.,.F.)
B_SPLINE_SURFACE_WITH_KNOTS((4,4),(3,2,2,2,3),(0.,1.),(0.,0.25,0.5,0.75,
1.),.UNSPECIFIED.)
GEOMETRIC_REPRESENTATION_ITEM()
RATIONAL_B_SPLINE_SURFACE(((1.,0.974927912181824,1.,0.974927912181824,1.,
0.974927912181824,1.,0.974927912181824,1.),(0.987189825241073,0.962438915249418,
0.987189825241073,0.962438915249418,0.987189825241073,0.962438915249418,
0.987189825241073,0.962438915249418,0.987189825241073),(0.987189825241073,
0.962438915249418,0.987189825241073,0.962438915249418,0.987189825241073,
0.962438915249418,0.987189825241073,0.962438915249418,0.987189825241073),
(1.,0.974927912181824,1.,0.974927912181824,1.,0.974927912181824,1.,0.974927912181824,
1.)))
REPRESENTATION_ITEM('')
SURFACE()
);
#372=(
BOUNDED_SURFACE()
B_SPLINE_SURFACE(3,2,((#25289,#25290,#25291,#25292,#25293,#25294,#25295,
#25296,#25297),(#25298,#25299,#25300,#25301,#25302,#25303,#25304,#25305,
#25306),(#25307,#25308,#25309,#25310,#25311,#25312,#25313,#25314,#25315),
(#25316,#25317,#25318,#25319,#25320,#25321,#25322,#25323,#25324)),
 .UNSPECIFIED.,.F.,.F.,.F.)
B_SPLINE_SURFACE_WITH_KNOTS((4,4),(3,2,2,2,3),(0.,1.),(0.,0.25,0.5,0.75,
1.),.UNSPECIFIED.)
GEOMETRIC_REPRESENTATION_ITEM()
RATIONAL_B_SPLINE_SURFACE(((1.,0.974927912181824,1.,0.974927912181824,1.,
0.974927912181824,1.,0.974927912181824,1.),(0.833333333333331,0.812439926818184,
0.833333333333331,0.812439926818184,0.833333333333331,0.812439926818184,
0.833333333333331,0.812439926818184,0.833333333333331),(0.833333333333331,
0.812439926818184,0.833333333333331,0.812439926818184,0.833333333333331,
0.812439926818184,0.833333333333331,0.812439926818184,0.833333333333331),
(1.,0.974927912181824,1.,0.974927912181824,1.,0.974927912181824,1.,0.974927912181824,
1.)))
REPRESENTATION_ITEM('')
SURFACE()
);
#373=(
BOUNDED_SURFACE()
B_SPLINE_SURFACE(3,2,((#25328,#25329,#25330,#25331,#25332,#25333,#25334,
#25335,#25336),(#25337,#25338,#25339,#25340,#25341,#25342,#25343,#25344,
#25345),(#25346,#25347,#25348,#25349,#25350,#25351,#25352,#25353,#25354),
(#25355,#25356,#25357,#25358,#25359,#25360,#25361,#25362,#25363)),
 .UNSPECIFIED.,.F.,.F.,.F.)
B_SPLINE_SURFACE_WITH_KNOTS((4,4),(3,2,2,2,3),(0.,1.),(0.,0.25,0.5,0.75,
1.),.UNSPECIFIED.)
GEOMETRIC_REPRESENTATION_ITEM()
RATIONAL_B_SPLINE_SURFACE(((1.,0.974927912181824,1.,0.974927912181824,1.,
0.974927912181824,1.,0.974927912181824,1.),(0.987189825241073,0.962438915249418,
0.987189825241073,0.962438915249418,0.987189825241073,0.962438915249418,
0.987189825241073,0.962438915249418,0.987189825241073),(0.987189825241073,
0.962438915249418,0.987189825241073,0.962438915249418,0.987189825241073,
0.962438915249418,0.987189825241073,0.962438915249418,0.987189825241073),
(1.,0.974927912181824,1.,0.974927912181824,1.,0.974927912181824,1.,0.974927912181824,
1.)))
REPRESENTATION_ITEM('')
SURFACE()
);
#374=(
BOUNDED_SURFACE()
B_SPLINE_SURFACE(3,2,((#25418,#25419,#25420,#25421,#25422,#25423,#25424,
#25425,#25426),(#25427,#25428,#25429,#25430,#25431,#25432,#25433,#25434,
#25435),(#25436,#25437,#25438,#25439,#25440,#25441,#25442,#25443,#25444),
(#25445,#25446,#25447,#25448,#25449,#25450,#25451,#25452,#25453)),
 .UNSPECIFIED.,.F.,.F.,.F.)
B_SPLINE_SURFACE_WITH_KNOTS((4,4),(3,2,2,2,3),(0.,1.),(0.,0.25,0.5,0.75,
1.),.UNSPECIFIED.)
GEOMETRIC_REPRESENTATION_ITEM()
RATIONAL_B_SPLINE_SURFACE(((1.,0.974927912181824,1.,0.974927912181824,1.,
0.974927912181824,1.,0.974927912181824,1.),(0.987189825241073,0.962438915249418,
0.987189825241073,0.962438915249418,0.987189825241073,0.962438915249418,
0.987189825241073,0.962438915249418,0.987189825241073),(0.987189825241073,
0.962438915249418,0.987189825241073,0.962438915249418,0.987189825241073,
0.962438915249418,0.987189825241073,0.962438915249418,0.987189825241073),
(1.,0.974927912181824,1.,0.974927912181824,1.,0.974927912181824,1.,0.974927912181824,
1.)))
REPRESENTATION_ITEM('')
SURFACE()
);
#375=(
BOUNDED_SURFACE()
B_SPLINE_SURFACE(3,2,((#25461,#25462,#25463,#25464,#25465,#25466,#25467,
#25468,#25469),(#25470,#25471,#25472,#25473,#25474,#25475,#25476,#25477,
#25478),(#25479,#25480,#25481,#25482,#25483,#25484,#25485,#25486,#25487),
(#25488,#25489,#25490,#25491,#25492,#25493,#25494,#25495,#25496)),
 .UNSPECIFIED.,.F.,.F.,.F.)
B_SPLINE_SURFACE_WITH_KNOTS((4,4),(3,2,2,2,3),(0.,1.),(0.,0.25,0.5,0.75,
1.),.UNSPECIFIED.)
GEOMETRIC_REPRESENTATION_ITEM()
RATIONAL_B_SPLINE_SURFACE(((1.,0.974927912181824,1.,0.974927912181824,1.,
0.974927912181824,1.,0.974927912181824,1.),(0.833333333333332,0.812439926818185,
0.833333333333332,0.812439926818185,0.833333333333332,0.812439926818185,
0.833333333333332,0.812439926818185,0.833333333333332),(0.833333333333332,
0.812439926818185,0.833333333333332,0.812439926818185,0.833333333333332,
0.812439926818185,0.833333333333332,0.812439926818185,0.833333333333332),
(1.,0.974927912181824,1.,0.974927912181824,1.,0.974927912181824,1.,0.974927912181824,
1.)))
REPRESENTATION_ITEM('')
SURFACE()
);
#376=(
BOUNDED_SURFACE()
B_SPLINE_SURFACE(3,2,((#25500,#25501,#25502,#25503,#25504,#25505,#25506,
#25507,#25508),(#25509,#25510,#25511,#25512,#25513,#25514,#25515,#25516,
#25517),(#25518,#25519,#25520,#25521,#25522,#25523,#25524,#25525,#25526),
(#25527,#25528,#25529,#25530,#25531,#25532,#25533,#25534,#25535)),
 .UNSPECIFIED.,.F.,.F.,.F.)
B_SPLINE_SURFACE_WITH_KNOTS((4,4),(3,2,2,2,3),(0.,1.),(0.,0.0714285714285714,
0.142857142857143,0.214285714285714,0.25),.UNSPECIFIED.)
GEOMETRIC_REPRESENTATION_ITEM()
RATIONAL_B_SPLINE_SURFACE(((1.,0.974927912181824,1.,0.974927912181824,1.,
0.974927912181824,1.,0.987463956090912,0.987463956090912),(0.987189825241073,
0.962438915249418,0.987189825241073,0.962438915249418,0.987189825241073,
0.962438915249418,0.987189825241073,0.974814370245245,0.974814370245245),
(0.987189825241073,0.962438915249418,0.987189825241073,0.962438915249418,
0.987189825241073,0.962438915249418,0.987189825241073,0.974814370245245,
0.974814370245245),(1.,0.974927912181824,1.,0.974927912181824,1.,0.974927912181824,
1.,0.987463956090912,0.987463956090912)))
REPRESENTATION_ITEM('')
SURFACE()
);
#377=(
BOUNDED_SURFACE()
B_SPLINE_SURFACE(3,2,((#25543,#25544,#25545,#25546,#25547,#25548,#25549,
#25550,#25551),(#25552,#25553,#25554,#25555,#25556,#25557,#25558,#25559,
#25560),(#25561,#25562,#25563,#25564,#25565,#25566,#25567,#25568,#25569),
(#25570,#25571,#25572,#25573,#25574,#25575,#25576,#25577,#25578)),
 .UNSPECIFIED.,.F.,.F.,.F.)
B_SPLINE_SURFACE_WITH_KNOTS((4,4),(3,2,2,2,3),(0.,1.),(0.,0.0714285714285714,
0.142857142857143,0.214285714285714,0.25),.UNSPECIFIED.)
GEOMETRIC_REPRESENTATION_ITEM()
RATIONAL_B_SPLINE_SURFACE(((1.,0.974927912181824,1.,0.974927912181824,1.,
0.974927912181824,1.,0.987463956090912,0.987463956090912),(0.987189825241073,
0.962438915249418,0.987189825241073,0.962438915249418,0.987189825241073,
0.962438915249418,0.987189825241073,0.974814370245245,0.974814370245246),
(0.987189825241073,0.962438915249418,0.987189825241073,0.962438915249418,
0.987189825241073,0.962438915249418,0.987189825241073,0.974814370245245,
0.974814370245246),(1.,0.974927912181824,1.,0.974927912181824,1.,0.974927912181824,
1.,0.987463956090912,0.987463956090912)))
REPRESENTATION_ITEM('')
SURFACE()
);
#378=(
BOUNDED_SURFACE()
B_SPLINE_SURFACE(3,2,((#25586,#25587,#25588,#25589,#25590,#25591,#25592,
#25593,#25594),(#25595,#25596,#25597,#25598,#25599,#25600,#25601,#25602,
#25603),(#25604,#25605,#25606,#25607,#25608,#25609,#25610,#25611,#25612),
(#25613,#25614,#25615,#25616,#25617,#25618,#25619,#25620,#25621)),
 .UNSPECIFIED.,.F.,.F.,.F.)
B_SPLINE_SURFACE_WITH_KNOTS((4,4),(3,2,2,2,3),(0.,1.),(0.,0.0714285714285714,
0.142857142857143,0.214285714285714,0.25),.UNSPECIFIED.)
GEOMETRIC_REPRESENTATION_ITEM()
RATIONAL_B_SPLINE_SURFACE(((1.,0.974927912181824,1.,0.974927912181824,1.,
0.974927912181824,1.,0.987463956090912,0.987463956090912),(0.83333333333333,
0.812439926818183,0.83333333333333,0.812439926818183,0.83333333333333,0.812439926818183,
0.83333333333333,0.822886630075756,0.822886630075757),(0.83333333333333,
0.812439926818183,0.83333333333333,0.812439926818183,0.83333333333333,0.812439926818183,
0.83333333333333,0.822886630075756,0.822886630075757),(1.,0.974927912181824,
1.,0.974927912181824,1.,0.974927912181824,1.,0.987463956090912,0.987463956090912)))
REPRESENTATION_ITEM('')
SURFACE()
);
#379=(
BOUNDED_SURFACE()
B_SPLINE_SURFACE(3,2,((#25625,#25626,#25627,#25628,#25629,#25630,#25631,
#25632,#25633),(#25634,#25635,#25636,#25637,#25638,#25639,#25640,#25641,
#25642),(#25643,#25644,#25645,#25646,#25647,#25648,#25649,#25650,#25651),
(#25652,#25653,#25654,#25655,#25656,#25657,#25658,#25659,#25660)),
 .UNSPECIFIED.,.F.,.F.,.F.)
B_SPLINE_SURFACE_WITH_KNOTS((4,4),(3,2,2,2,3),(0.,1.),(0.,0.25,0.5,0.75,
1.),.UNSPECIFIED.)
GEOMETRIC_REPRESENTATION_ITEM()
RATIONAL_B_SPLINE_SURFACE(((1.,0.974927912181824,1.,0.974927912181824,1.,
0.974927912181824,1.,0.974927912181824,1.),(0.987189825241073,0.962438915249418,
0.987189825241073,0.962438915249418,0.987189825241073,0.962438915249418,
0.987189825241073,0.962438915249418,0.987189825241073),(0.987189825241073,
0.962438915249418,0.987189825241073,0.962438915249418,0.987189825241073,
0.962438915249418,0.987189825241073,0.962438915249418,0.987189825241073),
(1.,0.974927912181824,1.,0.974927912181824,1.,0.974927912181824,1.,0.974927912181824,
1.)))
REPRESENTATION_ITEM('')
SURFACE()
);
#380=(
BOUNDED_SURFACE()
B_SPLINE_SURFACE(3,2,((#25715,#25716,#25717,#25718,#25719,#25720,#25721,
#25722,#25723),(#25724,#25725,#25726,#25727,#25728,#25729,#25730,#25731,
#25732),(#25733,#25734,#25735,#25736,#25737,#25738,#25739,#25740,#25741),
(#25742,#25743,#25744,#25745,#25746,#25747,#25748,#25749,#25750)),
 .UNSPECIFIED.,.F.,.F.,.F.)
B_SPLINE_SURFACE_WITH_KNOTS((4,4),(3,2,2,2,3),(0.,1.),(0.,0.25,0.5,0.75,
1.),.UNSPECIFIED.)
GEOMETRIC_REPRESENTATION_ITEM()
RATIONAL_B_SPLINE_SURFACE(((1.,0.974927912181824,1.,0.974927912181824,1.,
0.974927912181824,1.,0.974927912181824,1.),(0.987189825241073,0.962438915249418,
0.987189825241073,0.962438915249418,0.987189825241073,0.962438915249418,
0.987189825241073,0.962438915249418,0.987189825241073),(0.987189825241073,
0.962438915249418,0.987189825241073,0.962438915249418,0.987189825241073,
0.962438915249418,0.987189825241073,0.962438915249418,0.987189825241073),
(1.,0.974927912181824,1.,0.974927912181824,1.,0.974927912181824,1.,0.974927912181824,
1.)))
REPRESENTATION_ITEM('')
SURFACE()
);
#381=(
BOUNDED_SURFACE()
B_SPLINE_SURFACE(3,2,((#25758,#25759,#25760,#25761,#25762,#25763,#25764,
#25765,#25766),(#25767,#25768,#25769,#25770,#25771,#25772,#25773,#25774,
#25775),(#25776,#25777,#25778,#25779,#25780,#25781,#25782,#25783,#25784),
(#25785,#25786,#25787,#25788,#25789,#25790,#25791,#25792,#25793)),
 .UNSPECIFIED.,.F.,.F.,.F.)
B_SPLINE_SURFACE_WITH_KNOTS((4,4),(3,2,2,2,3),(0.,1.),(0.,0.25,0.5,0.75,
1.),.UNSPECIFIED.)
GEOMETRIC_REPRESENTATION_ITEM()
RATIONAL_B_SPLINE_SURFACE(((1.,0.974927912181824,1.,0.974927912181824,1.,
0.974927912181824,1.,0.974927912181824,1.),(0.833333333333333,0.812439926818186,
0.833333333333333,0.812439926818186,0.833333333333333,0.812439926818186,
0.833333333333333,0.812439926818186,0.833333333333333),(0.833333333333333,
0.812439926818186,0.833333333333333,0.812439926818186,0.833333333333333,
0.812439926818186,0.833333333333333,0.812439926818186,0.833333333333333),
(1.,0.974927912181824,1.,0.974927912181824,1.,0.974927912181824,1.,0.974927912181824,
1.)))
REPRESENTATION_ITEM('')
SURFACE()
);
#382=(
BOUNDED_SURFACE()
B_SPLINE_SURFACE(3,2,((#25797,#25798,#25799,#25800,#25801,#25802,#25803,
#25804,#25805),(#25806,#25807,#25808,#25809,#25810,#25811,#25812,#25813,
#25814),(#25815,#25816,#25817,#25818,#25819,#25820,#25821,#25822,#25823),
(#25824,#25825,#25826,#25827,#25828,#25829,#25830,#25831,#25832)),
 .UNSPECIFIED.,.F.,.F.,.F.)
B_SPLINE_SURFACE_WITH_KNOTS((4,4),(3,2,2,2,3),(0.,1.),(0.,0.25,0.5,0.75,
1.),.UNSPECIFIED.)
GEOMETRIC_REPRESENTATION_ITEM()
RATIONAL_B_SPLINE_SURFACE(((1.,0.974927912181824,1.,0.974927912181824,1.,
0.974927912181824,1.,0.974927912181824,1.),(0.987189825241073,0.962438915249418,
0.987189825241073,0.962438915249418,0.987189825241073,0.962438915249418,
0.987189825241073,0.962438915249418,0.987189825241073),(0.987189825241073,
0.962438915249418,0.987189825241073,0.962438915249418,0.987189825241073,
0.962438915249418,0.987189825241073,0.962438915249418,0.987189825241073),
(1.,0.974927912181824,1.,0.974927912181824,1.,0.974927912181824,1.,0.974927912181824,
1.)))
REPRESENTATION_ITEM('')
SURFACE()
);
#383=(
BOUNDED_SURFACE()
B_SPLINE_SURFACE(3,2,((#25887,#25888,#25889,#25890,#25891,#25892,#25893,
#25894,#25895),(#25896,#25897,#25898,#25899,#25900,#25901,#25902,#25903,
#25904),(#25905,#25906,#25907,#25908,#25909,#25910,#25911,#25912,#25913),
(#25914,#25915,#25916,#25917,#25918,#25919,#25920,#25921,#25922)),
 .UNSPECIFIED.,.F.,.F.,.F.)
B_SPLINE_SURFACE_WITH_KNOTS((4,4),(3,2,2,2,3),(0.,1.),(0.,0.25,0.5,0.75,
1.),.UNSPECIFIED.)
GEOMETRIC_REPRESENTATION_ITEM()
RATIONAL_B_SPLINE_SURFACE(((1.,0.974927912181824,1.,0.974927912181824,1.,
0.974927912181824,1.,0.974927912181824,1.),(0.987189825241073,0.962438915249418,
0.987189825241073,0.962438915249418,0.987189825241073,0.962438915249418,
0.987189825241073,0.962438915249418,0.987189825241073),(0.987189825241073,
0.962438915249418,0.987189825241073,0.962438915249418,0.987189825241073,
0.962438915249418,0.987189825241073,0.962438915249418,0.987189825241073),
(1.,0.974927912181824,1.,0.974927912181824,1.,0.974927912181824,1.,0.974927912181824,
1.)))
REPRESENTATION_ITEM('')
SURFACE()
);
#384=(
BOUNDED_SURFACE()
B_SPLINE_SURFACE(3,2,((#25930,#25931,#25932,#25933,#25934,#25935,#25936,
#25937,#25938),(#25939,#25940,#25941,#25942,#25943,#25944,#25945,#25946,
#25947),(#25948,#25949,#25950,#25951,#25952,#25953,#25954,#25955,#25956),
(#25957,#25958,#25959,#25960,#25961,#25962,#25963,#25964,#25965)),
 .UNSPECIFIED.,.F.,.F.,.F.)
B_SPLINE_SURFACE_WITH_KNOTS((4,4),(3,2,2,2,3),(0.,1.),(0.,0.25,0.5,0.75,
1.),.UNSPECIFIED.)
GEOMETRIC_REPRESENTATION_ITEM()
RATIONAL_B_SPLINE_SURFACE(((1.,0.974927912181824,1.,0.974927912181824,1.,
0.974927912181824,1.,0.974927912181824,1.),(0.833333333333333,0.812439926818186,
0.833333333333333,0.812439926818186,0.833333333333333,0.812439926818186,
0.833333333333333,0.812439926818186,0.833333333333333),(0.833333333333333,
0.812439926818186,0.833333333333333,0.812439926818186,0.833333333333333,
0.812439926818186,0.833333333333333,0.812439926818186,0.833333333333333),
(1.,0.974927912181824,1.,0.974927912181824,1.,0.974927912181824,1.,0.974927912181824,
1.)))
REPRESENTATION_ITEM('')
SURFACE()
);
#385=(
BOUNDED_SURFACE()
B_SPLINE_SURFACE(3,2,((#25969,#25970,#25971,#25972,#25973,#25974,#25975,
#25976,#25977),(#25978,#25979,#25980,#25981,#25982,#25983,#25984,#25985,
#25986),(#25987,#25988,#25989,#25990,#25991,#25992,#25993,#25994,#25995),
(#25996,#25997,#25998,#25999,#26000,#26001,#26002,#26003,#26004)),
 .UNSPECIFIED.,.F.,.F.,.F.)
B_SPLINE_SURFACE_WITH_KNOTS((4,4),(3,2,2,2,3),(0.,1.),(0.,0.25,0.5,0.75,
1.),.UNSPECIFIED.)
GEOMETRIC_REPRESENTATION_ITEM()
RATIONAL_B_SPLINE_SURFACE(((1.,0.974927912181824,1.,0.974927912181824,1.,
0.974927912181824,1.,0.974927912181824,1.),(0.987189825241073,0.962438915249418,
0.987189825241073,0.962438915249418,0.987189825241073,0.962438915249418,
0.987189825241073,0.962438915249418,0.987189825241073),(0.987189825241073,
0.962438915249418,0.987189825241073,0.962438915249418,0.987189825241073,
0.962438915249418,0.987189825241073,0.962438915249418,0.987189825241073),
(1.,0.974927912181824,1.,0.974927912181824,1.,0.974927912181824,1.,0.974927912181824,
1.)))
REPRESENTATION_ITEM('')
SURFACE()
);
#386=(
BOUNDED_SURFACE()
B_SPLINE_SURFACE(3,2,((#26059,#26060,#26061,#26062,#26063,#26064,#26065,
#26066,#26067),(#26068,#26069,#26070,#26071,#26072,#26073,#26074,#26075,
#26076),(#26077,#26078,#26079,#26080,#26081,#26082,#26083,#26084,#26085),
(#26086,#26087,#26088,#26089,#26090,#26091,#26092,#26093,#26094)),
 .UNSPECIFIED.,.F.,.F.,.F.)
B_SPLINE_SURFACE_WITH_KNOTS((4,4),(3,2,2,2,3),(0.,1.),(0.,0.25,0.5,0.75,
1.),.UNSPECIFIED.)
GEOMETRIC_REPRESENTATION_ITEM()
RATIONAL_B_SPLINE_SURFACE(((1.,0.974927912181824,1.,0.974927912181824,1.,
0.974927912181824,1.,0.974927912181824,1.),(0.987189825241073,0.962438915249418,
0.987189825241073,0.962438915249418,0.987189825241073,0.962438915249418,
0.987189825241073,0.962438915249418,0.987189825241073),(0.987189825241073,
0.962438915249418,0.987189825241073,0.962438915249418,0.987189825241073,
0.962438915249418,0.987189825241073,0.962438915249418,0.987189825241073),
(1.,0.974927912181824,1.,0.974927912181824,1.,0.974927912181824,1.,0.974927912181824,
1.)))
REPRESENTATION_ITEM('')
SURFACE()
);
#387=(
BOUNDED_SURFACE()
B_SPLINE_SURFACE(3,2,((#26102,#26103,#26104,#26105,#26106,#26107,#26108,
#26109,#26110),(#26111,#26112,#26113,#26114,#26115,#26116,#26117,#26118,
#26119),(#26120,#26121,#26122,#26123,#26124,#26125,#26126,#26127,#26128),
(#26129,#26130,#26131,#26132,#26133,#26134,#26135,#26136,#26137)),
 .UNSPECIFIED.,.F.,.F.,.F.)
B_SPLINE_SURFACE_WITH_KNOTS((4,4),(3,2,2,2,3),(0.,1.),(0.,0.25,0.5,0.75,
1.),.UNSPECIFIED.)
GEOMETRIC_REPRESENTATION_ITEM()
RATIONAL_B_SPLINE_SURFACE(((1.,0.974927912181824,1.,0.974927912181824,1.,
0.974927912181824,1.,0.974927912181824,1.),(0.833333333333332,0.812439926818185,
0.833333333333332,0.812439926818185,0.833333333333332,0.812439926818185,
0.833333333333332,0.812439926818185,0.833333333333332),(0.833333333333332,
0.812439926818185,0.833333333333332,0.812439926818185,0.833333333333332,
0.812439926818185,0.833333333333332,0.812439926818185,0.833333333333332),
(1.,0.974927912181824,1.,0.974927912181824,1.,0.974927912181824,1.,0.974927912181824,
1.)))
REPRESENTATION_ITEM('')
SURFACE()
);
#388=(
BOUNDED_SURFACE()
B_SPLINE_SURFACE(3,2,((#26141,#26142,#26143,#26144,#26145,#26146,#26147,
#26148,#26149),(#26150,#26151,#26152,#26153,#26154,#26155,#26156,#26157,
#26158),(#26159,#26160,#26161,#26162,#26163,#26164,#26165,#26166,#26167),
(#26168,#26169,#26170,#26171,#26172,#26173,#26174,#26175,#26176)),
 .UNSPECIFIED.,.F.,.F.,.F.)
B_SPLINE_SURFACE_WITH_KNOTS((4,4),(3,2,2,2,3),(0.,1.),(0.,0.25,0.5,0.75,
1.),.UNSPECIFIED.)
GEOMETRIC_REPRESENTATION_ITEM()
RATIONAL_B_SPLINE_SURFACE(((1.,0.974927912181824,1.,0.974927912181824,1.,
0.974927912181824,1.,0.974927912181824,1.),(0.987189825241073,0.962438915249418,
0.987189825241073,0.962438915249418,0.987189825241073,0.962438915249418,
0.987189825241073,0.962438915249418,0.987189825241073),(0.987189825241073,
0.962438915249418,0.987189825241073,0.962438915249418,0.987189825241073,
0.962438915249418,0.987189825241073,0.962438915249418,0.987189825241073),
(1.,0.974927912181824,1.,0.974927912181824,1.,0.974927912181824,1.,0.974927912181824,
1.)))
REPRESENTATION_ITEM('')
SURFACE()
);
#389=(
BOUNDED_SURFACE()
B_SPLINE_SURFACE(3,2,((#26231,#26232,#26233,#26234,#26235,#26236,#26237,
#26238,#26239),(#26240,#26241,#26242,#26243,#26244,#26245,#26246,#26247,
#26248),(#26249,#26250,#26251,#26252,#26253,#26254,#26255,#26256,#26257),
(#26258,#26259,#26260,#26261,#26262,#26263,#26264,#26265,#26266)),
 .UNSPECIFIED.,.F.,.F.,.F.)
B_SPLINE_SURFACE_WITH_KNOTS((4,4),(3,2,2,2,3),(0.,1.),(0.,0.25,0.5,0.75,
1.),.UNSPECIFIED.)
GEOMETRIC_REPRESENTATION_ITEM()
RATIONAL_B_SPLINE_SURFACE(((1.,0.974927912181824,1.,0.974927912181824,1.,
0.974927912181824,1.,0.974927912181824,1.),(0.987189825241073,0.962438915249418,
0.987189825241073,0.962438915249418,0.987189825241073,0.962438915249418,
0.987189825241073,0.962438915249418,0.987189825241073),(0.987189825241073,
0.962438915249418,0.987189825241073,0.962438915249418,0.987189825241073,
0.962438915249418,0.987189825241073,0.962438915249418,0.987189825241073),
(1.,0.974927912181824,1.,0.974927912181824,1.,0.974927912181824,1.,0.974927912181824,
1.)))
REPRESENTATION_ITEM('')
SURFACE()
);
#390=(
BOUNDED_SURFACE()
B_SPLINE_SURFACE(3,2,((#26274,#26275,#26276,#26277,#26278,#26279,#26280,
#26281,#26282),(#26283,#26284,#26285,#26286,#26287,#26288,#26289,#26290,
#26291),(#26292,#26293,#26294,#26295,#26296,#26297,#26298,#26299,#26300),
(#26301,#26302,#26303,#26304,#26305,#26306,#26307,#26308,#26309)),
 .UNSPECIFIED.,.F.,.F.,.F.)
B_SPLINE_SURFACE_WITH_KNOTS((4,4),(3,2,2,2,3),(0.,1.),(0.,0.25,0.5,0.75,
1.),.UNSPECIFIED.)
GEOMETRIC_REPRESENTATION_ITEM()
RATIONAL_B_SPLINE_SURFACE(((1.,0.974927912181824,1.,0.974927912181824,1.,
0.974927912181824,1.,0.974927912181824,1.),(0.833333333333333,0.812439926818186,
0.833333333333333,0.812439926818186,0.833333333333333,0.812439926818186,
0.833333333333333,0.812439926818186,0.833333333333333),(0.833333333333333,
0.812439926818186,0.833333333333333,0.812439926818186,0.833333333333333,
0.812439926818186,0.833333333333333,0.812439926818186,0.833333333333333),
(1.,0.974927912181824,1.,0.974927912181824,1.,0.974927912181824,1.,0.974927912181824,
1.)))
REPRESENTATION_ITEM('')
SURFACE()
);
#391=(
BOUNDED_SURFACE()
B_SPLINE_SURFACE(3,2,((#26313,#26314,#26315,#26316,#26317,#26318,#26319,
#26320,#26321),(#26322,#26323,#26324,#26325,#26326,#26327,#26328,#26329,
#26330),(#26331,#26332,#26333,#26334,#26335,#26336,#26337,#26338,#26339),
(#26340,#26341,#26342,#26343,#26344,#26345,#26346,#26347,#26348)),
 .UNSPECIFIED.,.F.,.F.,.F.)
B_SPLINE_SURFACE_WITH_KNOTS((4,4),(3,2,2,2,3),(0.,1.),(0.,0.25,0.5,0.75,
1.),.UNSPECIFIED.)
GEOMETRIC_REPRESENTATION_ITEM()
RATIONAL_B_SPLINE_SURFACE(((1.,0.974927912181824,1.,0.974927912181824,1.,
0.974927912181824,1.,0.974927912181824,1.),(0.987189825241073,0.962438915249418,
0.987189825241073,0.962438915249418,0.987189825241073,0.962438915249418,
0.987189825241073,0.962438915249418,0.987189825241073),(0.987189825241073,
0.962438915249418,0.987189825241073,0.962438915249418,0.987189825241073,
0.962438915249418,0.987189825241073,0.962438915249418,0.987189825241073),
(1.,0.974927912181824,1.,0.974927912181824,1.,0.974927912181824,1.,0.974927912181824,
1.)))
REPRESENTATION_ITEM('')
SURFACE()
);
#392=(
BOUNDED_SURFACE()
B_SPLINE_SURFACE(3,2,((#26403,#26404,#26405,#26406,#26407,#26408,#26409,
#26410,#26411),(#26412,#26413,#26414,#26415,#26416,#26417,#26418,#26419,
#26420),(#26421,#26422,#26423,#26424,#26425,#26426,#26427,#26428,#26429),
(#26430,#26431,#26432,#26433,#26434,#26435,#26436,#26437,#26438)),
 .UNSPECIFIED.,.F.,.F.,.F.)
B_SPLINE_SURFACE_WITH_KNOTS((4,4),(3,2,2,2,3),(0.,1.),(0.,0.25,0.5,0.75,
1.),.UNSPECIFIED.)
GEOMETRIC_REPRESENTATION_ITEM()
RATIONAL_B_SPLINE_SURFACE(((1.,0.974927912181824,1.,0.974927912181824,1.,
0.974927912181824,1.,0.974927912181824,1.),(0.987189825241073,0.962438915249418,
0.987189825241073,0.962438915249418,0.987189825241073,0.962438915249418,
0.987189825241073,0.962438915249418,0.987189825241073),(0.987189825241073,
0.962438915249418,0.987189825241073,0.962438915249418,0.987189825241073,
0.962438915249418,0.987189825241073,0.962438915249418,0.987189825241073),
(1.,0.974927912181824,1.,0.974927912181824,1.,0.974927912181824,1.,0.974927912181824,
1.)))
REPRESENTATION_ITEM('')
SURFACE()
);
#393=(
BOUNDED_SURFACE()
B_SPLINE_SURFACE(3,2,((#26446,#26447,#26448,#26449,#26450,#26451,#26452,
#26453,#26454),(#26455,#26456,#26457,#26458,#26459,#26460,#26461,#26462,
#26463),(#26464,#26465,#26466,#26467,#26468,#26469,#26470,#26471,#26472),
(#26473,#26474,#26475,#26476,#26477,#26478,#26479,#26480,#26481)),
 .UNSPECIFIED.,.F.,.F.,.F.)
B_SPLINE_SURFACE_WITH_KNOTS((4,4),(3,2,2,2,3),(0.,1.),(0.,0.25,0.5,0.75,
1.),.UNSPECIFIED.)
GEOMETRIC_REPRESENTATION_ITEM()
RATIONAL_B_SPLINE_SURFACE(((1.,0.974927912181824,1.,0.974927912181824,1.,
0.974927912181824,1.,0.974927912181824,1.),(0.833333333333332,0.812439926818185,
0.833333333333332,0.812439926818185,0.833333333333332,0.812439926818185,
0.833333333333332,0.812439926818185,0.833333333333332),(0.833333333333332,
0.812439926818185,0.833333333333332,0.812439926818185,0.833333333333332,
0.812439926818185,0.833333333333332,0.812439926818185,0.833333333333332),
(1.,0.974927912181824,1.,0.974927912181824,1.,0.974927912181824,1.,0.974927912181824,
1.)))
REPRESENTATION_ITEM('')
SURFACE()
);
#394=(
BOUNDED_SURFACE()
B_SPLINE_SURFACE(3,2,((#26485,#26486,#26487,#26488,#26489,#26490,#26491,
#26492,#26493),(#26494,#26495,#26496,#26497,#26498,#26499,#26500,#26501,
#26502),(#26503,#26504,#26505,#26506,#26507,#26508,#26509,#26510,#26511),
(#26512,#26513,#26514,#26515,#26516,#26517,#26518,#26519,#26520)),
 .UNSPECIFIED.,.F.,.F.,.F.)
B_SPLINE_SURFACE_WITH_KNOTS((4,4),(3,2,2,2,3),(0.,1.),(0.,0.25,0.5,0.75,
1.),.UNSPECIFIED.)
GEOMETRIC_REPRESENTATION_ITEM()
RATIONAL_B_SPLINE_SURFACE(((1.,0.974927912181824,1.,0.974927912181824,1.,
0.974927912181824,1.,0.974927912181824,1.),(0.987189825241073,0.962438915249418,
0.987189825241073,0.962438915249418,0.987189825241073,0.962438915249418,
0.987189825241073,0.962438915249418,0.987189825241073),(0.987189825241073,
0.962438915249418,0.987189825241073,0.962438915249418,0.987189825241073,
0.962438915249418,0.987189825241073,0.962438915249418,0.987189825241073),
(1.,0.974927912181824,1.,0.974927912181824,1.,0.974927912181824,1.,0.974927912181824,
1.)))
REPRESENTATION_ITEM('')
SURFACE()
);
#395=(
BOUNDED_SURFACE()
B_SPLINE_SURFACE(3,2,((#26575,#26576,#26577,#26578,#26579,#26580,#26581,
#26582,#26583),(#26584,#26585,#26586,#26587,#26588,#26589,#26590,#26591,
#26592),(#26593,#26594,#26595,#26596,#26597,#26598,#26599,#26600,#26601),
(#26602,#26603,#26604,#26605,#26606,#26607,#26608,#26609,#26610)),
 .UNSPECIFIED.,.F.,.F.,.F.)
B_SPLINE_SURFACE_WITH_KNOTS((4,4),(3,2,2,2,3),(0.,1.),(0.,0.25,0.5,0.75,
1.),.UNSPECIFIED.)
GEOMETRIC_REPRESENTATION_ITEM()
RATIONAL_B_SPLINE_SURFACE(((1.,0.974927912181824,1.,0.974927912181824,1.,
0.974927912181824,1.,0.974927912181824,1.),(0.987189825241073,0.962438915249418,
0.987189825241073,0.962438915249418,0.987189825241073,0.962438915249418,
0.987189825241073,0.962438915249418,0.987189825241073),(0.987189825241073,
0.962438915249418,0.987189825241073,0.962438915249418,0.987189825241073,
0.962438915249418,0.987189825241073,0.962438915249418,0.987189825241073),
(1.,0.974927912181824,1.,0.974927912181824,1.,0.974927912181824,1.,0.974927912181824,
1.)))
REPRESENTATION_ITEM('')
SURFACE()
);
#396=(
BOUNDED_SURFACE()
B_SPLINE_SURFACE(3,2,((#26618,#26619,#26620,#26621,#26622,#26623,#26624,
#26625,#26626),(#26627,#26628,#26629,#26630,#26631,#26632,#26633,#26634,
#26635),(#26636,#26637,#26638,#26639,#26640,#26641,#26642,#26643,#26644),
(#26645,#26646,#26647,#26648,#26649,#26650,#26651,#26652,#26653)),
 .UNSPECIFIED.,.F.,.F.,.F.)
B_SPLINE_SURFACE_WITH_KNOTS((4,4),(3,2,2,2,3),(0.,1.),(0.,0.25,0.5,0.75,
1.),.UNSPECIFIED.)
GEOMETRIC_REPRESENTATION_ITEM()
RATIONAL_B_SPLINE_SURFACE(((1.,0.974927912181824,1.,0.974927912181824,1.,
0.974927912181824,1.,0.974927912181824,1.),(0.833333333333333,0.812439926818186,
0.833333333333333,0.812439926818186,0.833333333333333,0.812439926818186,
0.833333333333333,0.812439926818186,0.833333333333333),(0.833333333333333,
0.812439926818186,0.833333333333333,0.812439926818186,0.833333333333333,
0.812439926818186,0.833333333333333,0.812439926818186,0.833333333333333),
(1.,0.974927912181824,1.,0.974927912181824,1.,0.974927912181824,1.,0.974927912181824,
1.)))
REPRESENTATION_ITEM('')
SURFACE()
);
#397=(
BOUNDED_SURFACE()
B_SPLINE_SURFACE(3,2,((#26657,#26658,#26659,#26660,#26661,#26662,#26663,
#26664,#26665),(#26666,#26667,#26668,#26669,#26670,#26671,#26672,#26673,
#26674),(#26675,#26676,#26677,#26678,#26679,#26680,#26681,#26682,#26683),
(#26684,#26685,#26686,#26687,#26688,#26689,#26690,#26691,#26692)),
 .UNSPECIFIED.,.F.,.F.,.F.)
B_SPLINE_SURFACE_WITH_KNOTS((4,4),(3,2,2,2,3),(0.,1.),(0.,0.25,0.5,0.75,
1.),.UNSPECIFIED.)
GEOMETRIC_REPRESENTATION_ITEM()
RATIONAL_B_SPLINE_SURFACE(((1.,0.974927912181824,1.,0.974927912181824,1.,
0.974927912181824,1.,0.974927912181824,1.),(0.987189825241073,0.962438915249418,
0.987189825241073,0.962438915249418,0.987189825241073,0.962438915249418,
0.987189825241073,0.962438915249418,0.987189825241073),(0.987189825241073,
0.962438915249418,0.987189825241073,0.962438915249418,0.987189825241073,
0.962438915249418,0.987189825241073,0.962438915249418,0.987189825241073),
(1.,0.974927912181824,1.,0.974927912181824,1.,0.974927912181824,1.,0.974927912181824,
1.)))
REPRESENTATION_ITEM('')
SURFACE()
);
#398=(
BOUNDED_SURFACE()
B_SPLINE_SURFACE(3,2,((#26747,#26748,#26749,#26750,#26751,#26752,#26753,
#26754,#26755),(#26756,#26757,#26758,#26759,#26760,#26761,#26762,#26763,
#26764),(#26765,#26766,#26767,#26768,#26769,#26770,#26771,#26772,#26773),
(#26774,#26775,#26776,#26777,#26778,#26779,#26780,#26781,#26782)),
 .UNSPECIFIED.,.F.,.F.,.F.)
B_SPLINE_SURFACE_WITH_KNOTS((4,4),(3,2,2,2,3),(0.,1.),(0.,0.25,0.5,0.75,
1.),.UNSPECIFIED.)
GEOMETRIC_REPRESENTATION_ITEM()
RATIONAL_B_SPLINE_SURFACE(((1.,0.974927912181824,1.,0.974927912181824,1.,
0.974927912181824,1.,0.974927912181824,1.),(0.987189825241073,0.962438915249418,
0.987189825241073,0.962438915249418,0.987189825241073,0.962438915249418,
0.987189825241073,0.962438915249418,0.987189825241073),(0.987189825241073,
0.962438915249418,0.987189825241073,0.962438915249418,0.987189825241073,
0.962438915249418,0.987189825241073,0.962438915249418,0.987189825241073),
(1.,0.974927912181824,1.,0.974927912181824,1.,0.974927912181824,1.,0.974927912181824,
1.)))
REPRESENTATION_ITEM('')
SURFACE()
);
#399=(
BOUNDED_SURFACE()
B_SPLINE_SURFACE(3,2,((#26790,#26791,#26792,#26793,#26794,#26795,#26796,
#26797,#26798),(#26799,#26800,#26801,#26802,#26803,#26804,#26805,#26806,
#26807),(#26808,#26809,#26810,#26811,#26812,#26813,#26814,#26815,#26816),
(#26817,#26818,#26819,#26820,#26821,#26822,#26823,#26824,#26825)),
 .UNSPECIFIED.,.F.,.F.,.F.)
B_SPLINE_SURFACE_WITH_KNOTS((4,4),(3,2,2,2,3),(0.,1.),(0.,0.25,0.5,0.75,
1.),.UNSPECIFIED.)
GEOMETRIC_REPRESENTATION_ITEM()
RATIONAL_B_SPLINE_SURFACE(((1.,0.974927912181824,1.,0.974927912181824,1.,
0.974927912181824,1.,0.974927912181824,1.),(0.833333333333332,0.812439926818185,
0.833333333333332,0.812439926818185,0.833333333333332,0.812439926818185,
0.833333333333332,0.812439926818185,0.833333333333332),(0.833333333333332,
0.812439926818185,0.833333333333332,0.812439926818185,0.833333333333332,
0.812439926818185,0.833333333333332,0.812439926818185,0.833333333333332),
(1.,0.974927912181824,1.,0.974927912181824,1.,0.974927912181824,1.,0.974927912181824,
1.)))
REPRESENTATION_ITEM('')
SURFACE()
);
#400=(
BOUNDED_SURFACE()
B_SPLINE_SURFACE(3,2,((#26829,#26830,#26831,#26832,#26833,#26834,#26835,
#26836,#26837),(#26838,#26839,#26840,#26841,#26842,#26843,#26844,#26845,
#26846),(#26847,#26848,#26849,#26850,#26851,#26852,#26853,#26854,#26855),
(#26856,#26857,#26858,#26859,#26860,#26861,#26862,#26863,#26864)),
 .UNSPECIFIED.,.F.,.F.,.F.)
B_SPLINE_SURFACE_WITH_KNOTS((4,4),(3,2,2,2,3),(0.,1.),(0.,0.25,0.5,0.75,
1.),.UNSPECIFIED.)
GEOMETRIC_REPRESENTATION_ITEM()
RATIONAL_B_SPLINE_SURFACE(((1.,0.974927912181824,1.,0.974927912181824,1.,
0.974927912181824,1.,0.974927912181824,1.),(0.987189825241073,0.962438915249418,
0.987189825241073,0.962438915249418,0.987189825241073,0.962438915249418,
0.987189825241073,0.962438915249418,0.987189825241073),(0.987189825241073,
0.962438915249418,0.987189825241073,0.962438915249418,0.987189825241073,
0.962438915249418,0.987189825241073,0.962438915249418,0.987189825241073),
(1.,0.974927912181824,1.,0.974927912181824,1.,0.974927912181824,1.,0.974927912181824,
1.)))
REPRESENTATION_ITEM('')
SURFACE()
);
#401=(
BOUNDED_SURFACE()
B_SPLINE_SURFACE(3,2,((#26919,#26920,#26921,#26922,#26923,#26924,#26925,
#26926,#26927),(#26928,#26929,#26930,#26931,#26932,#26933,#26934,#26935,
#26936),(#26937,#26938,#26939,#26940,#26941,#26942,#26943,#26944,#26945),
(#26946,#26947,#26948,#26949,#26950,#26951,#26952,#26953,#26954)),
 .UNSPECIFIED.,.F.,.F.,.F.)
B_SPLINE_SURFACE_WITH_KNOTS((4,4),(3,2,2,2,3),(0.,1.),(0.,0.25,0.5,0.75,
1.),.UNSPECIFIED.)
GEOMETRIC_REPRESENTATION_ITEM()
RATIONAL_B_SPLINE_SURFACE(((1.,0.974927912181824,1.,0.974927912181824,1.,
0.974927912181824,1.,0.974927912181824,1.),(0.987189825241073,0.962438915249418,
0.987189825241073,0.962438915249418,0.987189825241073,0.962438915249418,
0.987189825241073,0.962438915249418,0.987189825241073),(0.987189825241073,
0.962438915249418,0.987189825241073,0.962438915249418,0.987189825241073,
0.962438915249418,0.987189825241073,0.962438915249418,0.987189825241073),
(1.,0.974927912181824,1.,0.974927912181824,1.,0.974927912181824,1.,0.974927912181824,
1.)))
REPRESENTATION_ITEM('')
SURFACE()
);
#402=(
BOUNDED_SURFACE()
B_SPLINE_SURFACE(3,2,((#26962,#26963,#26964,#26965,#26966,#26967,#26968,
#26969,#26970),(#26971,#26972,#26973,#26974,#26975,#26976,#26977,#26978,
#26979),(#26980,#26981,#26982,#26983,#26984,#26985,#26986,#26987,#26988),
(#26989,#26990,#26991,#26992,#26993,#26994,#26995,#26996,#26997)),
 .UNSPECIFIED.,.F.,.F.,.F.)
B_SPLINE_SURFACE_WITH_KNOTS((4,4),(3,2,2,2,3),(0.,1.),(0.,0.25,0.5,0.75,
1.),.UNSPECIFIED.)
GEOMETRIC_REPRESENTATION_ITEM()
RATIONAL_B_SPLINE_SURFACE(((1.,0.974927912181824,1.,0.974927912181824,1.,
0.974927912181824,1.,0.974927912181824,1.),(0.833333333333332,0.812439926818185,
0.833333333333332,0.812439926818185,0.833333333333332,0.812439926818185,
0.833333333333332,0.812439926818185,0.833333333333332),(0.833333333333332,
0.812439926818185,0.833333333333332,0.812439926818185,0.833333333333332,
0.812439926818185,0.833333333333332,0.812439926818185,0.833333333333332),
(1.,0.974927912181824,1.,0.974927912181824,1.,0.974927912181824,1.,0.974927912181824,
1.)))
REPRESENTATION_ITEM('')
SURFACE()
);
#403=(
BOUNDED_SURFACE()
B_SPLINE_SURFACE(3,2,((#27001,#27002,#27003,#27004,#27005,#27006,#27007,
#27008,#27009),(#27010,#27011,#27012,#27013,#27014,#27015,#27016,#27017,
#27018),(#27019,#27020,#27021,#27022,#27023,#27024,#27025,#27026,#27027),
(#27028,#27029,#27030,#27031,#27032,#27033,#27034,#27035,#27036)),
 .UNSPECIFIED.,.F.,.F.,.F.)
B_SPLINE_SURFACE_WITH_KNOTS((4,4),(3,2,2,2,3),(0.,1.),(0.,0.25,0.5,0.75,
1.),.UNSPECIFIED.)
GEOMETRIC_REPRESENTATION_ITEM()
RATIONAL_B_SPLINE_SURFACE(((1.,0.974927912181824,1.,0.974927912181824,1.,
0.974927912181824,1.,0.974927912181824,1.),(0.987189825241073,0.962438915249418,
0.987189825241073,0.962438915249418,0.987189825241073,0.962438915249418,
0.987189825241073,0.962438915249418,0.987189825241073),(0.987189825241073,
0.962438915249418,0.987189825241073,0.962438915249418,0.987189825241073,
0.962438915249418,0.987189825241073,0.962438915249418,0.987189825241073),
(1.,0.974927912181824,1.,0.974927912181824,1.,0.974927912181824,1.,0.974927912181824,
1.)))
REPRESENTATION_ITEM('')
SURFACE()
);
#404=(
BOUNDED_SURFACE()
B_SPLINE_SURFACE(3,2,((#27091,#27092,#27093,#27094,#27095,#27096,#27097,
#27098,#27099),(#27100,#27101,#27102,#27103,#27104,#27105,#27106,#27107,
#27108),(#27109,#27110,#27111,#27112,#27113,#27114,#27115,#27116,#27117),
(#27118,#27119,#27120,#27121,#27122,#27123,#27124,#27125,#27126)),
 .UNSPECIFIED.,.F.,.F.,.F.)
B_SPLINE_SURFACE_WITH_KNOTS((4,4),(3,2,2,2,3),(0.,1.),(0.,0.25,0.5,0.75,
1.),.UNSPECIFIED.)
GEOMETRIC_REPRESENTATION_ITEM()
RATIONAL_B_SPLINE_SURFACE(((1.,0.974927912181824,1.,0.974927912181824,1.,
0.974927912181824,1.,0.974927912181824,1.),(0.987189825241073,0.962438915249418,
0.987189825241073,0.962438915249418,0.987189825241073,0.962438915249418,
0.987189825241073,0.962438915249418,0.987189825241073),(0.987189825241073,
0.962438915249418,0.987189825241073,0.962438915249418,0.987189825241073,
0.962438915249418,0.987189825241073,0.962438915249418,0.987189825241073),
(1.,0.974927912181824,1.,0.974927912181824,1.,0.974927912181824,1.,0.974927912181824,
1.)))
REPRESENTATION_ITEM('')
SURFACE()
);
#405=(
BOUNDED_SURFACE()
B_SPLINE_SURFACE(3,2,((#27134,#27135,#27136,#27137,#27138,#27139,#27140,
#27141,#27142),(#27143,#27144,#27145,#27146,#27147,#27148,#27149,#27150,
#27151),(#27152,#27153,#27154,#27155,#27156,#27157,#27158,#27159,#27160),
(#27161,#27162,#27163,#27164,#27165,#27166,#27167,#27168,#27169)),
 .UNSPECIFIED.,.F.,.F.,.F.)
B_SPLINE_SURFACE_WITH_KNOTS((4,4),(3,2,2,2,3),(0.,1.),(0.,0.25,0.5,0.75,
1.),.UNSPECIFIED.)
GEOMETRIC_REPRESENTATION_ITEM()
RATIONAL_B_SPLINE_SURFACE(((1.,0.974927912181824,1.,0.974927912181824,1.,
0.974927912181824,1.,0.974927912181824,1.),(0.833333333333332,0.812439926818185,
0.833333333333332,0.812439926818185,0.833333333333332,0.812439926818185,
0.833333333333332,0.812439926818185,0.833333333333332),(0.833333333333332,
0.812439926818185,0.833333333333332,0.812439926818185,0.833333333333332,
0.812439926818185,0.833333333333332,0.812439926818185,0.833333333333332),
(1.,0.974927912181824,1.,0.974927912181824,1.,0.974927912181824,1.,0.974927912181824,
1.)))
REPRESENTATION_ITEM('')
SURFACE()
);
#406=(
BOUNDED_SURFACE()
B_SPLINE_SURFACE(3,2,((#27173,#27174,#27175,#27176,#27177,#27178,#27179,
#27180,#27181),(#27182,#27183,#27184,#27185,#27186,#27187,#27188,#27189,
#27190),(#27191,#27192,#27193,#27194,#27195,#27196,#27197,#27198,#27199),
(#27200,#27201,#27202,#27203,#27204,#27205,#27206,#27207,#27208)),
 .UNSPECIFIED.,.F.,.F.,.F.)
B_SPLINE_SURFACE_WITH_KNOTS((4,4),(3,2,2,2,3),(0.,1.),(0.,0.25,0.5,0.75,
1.),.UNSPECIFIED.)
GEOMETRIC_REPRESENTATION_ITEM()
RATIONAL_B_SPLINE_SURFACE(((1.,0.974927912181824,1.,0.974927912181824,1.,
0.974927912181824,1.,0.974927912181824,1.),(0.987189825241073,0.962438915249418,
0.987189825241073,0.962438915249418,0.987189825241073,0.962438915249418,
0.987189825241073,0.962438915249418,0.987189825241073),(0.987189825241073,
0.962438915249418,0.987189825241073,0.962438915249418,0.987189825241073,
0.962438915249418,0.987189825241073,0.962438915249418,0.987189825241073),
(1.,0.974927912181824,1.,0.974927912181824,1.,0.974927912181824,1.,0.974927912181824,
1.)))
REPRESENTATION_ITEM('')
SURFACE()
);
#407=(
BOUNDED_SURFACE()
B_SPLINE_SURFACE(3,2,((#27216,#27217,#27218,#27219,#27220,#27221,#27222,
#27223,#27224),(#27225,#27226,#27227,#27228,#27229,#27230,#27231,#27232,
#27233),(#27234,#27235,#27236,#27237,#27238,#27239,#27240,#27241,#27242),
(#27243,#27244,#27245,#27246,#27247,#27248,#27249,#27250,#27251)),
 .UNSPECIFIED.,.F.,.F.,.F.)
B_SPLINE_SURFACE_WITH_KNOTS((4,4),(3,2,2,2,3),(0.,1.),(0.,0.25,0.5,0.75,
1.),.UNSPECIFIED.)
GEOMETRIC_REPRESENTATION_ITEM()
RATIONAL_B_SPLINE_SURFACE(((1.,0.974927912181824,1.,0.974927912181824,1.,
0.974927912181824,1.,0.974927912181824,1.),(0.987189825241073,0.962438915249418,
0.987189825241073,0.962438915249418,0.987189825241073,0.962438915249418,
0.987189825241073,0.962438915249418,0.987189825241073),(0.987189825241073,
0.962438915249418,0.987189825241073,0.962438915249418,0.987189825241073,
0.962438915249418,0.987189825241073,0.962438915249418,0.987189825241073),
(1.,0.974927912181824,1.,0.974927912181824,1.,0.974927912181824,1.,0.974927912181824,
1.)))
REPRESENTATION_ITEM('')
SURFACE()
);
#408=(
BOUNDED_SURFACE()
B_SPLINE_SURFACE(3,2,((#27259,#27260,#27261,#27262,#27263,#27264,#27265,
#27266,#27267),(#27268,#27269,#27270,#27271,#27272,#27273,#27274,#27275,
#27276),(#27277,#27278,#27279,#27280,#27281,#27282,#27283,#27284,#27285),
(#27286,#27287,#27288,#27289,#27290,#27291,#27292,#27293,#27294)),
 .UNSPECIFIED.,.F.,.F.,.F.)
B_SPLINE_SURFACE_WITH_KNOTS((4,4),(3,2,2,2,3),(0.,1.),(0.,0.25,0.5,0.75,
1.),.UNSPECIFIED.)
GEOMETRIC_REPRESENTATION_ITEM()
RATIONAL_B_SPLINE_SURFACE(((1.,0.974927912181824,1.,0.974927912181824,1.,
0.974927912181824,1.,0.974927912181824,1.),(0.833333333333332,0.812439926818185,
0.833333333333332,0.812439926818185,0.833333333333332,0.812439926818185,
0.833333333333332,0.812439926818185,0.833333333333332),(0.833333333333332,
0.812439926818185,0.833333333333332,0.812439926818185,0.833333333333332,
0.812439926818185,0.833333333333332,0.812439926818185,0.833333333333332),
(1.,0.974927912181824,1.,0.974927912181824,1.,0.974927912181824,1.,0.974927912181824,
1.)))
REPRESENTATION_ITEM('')
SURFACE()
);
#409=(
BOUNDED_SURFACE()
B_SPLINE_SURFACE(3,2,((#27298,#27299,#27300,#27301,#27302,#27303,#27304,
#27305,#27306),(#27307,#27308,#27309,#27310,#27311,#27312,#27313,#27314,
#27315),(#27316,#27317,#27318,#27319,#27320,#27321,#27322,#27323,#27324),
(#27325,#27326,#27327,#27328,#27329,#27330,#27331,#27332,#27333)),
 .UNSPECIFIED.,.F.,.F.,.F.)
B_SPLINE_SURFACE_WITH_KNOTS((4,4),(3,2,2,2,3),(0.,1.),(0.,0.25,0.5,0.75,
1.),.UNSPECIFIED.)
GEOMETRIC_REPRESENTATION_ITEM()
RATIONAL_B_SPLINE_SURFACE(((1.,0.974927912181824,1.,0.974927912181824,1.,
0.974927912181824,1.,0.974927912181824,1.),(0.987189825241073,0.962438915249418,
0.987189825241073,0.962438915249418,0.987189825241073,0.962438915249418,
0.987189825241073,0.962438915249418,0.987189825241073),(0.987189825241073,
0.962438915249418,0.987189825241073,0.962438915249418,0.987189825241073,
0.962438915249418,0.987189825241073,0.962438915249418,0.987189825241073),
(1.,0.974927912181824,1.,0.974927912181824,1.,0.974927912181824,1.,0.974927912181824,
1.)))
REPRESENTATION_ITEM('')
SURFACE()
);
#410=(
BOUNDED_SURFACE()
B_SPLINE_SURFACE(3,2,((#27341,#27342,#27343,#27344,#27345,#27346,#27347,
#27348,#27349),(#27350,#27351,#27352,#27353,#27354,#27355,#27356,#27357,
#27358),(#27359,#27360,#27361,#27362,#27363,#27364,#27365,#27366,#27367),
(#27368,#27369,#27370,#27371,#27372,#27373,#27374,#27375,#27376)),
 .UNSPECIFIED.,.F.,.F.,.F.)
B_SPLINE_SURFACE_WITH_KNOTS((4,4),(3,2,2,2,3),(0.,1.),(0.,0.25,0.5,0.75,
1.),.UNSPECIFIED.)
GEOMETRIC_REPRESENTATION_ITEM()
RATIONAL_B_SPLINE_SURFACE(((1.,0.974927912181824,1.,0.974927912181824,1.,
0.974927912181824,1.,0.974927912181824,1.),(0.987189825241073,0.962438915249418,
0.987189825241073,0.962438915249418,0.987189825241073,0.962438915249418,
0.987189825241073,0.962438915249418,0.987189825241073),(0.987189825241073,
0.962438915249418,0.987189825241073,0.962438915249418,0.987189825241073,
0.962438915249418,0.987189825241073,0.962438915249418,0.987189825241073),
(1.,0.974927912181824,1.,0.974927912181824,1.,0.974927912181824,1.,0.974927912181824,
1.)))
REPRESENTATION_ITEM('')
SURFACE()
);
#411=(
BOUNDED_SURFACE()
B_SPLINE_SURFACE(3,2,((#27384,#27385,#27386,#27387,#27388,#27389,#27390,
#27391,#27392),(#27393,#27394,#27395,#27396,#27397,#27398,#27399,#27400,
#27401),(#27402,#27403,#27404,#27405,#27406,#27407,#27408,#27409,#27410),
(#27411,#27412,#27413,#27414,#27415,#27416,#27417,#27418,#27419)),
 .UNSPECIFIED.,.F.,.F.,.F.)
B_SPLINE_SURFACE_WITH_KNOTS((4,4),(3,2,2,2,3),(0.,1.),(0.,0.25,0.5,0.75,
1.),.UNSPECIFIED.)
GEOMETRIC_REPRESENTATION_ITEM()
RATIONAL_B_SPLINE_SURFACE(((1.,0.974927912181824,1.,0.974927912181824,1.,
0.974927912181824,1.,0.974927912181824,1.),(0.833333333333333,0.812439926818186,
0.833333333333333,0.812439926818186,0.833333333333333,0.812439926818186,
0.833333333333333,0.812439926818186,0.833333333333333),(0.833333333333333,
0.812439926818186,0.833333333333333,0.812439926818186,0.833333333333333,
0.812439926818186,0.833333333333333,0.812439926818186,0.833333333333333),
(1.,0.974927912181824,1.,0.974927912181824,1.,0.974927912181824,1.,0.974927912181824,
1.)))
REPRESENTATION_ITEM('')
SURFACE()
);
#412=(
BOUNDED_SURFACE()
B_SPLINE_SURFACE(3,2,((#27423,#27424,#27425,#27426,#27427,#27428,#27429,
#27430,#27431),(#27432,#27433,#27434,#27435,#27436,#27437,#27438,#27439,
#27440),(#27441,#27442,#27443,#27444,#27445,#27446,#27447,#27448,#27449),
(#27450,#27451,#27452,#27453,#27454,#27455,#27456,#27457,#27458)),
 .UNSPECIFIED.,.F.,.F.,.F.)
B_SPLINE_SURFACE_WITH_KNOTS((4,4),(3,2,2,2,3),(0.,1.),(0.,0.25,0.5,0.75,
1.),.UNSPECIFIED.)
GEOMETRIC_REPRESENTATION_ITEM()
RATIONAL_B_SPLINE_SURFACE(((1.,0.974927912181824,1.,0.974927912181824,1.,
0.974927912181824,1.,0.974927912181824,1.),(0.987189825241073,0.962438915249418,
0.987189825241073,0.962438915249418,0.987189825241073,0.962438915249418,
0.987189825241073,0.962438915249418,0.987189825241073),(0.987189825241073,
0.962438915249418,0.987189825241073,0.962438915249418,0.987189825241073,
0.962438915249418,0.987189825241073,0.962438915249418,0.987189825241073),
(1.,0.974927912181824,1.,0.974927912181824,1.,0.974927912181824,1.,0.974927912181824,
1.)))
REPRESENTATION_ITEM('')
SURFACE()
);
#413=(
BOUNDED_SURFACE()
B_SPLINE_SURFACE(3,2,((#27513,#27514,#27515,#27516,#27517,#27518,#27519,
#27520,#27521),(#27522,#27523,#27524,#27525,#27526,#27527,#27528,#27529,
#27530),(#27531,#27532,#27533,#27534,#27535,#27536,#27537,#27538,#27539),
(#27540,#27541,#27542,#27543,#27544,#27545,#27546,#27547,#27548)),
 .UNSPECIFIED.,.F.,.F.,.F.)
B_SPLINE_SURFACE_WITH_KNOTS((4,4),(3,2,2,2,3),(0.,1.),(0.,0.25,0.5,0.75,
1.),.UNSPECIFIED.)
GEOMETRIC_REPRESENTATION_ITEM()
RATIONAL_B_SPLINE_SURFACE(((1.,0.974927912181824,1.,0.974927912181824,1.,
0.974927912181824,1.,0.974927912181824,1.),(0.987189825241073,0.962438915249418,
0.987189825241073,0.962438915249418,0.987189825241073,0.962438915249418,
0.987189825241073,0.962438915249418,0.987189825241073),(0.987189825241073,
0.962438915249418,0.987189825241073,0.962438915249418,0.987189825241073,
0.962438915249418,0.987189825241073,0.962438915249418,0.987189825241073),
(1.,0.974927912181824,1.,0.974927912181824,1.,0.974927912181824,1.,0.974927912181824,
1.)))
REPRESENTATION_ITEM('')
SURFACE()
);
#414=(
BOUNDED_SURFACE()
B_SPLINE_SURFACE(3,2,((#27556,#27557,#27558,#27559,#27560,#27561,#27562,
#27563,#27564),(#27565,#27566,#27567,#27568,#27569,#27570,#27571,#27572,
#27573),(#27574,#27575,#27576,#27577,#27578,#27579,#27580,#27581,#27582),
(#27583,#27584,#27585,#27586,#27587,#27588,#27589,#27590,#27591)),
 .UNSPECIFIED.,.F.,.F.,.F.)
B_SPLINE_SURFACE_WITH_KNOTS((4,4),(3,2,2,2,3),(0.,1.),(0.,0.25,0.5,0.75,
1.),.UNSPECIFIED.)
GEOMETRIC_REPRESENTATION_ITEM()
RATIONAL_B_SPLINE_SURFACE(((1.,0.974927912181824,1.,0.974927912181824,1.,
0.974927912181824,1.,0.974927912181824,1.),(0.833333333333333,0.812439926818186,
0.833333333333333,0.812439926818186,0.833333333333333,0.812439926818186,
0.833333333333333,0.812439926818186,0.833333333333333),(0.833333333333333,
0.812439926818186,0.833333333333333,0.812439926818186,0.833333333333333,
0.812439926818186,0.833333333333333,0.812439926818186,0.833333333333333),
(1.,0.974927912181824,1.,0.974927912181824,1.,0.974927912181824,1.,0.974927912181824,
1.)))
REPRESENTATION_ITEM('')
SURFACE()
);
#415=(
BOUNDED_SURFACE()
B_SPLINE_SURFACE(3,2,((#27595,#27596,#27597,#27598,#27599,#27600,#27601,
#27602,#27603),(#27604,#27605,#27606,#27607,#27608,#27609,#27610,#27611,
#27612),(#27613,#27614,#27615,#27616,#27617,#27618,#27619,#27620,#27621),
(#27622,#27623,#27624,#27625,#27626,#27627,#27628,#27629,#27630)),
 .UNSPECIFIED.,.F.,.F.,.F.)
B_SPLINE_SURFACE_WITH_KNOTS((4,4),(3,2,2,2,3),(0.,1.),(0.,0.25,0.5,0.75,
1.),.UNSPECIFIED.)
GEOMETRIC_REPRESENTATION_ITEM()
RATIONAL_B_SPLINE_SURFACE(((1.,0.974927912181824,1.,0.974927912181824,1.,
0.974927912181824,1.,0.974927912181824,1.),(0.987189825241073,0.962438915249418,
0.987189825241073,0.962438915249418,0.987189825241073,0.962438915249418,
0.987189825241073,0.962438915249418,0.987189825241073),(0.987189825241073,
0.962438915249418,0.987189825241073,0.962438915249418,0.987189825241073,
0.962438915249418,0.987189825241073,0.962438915249418,0.987189825241073),
(1.,0.974927912181824,1.,0.974927912181824,1.,0.974927912181824,1.,0.974927912181824,
1.)))
REPRESENTATION_ITEM('')
SURFACE()
);
#416=(
BOUNDED_SURFACE()
B_SPLINE_SURFACE(3,2,((#27685,#27686,#27687,#27688,#27689,#27690,#27691,
#27692,#27693),(#27694,#27695,#27696,#27697,#27698,#27699,#27700,#27701,
#27702),(#27703,#27704,#27705,#27706,#27707,#27708,#27709,#27710,#27711),
(#27712,#27713,#27714,#27715,#27716,#27717,#27718,#27719,#27720)),
 .UNSPECIFIED.,.F.,.F.,.F.)
B_SPLINE_SURFACE_WITH_KNOTS((4,4),(3,2,2,2,3),(0.,1.),(0.,0.25,0.5,0.75,
1.),.UNSPECIFIED.)
GEOMETRIC_REPRESENTATION_ITEM()
RATIONAL_B_SPLINE_SURFACE(((1.,0.974927912181824,1.,0.974927912181824,1.,
0.974927912181824,1.,0.974927912181824,1.),(0.987189825241073,0.962438915249418,
0.987189825241073,0.962438915249418,0.987189825241073,0.962438915249418,
0.987189825241073,0.962438915249418,0.987189825241073),(0.987189825241073,
0.962438915249418,0.987189825241073,0.962438915249418,0.987189825241073,
0.962438915249418,0.987189825241073,0.962438915249418,0.987189825241073),
(1.,0.974927912181824,1.,0.974927912181824,1.,0.974927912181824,1.,0.974927912181824,
1.)))
REPRESENTATION_ITEM('')
SURFACE()
);
#417=(
BOUNDED_SURFACE()
B_SPLINE_SURFACE(3,2,((#27728,#27729,#27730,#27731,#27732,#27733,#27734,
#27735,#27736),(#27737,#27738,#27739,#27740,#27741,#27742,#27743,#27744,
#27745),(#27746,#27747,#27748,#27749,#27750,#27751,#27752,#27753,#27754),
(#27755,#27756,#27757,#27758,#27759,#27760,#27761,#27762,#27763)),
 .UNSPECIFIED.,.F.,.F.,.F.)
B_SPLINE_SURFACE_WITH_KNOTS((4,4),(3,2,2,2,3),(0.,1.),(0.,0.25,0.5,0.75,
1.),.UNSPECIFIED.)
GEOMETRIC_REPRESENTATION_ITEM()
RATIONAL_B_SPLINE_SURFACE(((1.,0.974927912181824,1.,0.974927912181824,1.,
0.974927912181824,1.,0.974927912181824,1.),(0.833333333333332,0.812439926818185,
0.833333333333332,0.812439926818185,0.833333333333332,0.812439926818185,
0.833333333333332,0.812439926818185,0.833333333333332),(0.833333333333332,
0.812439926818185,0.833333333333332,0.812439926818185,0.833333333333332,
0.812439926818185,0.833333333333332,0.812439926818185,0.833333333333332),
(1.,0.974927912181824,1.,0.974927912181824,1.,0.974927912181824,1.,0.974927912181824,
1.)))
REPRESENTATION_ITEM('')
SURFACE()
);
#418=(
BOUNDED_SURFACE()
B_SPLINE_SURFACE(3,2,((#27767,#27768,#27769,#27770,#27771,#27772,#27773,
#27774,#27775),(#27776,#27777,#27778,#27779,#27780,#27781,#27782,#27783,
#27784),(#27785,#27786,#27787,#27788,#27789,#27790,#27791,#27792,#27793),
(#27794,#27795,#27796,#27797,#27798,#27799,#27800,#27801,#27802)),
 .UNSPECIFIED.,.F.,.F.,.F.)
B_SPLINE_SURFACE_WITH_KNOTS((4,4),(3,2,2,2,3),(0.,1.),(0.,0.25,0.5,0.75,
1.),.UNSPECIFIED.)
GEOMETRIC_REPRESENTATION_ITEM()
RATIONAL_B_SPLINE_SURFACE(((1.,0.974927912181824,1.,0.974927912181824,1.,
0.974927912181824,1.,0.974927912181824,1.),(0.987189825241073,0.962438915249418,
0.987189825241073,0.962438915249418,0.987189825241073,0.962438915249418,
0.987189825241073,0.962438915249418,0.987189825241073),(0.987189825241073,
0.962438915249418,0.987189825241073,0.962438915249418,0.987189825241073,
0.962438915249418,0.987189825241073,0.962438915249418,0.987189825241073),
(1.,0.974927912181824,1.,0.974927912181824,1.,0.974927912181824,1.,0.974927912181824,
1.)))
REPRESENTATION_ITEM('')
SURFACE()
);
#419=(
BOUNDED_SURFACE()
B_SPLINE_SURFACE(3,2,((#27857,#27858,#27859,#27860,#27861,#27862,#27863,
#27864,#27865),(#27866,#27867,#27868,#27869,#27870,#27871,#27872,#27873,
#27874),(#27875,#27876,#27877,#27878,#27879,#27880,#27881,#27882,#27883),
(#27884,#27885,#27886,#27887,#27888,#27889,#27890,#27891,#27892)),
 .UNSPECIFIED.,.F.,.F.,.F.)
B_SPLINE_SURFACE_WITH_KNOTS((4,4),(3,2,2,2,3),(0.,1.),(0.,0.25,0.5,0.75,
1.),.UNSPECIFIED.)
GEOMETRIC_REPRESENTATION_ITEM()
RATIONAL_B_SPLINE_SURFACE(((1.,0.974927912181824,1.,0.974927912181824,1.,
0.974927912181824,1.,0.974927912181824,1.),(0.987189825241073,0.962438915249418,
0.987189825241073,0.962438915249418,0.987189825241073,0.962438915249418,
0.987189825241073,0.962438915249418,0.987189825241073),(0.987189825241073,
0.962438915249418,0.987189825241073,0.962438915249418,0.987189825241073,
0.962438915249418,0.987189825241073,0.962438915249418,0.987189825241073),
(1.,0.974927912181824,1.,0.974927912181824,1.,0.974927912181824,1.,0.974927912181824,
1.)))
REPRESENTATION_ITEM('')
SURFACE()
);
#420=(
BOUNDED_SURFACE()
B_SPLINE_SURFACE(3,2,((#27900,#27901,#27902,#27903,#27904,#27905,#27906,
#27907,#27908),(#27909,#27910,#27911,#27912,#27913,#27914,#27915,#27916,
#27917),(#27918,#27919,#27920,#27921,#27922,#27923,#27924,#27925,#27926),
(#27927,#27928,#27929,#27930,#27931,#27932,#27933,#27934,#27935)),
 .UNSPECIFIED.,.F.,.F.,.F.)
B_SPLINE_SURFACE_WITH_KNOTS((4,4),(3,2,2,2,3),(0.,1.),(0.,0.25,0.5,0.75,
1.),.UNSPECIFIED.)
GEOMETRIC_REPRESENTATION_ITEM()
RATIONAL_B_SPLINE_SURFACE(((1.,0.974927912181824,1.,0.974927912181824,1.,
0.974927912181824,1.,0.974927912181824,1.),(0.833333333333333,0.812439926818186,
0.833333333333333,0.812439926818186,0.833333333333333,0.812439926818186,
0.833333333333333,0.812439926818186,0.833333333333333),(0.833333333333333,
0.812439926818186,0.833333333333333,0.812439926818186,0.833333333333333,
0.812439926818186,0.833333333333333,0.812439926818186,0.833333333333333),
(1.,0.974927912181824,1.,0.974927912181824,1.,0.974927912181824,1.,0.974927912181824,
1.)))
REPRESENTATION_ITEM('')
SURFACE()
);
#421=(
BOUNDED_SURFACE()
B_SPLINE_SURFACE(3,2,((#27939,#27940,#27941,#27942,#27943,#27944,#27945,
#27946,#27947),(#27948,#27949,#27950,#27951,#27952,#27953,#27954,#27955,
#27956),(#27957,#27958,#27959,#27960,#27961,#27962,#27963,#27964,#27965),
(#27966,#27967,#27968,#27969,#27970,#27971,#27972,#27973,#27974)),
 .UNSPECIFIED.,.F.,.F.,.F.)
B_SPLINE_SURFACE_WITH_KNOTS((4,4),(3,2,2,2,3),(0.,1.),(0.,0.25,0.5,0.75,
1.),.UNSPECIFIED.)
GEOMETRIC_REPRESENTATION_ITEM()
RATIONAL_B_SPLINE_SURFACE(((1.,0.974927912181824,1.,0.974927912181824,1.,
0.974927912181824,1.,0.974927912181824,1.),(0.987189825241073,0.962438915249418,
0.987189825241073,0.962438915249418,0.987189825241073,0.962438915249418,
0.987189825241073,0.962438915249418,0.987189825241073),(0.987189825241073,
0.962438915249418,0.987189825241073,0.962438915249418,0.987189825241073,
0.962438915249418,0.987189825241073,0.962438915249418,0.987189825241073),
(1.,0.974927912181824,1.,0.974927912181824,1.,0.974927912181824,1.,0.974927912181824,
1.)))
REPRESENTATION_ITEM('')
SURFACE()
);
#422=(
BOUNDED_SURFACE()
B_SPLINE_SURFACE(3,2,((#28029,#28030,#28031,#28032,#28033,#28034,#28035,
#28036,#28037),(#28038,#28039,#28040,#28041,#28042,#28043,#28044,#28045,
#28046),(#28047,#28048,#28049,#28050,#28051,#28052,#28053,#28054,#28055),
(#28056,#28057,#28058,#28059,#28060,#28061,#28062,#28063,#28064)),
 .UNSPECIFIED.,.F.,.F.,.F.)
B_SPLINE_SURFACE_WITH_KNOTS((4,4),(3,2,2,2,3),(0.,1.),(0.,0.25,0.5,0.75,
1.),.UNSPECIFIED.)
GEOMETRIC_REPRESENTATION_ITEM()
RATIONAL_B_SPLINE_SURFACE(((1.,0.974927912181824,1.,0.974927912181824,1.,
0.974927912181824,1.,0.974927912181824,1.),(0.987189825241073,0.962438915249418,
0.987189825241073,0.962438915249418,0.987189825241073,0.962438915249418,
0.987189825241073,0.962438915249418,0.987189825241073),(0.987189825241073,
0.962438915249418,0.987189825241073,0.962438915249418,0.987189825241073,
0.962438915249418,0.987189825241073,0.962438915249418,0.987189825241073),
(1.,0.974927912181824,1.,0.974927912181824,1.,0.974927912181824,1.,0.974927912181824,
1.)))
REPRESENTATION_ITEM('')
SURFACE()
);
#423=(
BOUNDED_SURFACE()
B_SPLINE_SURFACE(3,2,((#28072,#28073,#28074,#28075,#28076,#28077,#28078,
#28079,#28080),(#28081,#28082,#28083,#28084,#28085,#28086,#28087,#28088,
#28089),(#28090,#28091,#28092,#28093,#28094,#28095,#28096,#28097,#28098),
(#28099,#28100,#28101,#28102,#28103,#28104,#28105,#28106,#28107)),
 .UNSPECIFIED.,.F.,.F.,.F.)
B_SPLINE_SURFACE_WITH_KNOTS((4,4),(3,2,2,2,3),(0.,1.),(0.,0.25,0.5,0.75,
1.),.UNSPECIFIED.)
GEOMETRIC_REPRESENTATION_ITEM()
RATIONAL_B_SPLINE_SURFACE(((1.,0.974927912181824,1.,0.974927912181824,1.,
0.974927912181824,1.,0.974927912181824,1.),(0.833333333333332,0.812439926818185,
0.833333333333332,0.812439926818185,0.833333333333332,0.812439926818185,
0.833333333333332,0.812439926818185,0.833333333333332),(0.833333333333332,
0.812439926818185,0.833333333333332,0.812439926818185,0.833333333333332,
0.812439926818185,0.833333333333332,0.812439926818185,0.833333333333332),
(1.,0.974927912181824,1.,0.974927912181824,1.,0.974927912181824,1.,0.974927912181824,
1.)))
REPRESENTATION_ITEM('')
SURFACE()
);
#424=(
BOUNDED_SURFACE()
B_SPLINE_SURFACE(3,2,((#28111,#28112,#28113,#28114,#28115,#28116,#28117,
#28118,#28119),(#28120,#28121,#28122,#28123,#28124,#28125,#28126,#28127,
#28128),(#28129,#28130,#28131,#28132,#28133,#28134,#28135,#28136,#28137),
(#28138,#28139,#28140,#28141,#28142,#28143,#28144,#28145,#28146)),
 .UNSPECIFIED.,.F.,.F.,.F.)
B_SPLINE_SURFACE_WITH_KNOTS((4,4),(3,2,2,2,3),(0.,1.),(0.,0.25,0.5,0.75,
1.),.UNSPECIFIED.)
GEOMETRIC_REPRESENTATION_ITEM()
RATIONAL_B_SPLINE_SURFACE(((1.,0.974927912181824,1.,0.974927912181824,1.,
0.974927912181824,1.,0.974927912181824,1.),(0.987189825241073,0.962438915249418,
0.987189825241073,0.962438915249418,0.987189825241073,0.962438915249418,
0.987189825241073,0.962438915249418,0.987189825241073),(0.987189825241073,
0.962438915249418,0.987189825241073,0.962438915249418,0.987189825241073,
0.962438915249418,0.987189825241073,0.962438915249418,0.987189825241073),
(1.,0.974927912181824,1.,0.974927912181824,1.,0.974927912181824,1.,0.974927912181824,
1.)))
REPRESENTATION_ITEM('')
SURFACE()
);
#425=(
BOUNDED_SURFACE()
B_SPLINE_SURFACE(3,2,((#28201,#28202,#28203,#28204,#28205,#28206,#28207,
#28208,#28209),(#28210,#28211,#28212,#28213,#28214,#28215,#28216,#28217,
#28218),(#28219,#28220,#28221,#28222,#28223,#28224,#28225,#28226,#28227),
(#28228,#28229,#28230,#28231,#28232,#28233,#28234,#28235,#28236)),
 .UNSPECIFIED.,.F.,.F.,.F.)
B_SPLINE_SURFACE_WITH_KNOTS((4,4),(3,2,2,2,3),(0.,1.),(0.,0.25,0.5,0.75,
1.),.UNSPECIFIED.)
GEOMETRIC_REPRESENTATION_ITEM()
RATIONAL_B_SPLINE_SURFACE(((1.,0.974927912181824,1.,0.974927912181824,1.,
0.974927912181824,1.,0.974927912181824,1.),(0.987189825241073,0.962438915249418,
0.987189825241073,0.962438915249418,0.987189825241073,0.962438915249418,
0.987189825241073,0.962438915249418,0.987189825241073),(0.987189825241073,
0.962438915249418,0.987189825241073,0.962438915249418,0.987189825241073,
0.962438915249418,0.987189825241073,0.962438915249418,0.987189825241073),
(1.,0.974927912181824,1.,0.974927912181824,1.,0.974927912181824,1.,0.974927912181824,
1.)))
REPRESENTATION_ITEM('')
SURFACE()
);
#426=(
BOUNDED_SURFACE()
B_SPLINE_SURFACE(3,2,((#28244,#28245,#28246,#28247,#28248,#28249,#28250,
#28251,#28252),(#28253,#28254,#28255,#28256,#28257,#28258,#28259,#28260,
#28261),(#28262,#28263,#28264,#28265,#28266,#28267,#28268,#28269,#28270),
(#28271,#28272,#28273,#28274,#28275,#28276,#28277,#28278,#28279)),
 .UNSPECIFIED.,.F.,.F.,.F.)
B_SPLINE_SURFACE_WITH_KNOTS((4,4),(3,2,2,2,3),(0.,1.),(0.,0.25,0.5,0.75,
1.),.UNSPECIFIED.)
GEOMETRIC_REPRESENTATION_ITEM()
RATIONAL_B_SPLINE_SURFACE(((1.,0.974927912181824,1.,0.974927912181824,1.,
0.974927912181824,1.,0.974927912181824,1.),(0.833333333333333,0.812439926818186,
0.833333333333333,0.812439926818186,0.833333333333333,0.812439926818186,
0.833333333333333,0.812439926818186,0.833333333333333),(0.833333333333333,
0.812439926818186,0.833333333333333,0.812439926818186,0.833333333333333,
0.812439926818186,0.833333333333333,0.812439926818186,0.833333333333333),
(1.,0.974927912181824,1.,0.974927912181824,1.,0.974927912181824,1.,0.974927912181824,
1.)))
REPRESENTATION_ITEM('')
SURFACE()
);
#427=(
BOUNDED_SURFACE()
B_SPLINE_SURFACE(3,2,((#28283,#28284,#28285,#28286,#28287,#28288,#28289,
#28290,#28291),(#28292,#28293,#28294,#28295,#28296,#28297,#28298,#28299,
#28300),(#28301,#28302,#28303,#28304,#28305,#28306,#28307,#28308,#28309),
(#28310,#28311,#28312,#28313,#28314,#28315,#28316,#28317,#28318)),
 .UNSPECIFIED.,.F.,.F.,.F.)
B_SPLINE_SURFACE_WITH_KNOTS((4,4),(3,2,2,2,3),(0.,1.),(0.,0.25,0.5,0.75,
1.),.UNSPECIFIED.)
GEOMETRIC_REPRESENTATION_ITEM()
RATIONAL_B_SPLINE_SURFACE(((1.,0.974927912181824,1.,0.974927912181824,1.,
0.974927912181824,1.,0.974927912181824,1.),(0.987189825241073,0.962438915249418,
0.987189825241073,0.962438915249418,0.987189825241073,0.962438915249418,
0.987189825241073,0.962438915249418,0.987189825241073),(0.987189825241073,
0.962438915249418,0.987189825241073,0.962438915249418,0.987189825241073,
0.962438915249418,0.987189825241073,0.962438915249418,0.987189825241073),
(1.,0.974927912181824,1.,0.974927912181824,1.,0.974927912181824,1.,0.974927912181824,
1.)))
REPRESENTATION_ITEM('')
SURFACE()
);
#428=(
BOUNDED_SURFACE()
B_SPLINE_SURFACE(3,2,((#28373,#28374,#28375,#28376,#28377,#28378,#28379,
#28380,#28381),(#28382,#28383,#28384,#28385,#28386,#28387,#28388,#28389,
#28390),(#28391,#28392,#28393,#28394,#28395,#28396,#28397,#28398,#28399),
(#28400,#28401,#28402,#28403,#28404,#28405,#28406,#28407,#28408)),
 .UNSPECIFIED.,.F.,.F.,.F.)
B_SPLINE_SURFACE_WITH_KNOTS((4,4),(3,2,2,2,3),(0.,1.),(0.,0.25,0.5,0.75,
1.),.UNSPECIFIED.)
GEOMETRIC_REPRESENTATION_ITEM()
RATIONAL_B_SPLINE_SURFACE(((1.,0.974927912181824,1.,0.974927912181824,1.,
0.974927912181824,1.,0.974927912181824,1.),(0.987189825241073,0.962438915249418,
0.987189825241073,0.962438915249418,0.987189825241073,0.962438915249418,
0.987189825241073,0.962438915249418,0.987189825241073),(0.987189825241073,
0.962438915249418,0.987189825241073,0.962438915249418,0.987189825241073,
0.962438915249418,0.987189825241073,0.962438915249418,0.987189825241073),
(1.,0.974927912181824,1.,0.974927912181824,1.,0.974927912181824,1.,0.974927912181824,
1.)))
REPRESENTATION_ITEM('')
SURFACE()
);
#429=(
BOUNDED_SURFACE()
B_SPLINE_SURFACE(3,2,((#28416,#28417,#28418,#28419,#28420,#28421,#28422,
#28423,#28424),(#28425,#28426,#28427,#28428,#28429,#28430,#28431,#28432,
#28433),(#28434,#28435,#28436,#28437,#28438,#28439,#28440,#28441,#28442),
(#28443,#28444,#28445,#28446,#28447,#28448,#28449,#28450,#28451)),
 .UNSPECIFIED.,.F.,.F.,.F.)
B_SPLINE_SURFACE_WITH_KNOTS((4,4),(3,2,2,2,3),(0.,1.),(0.,0.25,0.5,0.75,
1.),.UNSPECIFIED.)
GEOMETRIC_REPRESENTATION_ITEM()
RATIONAL_B_SPLINE_SURFACE(((1.,0.974927912181824,1.,0.974927912181824,1.,
0.974927912181824,1.,0.974927912181824,1.),(0.833333333333332,0.812439926818185,
0.833333333333332,0.812439926818185,0.833333333333332,0.812439926818185,
0.833333333333332,0.812439926818185,0.833333333333332),(0.833333333333332,
0.812439926818185,0.833333333333332,0.812439926818185,0.833333333333332,
0.812439926818185,0.833333333333332,0.812439926818185,0.833333333333332),
(1.,0.974927912181824,1.,0.974927912181824,1.,0.974927912181824,1.,0.974927912181824,
1.)))
REPRESENTATION_ITEM('')
SURFACE()
);
#430=(
BOUNDED_SURFACE()
B_SPLINE_SURFACE(3,2,((#28455,#28456,#28457,#28458,#28459,#28460,#28461,
#28462,#28463),(#28464,#28465,#28466,#28467,#28468,#28469,#28470,#28471,
#28472),(#28473,#28474,#28475,#28476,#28477,#28478,#28479,#28480,#28481),
(#28482,#28483,#28484,#28485,#28486,#28487,#28488,#28489,#28490)),
 .UNSPECIFIED.,.F.,.F.,.F.)
B_SPLINE_SURFACE_WITH_KNOTS((4,4),(3,2,2,2,3),(0.,1.),(0.,0.25,0.5,0.75,
1.),.UNSPECIFIED.)
GEOMETRIC_REPRESENTATION_ITEM()
RATIONAL_B_SPLINE_SURFACE(((1.,0.974927912181824,1.,0.974927912181824,1.,
0.974927912181824,1.,0.974927912181824,1.),(0.987189825241073,0.962438915249418,
0.987189825241073,0.962438915249418,0.987189825241073,0.962438915249418,
0.987189825241073,0.962438915249418,0.987189825241073),(0.987189825241073,
0.962438915249418,0.987189825241073,0.962438915249418,0.987189825241073,
0.962438915249418,0.987189825241073,0.962438915249418,0.987189825241073),
(1.,0.974927912181824,1.,0.974927912181824,1.,0.974927912181824,1.,0.974927912181824,
1.)))
REPRESENTATION_ITEM('')
SURFACE()
);
#431=(
BOUNDED_SURFACE()
B_SPLINE_SURFACE(3,2,((#28498,#28499,#28500,#28501,#28502,#28503,#28504,
#28505,#28506),(#28507,#28508,#28509,#28510,#28511,#28512,#28513,#28514,
#28515),(#28516,#28517,#28518,#28519,#28520,#28521,#28522,#28523,#28524),
(#28525,#28526,#28527,#28528,#28529,#28530,#28531,#28532,#28533)),
 .UNSPECIFIED.,.F.,.F.,.F.)
B_SPLINE_SURFACE_WITH_KNOTS((4,4),(3,2,2,2,3),(0.,1.),(0.,0.25,0.5,0.75,
1.),.UNSPECIFIED.)
GEOMETRIC_REPRESENTATION_ITEM()
RATIONAL_B_SPLINE_SURFACE(((1.,0.974927912181824,1.,0.974927912181824,1.,
0.974927912181824,1.,0.974927912181824,1.),(0.987189825241073,0.962438915249418,
0.987189825241073,0.962438915249418,0.987189825241073,0.962438915249418,
0.987189825241073,0.962438915249418,0.987189825241073),(0.987189825241073,
0.962438915249418,0.987189825241073,0.962438915249418,0.987189825241073,
0.962438915249418,0.987189825241073,0.962438915249418,0.987189825241073),
(1.,0.974927912181824,1.,0.974927912181824,1.,0.974927912181824,1.,0.974927912181824,
1.)))
REPRESENTATION_ITEM('')
SURFACE()
);
#432=(
BOUNDED_SURFACE()
B_SPLINE_SURFACE(3,2,((#28541,#28542,#28543,#28544,#28545,#28546,#28547,
#28548,#28549),(#28550,#28551,#28552,#28553,#28554,#28555,#28556,#28557,
#28558),(#28559,#28560,#28561,#28562,#28563,#28564,#28565,#28566,#28567),
(#28568,#28569,#28570,#28571,#28572,#28573,#28574,#28575,#28576)),
 .UNSPECIFIED.,.F.,.F.,.F.)
B_SPLINE_SURFACE_WITH_KNOTS((4,4),(3,2,2,2,3),(0.,1.),(0.,0.25,0.5,0.75,
1.),.UNSPECIFIED.)
GEOMETRIC_REPRESENTATION_ITEM()
RATIONAL_B_SPLINE_SURFACE(((1.,0.974927912181824,1.,0.974927912181824,1.,
0.974927912181824,1.,0.974927912181824,1.),(0.833333333333332,0.812439926818185,
0.833333333333332,0.812439926818185,0.833333333333332,0.812439926818185,
0.833333333333332,0.812439926818185,0.833333333333332),(0.833333333333332,
0.812439926818185,0.833333333333332,0.812439926818185,0.833333333333332,
0.812439926818185,0.833333333333332,0.812439926818185,0.833333333333332),
(1.,0.974927912181824,1.,0.974927912181824,1.,0.974927912181824,1.,0.974927912181824,
1.)))
REPRESENTATION_ITEM('')
SURFACE()
);
#433=(
BOUNDED_SURFACE()
B_SPLINE_SURFACE(3,2,((#28580,#28581,#28582,#28583,#28584,#28585,#28586,
#28587,#28588),(#28589,#28590,#28591,#28592,#28593,#28594,#28595,#28596,
#28597),(#28598,#28599,#28600,#28601,#28602,#28603,#28604,#28605,#28606),
(#28607,#28608,#28609,#28610,#28611,#28612,#28613,#28614,#28615)),
 .UNSPECIFIED.,.F.,.F.,.F.)
B_SPLINE_SURFACE_WITH_KNOTS((4,4),(3,2,2,2,3),(0.,1.),(0.,0.25,0.5,0.75,
1.),.UNSPECIFIED.)
GEOMETRIC_REPRESENTATION_ITEM()
RATIONAL_B_SPLINE_SURFACE(((1.,0.974927912181824,1.,0.974927912181824,1.,
0.974927912181824,1.,0.974927912181824,1.),(0.987189825241073,0.962438915249418,
0.987189825241073,0.962438915249418,0.987189825241073,0.962438915249418,
0.987189825241073,0.962438915249418,0.987189825241073),(0.987189825241073,
0.962438915249418,0.987189825241073,0.962438915249418,0.987189825241073,
0.962438915249418,0.987189825241073,0.962438915249418,0.987189825241073),
(1.,0.974927912181824,1.,0.974927912181824,1.,0.974927912181824,1.,0.974927912181824,
1.)))
REPRESENTATION_ITEM('')
SURFACE()
);
#434=(
BOUNDED_SURFACE()
B_SPLINE_SURFACE(3,2,((#28623,#28624,#28625,#28626,#28627,#28628,#28629,
#28630,#28631),(#28632,#28633,#28634,#28635,#28636,#28637,#28638,#28639,
#28640),(#28641,#28642,#28643,#28644,#28645,#28646,#28647,#28648,#28649),
(#28650,#28651,#28652,#28653,#28654,#28655,#28656,#28657,#28658)),
 .UNSPECIFIED.,.F.,.F.,.F.)
B_SPLINE_SURFACE_WITH_KNOTS((4,4),(3,2,2,2,3),(0.,1.),(0.,0.25,0.5,0.75,
1.),.UNSPECIFIED.)
GEOMETRIC_REPRESENTATION_ITEM()
RATIONAL_B_SPLINE_SURFACE(((1.,0.974927912181824,1.,0.974927912181824,1.,
0.974927912181824,1.,0.974927912181824,1.),(0.987189825241073,0.962438915249418,
0.987189825241073,0.962438915249418,0.987189825241073,0.962438915249418,
0.987189825241073,0.962438915249418,0.987189825241073),(0.987189825241073,
0.962438915249418,0.987189825241073,0.962438915249418,0.987189825241073,
0.962438915249418,0.987189825241073,0.962438915249418,0.987189825241073),
(1.,0.974927912181824,1.,0.974927912181824,1.,0.974927912181824,1.,0.974927912181824,
1.)))
REPRESENTATION_ITEM('')
SURFACE()
);
#435=(
BOUNDED_SURFACE()
B_SPLINE_SURFACE(3,2,((#28666,#28667,#28668,#28669,#28670,#28671,#28672,
#28673,#28674),(#28675,#28676,#28677,#28678,#28679,#28680,#28681,#28682,
#28683),(#28684,#28685,#28686,#28687,#28688,#28689,#28690,#28691,#28692),
(#28693,#28694,#28695,#28696,#28697,#28698,#28699,#28700,#28701)),
 .UNSPECIFIED.,.F.,.F.,.F.)
B_SPLINE_SURFACE_WITH_KNOTS((4,4),(3,2,2,2,3),(0.,1.),(0.,0.25,0.5,0.75,
1.),.UNSPECIFIED.)
GEOMETRIC_REPRESENTATION_ITEM()
RATIONAL_B_SPLINE_SURFACE(((1.,0.974927912181824,1.,0.974927912181824,1.,
0.974927912181824,1.,0.974927912181824,1.),(0.833333333333333,0.812439926818186,
0.833333333333333,0.812439926818186,0.833333333333333,0.812439926818186,
0.833333333333333,0.812439926818186,0.833333333333333),(0.833333333333333,
0.812439926818186,0.833333333333333,0.812439926818186,0.833333333333333,
0.812439926818186,0.833333333333333,0.812439926818186,0.833333333333333),
(1.,0.974927912181824,1.,0.974927912181824,1.,0.974927912181824,1.,0.974927912181824,
1.)))
REPRESENTATION_ITEM('')
SURFACE()
);
#436=(
BOUNDED_SURFACE()
B_SPLINE_SURFACE(3,2,((#28705,#28706,#28707,#28708,#28709,#28710,#28711,
#28712,#28713),(#28714,#28715,#28716,#28717,#28718,#28719,#28720,#28721,
#28722),(#28723,#28724,#28725,#28726,#28727,#28728,#28729,#28730,#28731),
(#28732,#28733,#28734,#28735,#28736,#28737,#28738,#28739,#28740)),
 .UNSPECIFIED.,.F.,.F.,.F.)
B_SPLINE_SURFACE_WITH_KNOTS((4,4),(3,2,2,2,3),(0.,1.),(0.,0.25,0.5,0.75,
1.),.UNSPECIFIED.)
GEOMETRIC_REPRESENTATION_ITEM()
RATIONAL_B_SPLINE_SURFACE(((1.,0.974927912181824,1.,0.974927912181824,1.,
0.974927912181824,1.,0.974927912181824,1.),(0.987189825241073,0.962438915249418,
0.987189825241073,0.962438915249418,0.987189825241073,0.962438915249418,
0.987189825241073,0.962438915249418,0.987189825241073),(0.987189825241073,
0.962438915249418,0.987189825241073,0.962438915249418,0.987189825241073,
0.962438915249418,0.987189825241073,0.962438915249418,0.987189825241073),
(1.,0.974927912181824,1.,0.974927912181824,1.,0.974927912181824,1.,0.974927912181824,
1.)))
REPRESENTATION_ITEM('')
SURFACE()
);
#437=(
BOUNDED_SURFACE()
B_SPLINE_SURFACE(3,2,((#28795,#28796,#28797,#28798,#28799,#28800,#28801,
#28802,#28803),(#28804,#28805,#28806,#28807,#28808,#28809,#28810,#28811,
#28812),(#28813,#28814,#28815,#28816,#28817,#28818,#28819,#28820,#28821),
(#28822,#28823,#28824,#28825,#28826,#28827,#28828,#28829,#28830)),
 .UNSPECIFIED.,.F.,.F.,.F.)
B_SPLINE_SURFACE_WITH_KNOTS((4,4),(3,2,2,2,3),(0.,1.),(0.,0.25,0.5,0.75,
1.),.UNSPECIFIED.)
GEOMETRIC_REPRESENTATION_ITEM()
RATIONAL_B_SPLINE_SURFACE(((1.,0.974927912181824,1.,0.974927912181824,1.,
0.974927912181824,1.,0.974927912181824,1.),(0.987189825241073,0.962438915249418,
0.987189825241073,0.962438915249418,0.987189825241073,0.962438915249418,
0.987189825241073,0.962438915249418,0.987189825241073),(0.987189825241073,
0.962438915249418,0.987189825241073,0.962438915249418,0.987189825241073,
0.962438915249418,0.987189825241073,0.962438915249418,0.987189825241073),
(1.,0.974927912181824,1.,0.974927912181824,1.,0.974927912181824,1.,0.974927912181824,
1.)))
REPRESENTATION_ITEM('')
SURFACE()
);
#438=(
BOUNDED_SURFACE()
B_SPLINE_SURFACE(3,2,((#28838,#28839,#28840,#28841,#28842,#28843,#28844,
#28845,#28846),(#28847,#28848,#28849,#28850,#28851,#28852,#28853,#28854,
#28855),(#28856,#28857,#28858,#28859,#28860,#28861,#28862,#28863,#28864),
(#28865,#28866,#28867,#28868,#28869,#28870,#28871,#28872,#28873)),
 .UNSPECIFIED.,.F.,.F.,.F.)
B_SPLINE_SURFACE_WITH_KNOTS((4,4),(3,2,2,2,3),(0.,1.),(0.,0.25,0.5,0.75,
1.),.UNSPECIFIED.)
GEOMETRIC_REPRESENTATION_ITEM()
RATIONAL_B_SPLINE_SURFACE(((1.,0.974927912181824,1.,0.974927912181824,1.,
0.974927912181824,1.,0.974927912181824,1.),(0.833333333333332,0.812439926818185,
0.833333333333332,0.812439926818185,0.833333333333332,0.812439926818185,
0.833333333333332,0.812439926818185,0.833333333333332),(0.833333333333332,
0.812439926818185,0.833333333333332,0.812439926818185,0.833333333333332,
0.812439926818185,0.833333333333332,0.812439926818185,0.833333333333332),
(1.,0.974927912181824,1.,0.974927912181824,1.,0.974927912181824,1.,0.974927912181824,
1.)))
REPRESENTATION_ITEM('')
SURFACE()
);
#439=(
BOUNDED_SURFACE()
B_SPLINE_SURFACE(3,2,((#28877,#28878,#28879,#28880,#28881,#28882,#28883,
#28884,#28885),(#28886,#28887,#28888,#28889,#28890,#28891,#28892,#28893,
#28894),(#28895,#28896,#28897,#28898,#28899,#28900,#28901,#28902,#28903),
(#28904,#28905,#28906,#28907,#28908,#28909,#28910,#28911,#28912)),
 .UNSPECIFIED.,.F.,.F.,.F.)
B_SPLINE_SURFACE_WITH_KNOTS((4,4),(3,2,2,2,3),(0.,1.),(0.,0.25,0.5,0.75,
1.),.UNSPECIFIED.)
GEOMETRIC_REPRESENTATION_ITEM()
RATIONAL_B_SPLINE_SURFACE(((1.,0.974927912181824,1.,0.974927912181824,1.,
0.974927912181824,1.,0.974927912181824,1.),(0.987189825241073,0.962438915249418,
0.987189825241073,0.962438915249418,0.987189825241073,0.962438915249418,
0.987189825241073,0.962438915249418,0.987189825241073),(0.987189825241073,
0.962438915249418,0.987189825241073,0.962438915249418,0.987189825241073,
0.962438915249418,0.987189825241073,0.962438915249418,0.987189825241073),
(1.,0.974927912181824,1.,0.974927912181824,1.,0.974927912181824,1.,0.974927912181824,
1.)))
REPRESENTATION_ITEM('')
SURFACE()
);
#440=(
BOUNDED_SURFACE()
B_SPLINE_SURFACE(3,2,((#28967,#28968,#28969,#28970,#28971,#28972,#28973,
#28974,#28975),(#28976,#28977,#28978,#28979,#28980,#28981,#28982,#28983,
#28984),(#28985,#28986,#28987,#28988,#28989,#28990,#28991,#28992,#28993),
(#28994,#28995,#28996,#28997,#28998,#28999,#29000,#29001,#29002)),
 .UNSPECIFIED.,.F.,.F.,.F.)
B_SPLINE_SURFACE_WITH_KNOTS((4,4),(3,2,2,2,3),(0.,1.),(0.,0.25,0.5,0.75,
1.),.UNSPECIFIED.)
GEOMETRIC_REPRESENTATION_ITEM()
RATIONAL_B_SPLINE_SURFACE(((1.,0.974927912181824,1.,0.974927912181824,1.,
0.974927912181824,1.,0.974927912181824,1.),(0.987189825241073,0.962438915249418,
0.987189825241073,0.962438915249418,0.987189825241073,0.962438915249418,
0.987189825241073,0.962438915249418,0.987189825241073),(0.987189825241073,
0.962438915249418,0.987189825241073,0.962438915249418,0.987189825241073,
0.962438915249418,0.987189825241073,0.962438915249418,0.987189825241073),
(1.,0.974927912181824,1.,0.974927912181824,1.,0.974927912181824,1.,0.974927912181824,
1.)))
REPRESENTATION_ITEM('')
SURFACE()
);
#441=(
BOUNDED_SURFACE()
B_SPLINE_SURFACE(3,2,((#29010,#29011,#29012,#29013,#29014,#29015,#29016,
#29017,#29018),(#29019,#29020,#29021,#29022,#29023,#29024,#29025,#29026,
#29027),(#29028,#29029,#29030,#29031,#29032,#29033,#29034,#29035,#29036),
(#29037,#29038,#29039,#29040,#29041,#29042,#29043,#29044,#29045)),
 .UNSPECIFIED.,.F.,.F.,.F.)
B_SPLINE_SURFACE_WITH_KNOTS((4,4),(3,2,2,2,3),(0.,1.),(0.,0.25,0.5,0.75,
1.),.UNSPECIFIED.)
GEOMETRIC_REPRESENTATION_ITEM()
RATIONAL_B_SPLINE_SURFACE(((1.,0.974927912181824,1.,0.974927912181824,1.,
0.974927912181824,1.,0.974927912181824,1.),(0.833333333333331,0.812439926818184,
0.833333333333331,0.812439926818184,0.833333333333331,0.812439926818184,
0.833333333333331,0.812439926818184,0.833333333333331),(0.833333333333331,
0.812439926818184,0.833333333333331,0.812439926818184,0.833333333333331,
0.812439926818184,0.833333333333331,0.812439926818184,0.833333333333331),
(1.,0.974927912181824,1.,0.974927912181824,1.,0.974927912181824,1.,0.974927912181824,
1.)))
REPRESENTATION_ITEM('')
SURFACE()
);
#442=(
BOUNDED_SURFACE()
B_SPLINE_SURFACE(3,2,((#29049,#29050,#29051,#29052,#29053,#29054,#29055,
#29056,#29057),(#29058,#29059,#29060,#29061,#29062,#29063,#29064,#29065,
#29066),(#29067,#29068,#29069,#29070,#29071,#29072,#29073,#29074,#29075),
(#29076,#29077,#29078,#29079,#29080,#29081,#29082,#29083,#29084)),
 .UNSPECIFIED.,.F.,.F.,.F.)
B_SPLINE_SURFACE_WITH_KNOTS((4,4),(3,2,2,2,3),(0.,1.),(0.,0.0714285714285714,
0.142857142857143,0.214285714285714,0.25),.UNSPECIFIED.)
GEOMETRIC_REPRESENTATION_ITEM()
RATIONAL_B_SPLINE_SURFACE(((1.,0.974927912181824,1.,0.974927912181824,1.,
0.974927912181824,1.,0.987463956090912,0.987463956090912),(0.987189825241073,
0.962438915249418,0.987189825241073,0.962438915249418,0.987189825241073,
0.962438915249418,0.987189825241073,0.974814370245245,0.974814370245245),
(0.987189825241073,0.962438915249418,0.987189825241073,0.962438915249418,
0.987189825241073,0.962438915249418,0.987189825241073,0.974814370245245,
0.974814370245245),(1.,0.974927912181824,1.,0.974927912181824,1.,0.974927912181824,
1.,0.987463956090912,0.987463956090912)))
REPRESENTATION_ITEM('')
SURFACE()
);
#443=(
BOUNDED_SURFACE()
B_SPLINE_SURFACE(3,2,((#29092,#29093,#29094,#29095,#29096,#29097,#29098,
#29099,#29100),(#29101,#29102,#29103,#29104,#29105,#29106,#29107,#29108,
#29109),(#29110,#29111,#29112,#29113,#29114,#29115,#29116,#29117,#29118),
(#29119,#29120,#29121,#29122,#29123,#29124,#29125,#29126,#29127)),
 .UNSPECIFIED.,.F.,.F.,.F.)
B_SPLINE_SURFACE_WITH_KNOTS((4,4),(3,2,2,2,3),(0.,1.),(0.,0.0714285714285714,
0.142857142857143,0.214285714285714,0.25),.UNSPECIFIED.)
GEOMETRIC_REPRESENTATION_ITEM()
RATIONAL_B_SPLINE_SURFACE(((1.,0.974927912181824,1.,0.974927912181824,1.,
0.974927912181824,1.,0.987463956090912,0.987463956090912),(0.987189825241073,
0.962438915249418,0.987189825241073,0.962438915249418,0.987189825241073,
0.962438915249418,0.987189825241073,0.974814370245245,0.974814370245245),
(0.987189825241073,0.962438915249418,0.987189825241073,0.962438915249418,
0.987189825241073,0.962438915249418,0.987189825241073,0.974814370245245,
0.974814370245245),(1.,0.974927912181824,1.,0.974927912181824,1.,0.974927912181824,
1.,0.987463956090912,0.987463956090912)))
REPRESENTATION_ITEM('')
SURFACE()
);
#444=(
BOUNDED_SURFACE()
B_SPLINE_SURFACE(3,2,((#29135,#29136,#29137,#29138,#29139,#29140,#29141,
#29142,#29143),(#29144,#29145,#29146,#29147,#29148,#29149,#29150,#29151,
#29152),(#29153,#29154,#29155,#29156,#29157,#29158,#29159,#29160,#29161),
(#29162,#29163,#29164,#29165,#29166,#29167,#29168,#29169,#29170)),
 .UNSPECIFIED.,.F.,.F.,.F.)
B_SPLINE_SURFACE_WITH_KNOTS((4,4),(3,2,2,2,3),(0.,1.),(0.,0.0714285714285714,
0.142857142857143,0.214285714285714,0.25),.UNSPECIFIED.)
GEOMETRIC_REPRESENTATION_ITEM()
RATIONAL_B_SPLINE_SURFACE(((1.,0.974927912181824,1.,0.974927912181824,1.,
0.974927912181824,1.,0.987463956090912,0.987463956090912),(0.833333333333332,
0.812439926818185,0.833333333333332,0.812439926818185,0.833333333333332,
0.812439926818185,0.833333333333332,0.822886630075758,0.822886630075758),
(0.833333333333332,0.812439926818185,0.833333333333332,0.812439926818185,
0.833333333333332,0.812439926818185,0.833333333333332,0.822886630075758,
0.822886630075758),(1.,0.974927912181824,1.,0.974927912181824,1.,0.974927912181824,
1.,0.987463956090912,0.987463956090912)))
REPRESENTATION_ITEM('')
SURFACE()
);
#445=(
BOUNDED_SURFACE()
B_SPLINE_SURFACE(3,2,((#29174,#29175,#29176,#29177,#29178,#29179,#29180,
#29181,#29182),(#29183,#29184,#29185,#29186,#29187,#29188,#29189,#29190,
#29191),(#29192,#29193,#29194,#29195,#29196,#29197,#29198,#29199,#29200),
(#29201,#29202,#29203,#29204,#29205,#29206,#29207,#29208,#29209)),
 .UNSPECIFIED.,.F.,.F.,.F.)
B_SPLINE_SURFACE_WITH_KNOTS((4,4),(3,2,2,2,3),(0.,1.),(0.,0.25,0.5,0.75,
1.),.UNSPECIFIED.)
GEOMETRIC_REPRESENTATION_ITEM()
RATIONAL_B_SPLINE_SURFACE(((1.,0.974927912181824,1.,0.974927912181824,1.,
0.974927912181824,1.,0.974927912181824,1.),(0.987189825241073,0.962438915249418,
0.987189825241073,0.962438915249418,0.987189825241073,0.962438915249418,
0.987189825241073,0.962438915249418,0.987189825241073),(0.987189825241073,
0.962438915249418,0.987189825241073,0.962438915249418,0.987189825241073,
0.962438915249418,0.987189825241073,0.962438915249418,0.987189825241073),
(1.,0.974927912181824,1.,0.974927912181824,1.,0.974927912181824,1.,0.974927912181824,
1.)))
REPRESENTATION_ITEM('')
SURFACE()
);
#446=(
BOUNDED_SURFACE()
B_SPLINE_SURFACE(3,2,((#29264,#29265,#29266,#29267,#29268,#29269,#29270,
#29271,#29272),(#29273,#29274,#29275,#29276,#29277,#29278,#29279,#29280,
#29281),(#29282,#29283,#29284,#29285,#29286,#29287,#29288,#29289,#29290),
(#29291,#29292,#29293,#29294,#29295,#29296,#29297,#29298,#29299)),
 .UNSPECIFIED.,.F.,.F.,.F.)
B_SPLINE_SURFACE_WITH_KNOTS((4,4),(3,2,2,2,3),(0.,1.),(0.,0.25,0.5,0.75,
1.),.UNSPECIFIED.)
GEOMETRIC_REPRESENTATION_ITEM()
RATIONAL_B_SPLINE_SURFACE(((1.,0.974927912181824,1.,0.974927912181824,1.,
0.974927912181824,1.,0.974927912181824,1.),(0.987189825241073,0.962438915249418,
0.987189825241073,0.962438915249418,0.987189825241073,0.962438915249418,
0.987189825241073,0.962438915249418,0.987189825241073),(0.987189825241073,
0.962438915249418,0.987189825241073,0.962438915249418,0.987189825241073,
0.962438915249418,0.987189825241073,0.962438915249418,0.987189825241073),
(1.,0.974927912181824,1.,0.974927912181824,1.,0.974927912181824,1.,0.974927912181824,
1.)))
REPRESENTATION_ITEM('')
SURFACE()
);
#447=(
BOUNDED_SURFACE()
B_SPLINE_SURFACE(3,2,((#29307,#29308,#29309,#29310,#29311,#29312,#29313,
#29314,#29315),(#29316,#29317,#29318,#29319,#29320,#29321,#29322,#29323,
#29324),(#29325,#29326,#29327,#29328,#29329,#29330,#29331,#29332,#29333),
(#29334,#29335,#29336,#29337,#29338,#29339,#29340,#29341,#29342)),
 .UNSPECIFIED.,.F.,.F.,.F.)
B_SPLINE_SURFACE_WITH_KNOTS((4,4),(3,2,2,2,3),(0.,1.),(0.,0.25,0.5,0.75,
1.),.UNSPECIFIED.)
GEOMETRIC_REPRESENTATION_ITEM()
RATIONAL_B_SPLINE_SURFACE(((1.,0.974927912181824,1.,0.974927912181824,1.,
0.974927912181824,1.,0.974927912181824,1.),(0.833333333333333,0.812439926818186,
0.833333333333333,0.812439926818186,0.833333333333333,0.812439926818186,
0.833333333333333,0.812439926818186,0.833333333333333),(0.833333333333333,
0.812439926818186,0.833333333333333,0.812439926818186,0.833333333333333,
0.812439926818186,0.833333333333333,0.812439926818186,0.833333333333333),
(1.,0.974927912181824,1.,0.974927912181824,1.,0.974927912181824,1.,0.974927912181824,
1.)))
REPRESENTATION_ITEM('')
SURFACE()
);
#448=(
BOUNDED_SURFACE()
B_SPLINE_SURFACE(3,2,((#29346,#29347,#29348,#29349,#29350,#29351,#29352,
#29353,#29354),(#29355,#29356,#29357,#29358,#29359,#29360,#29361,#29362,
#29363),(#29364,#29365,#29366,#29367,#29368,#29369,#29370,#29371,#29372),
(#29373,#29374,#29375,#29376,#29377,#29378,#29379,#29380,#29381)),
 .UNSPECIFIED.,.F.,.F.,.F.)
B_SPLINE_SURFACE_WITH_KNOTS((4,4),(3,2,2,2,3),(0.,1.),(0.,0.25,0.5,0.75,
1.),.UNSPECIFIED.)
GEOMETRIC_REPRESENTATION_ITEM()
RATIONAL_B_SPLINE_SURFACE(((1.,0.974927912181824,1.,0.974927912181824,1.,
0.974927912181824,1.,0.974927912181824,1.),(0.987189825241073,0.962438915249418,
0.987189825241073,0.962438915249418,0.987189825241073,0.962438915249418,
0.987189825241073,0.962438915249418,0.987189825241073),(0.987189825241073,
0.962438915249418,0.987189825241073,0.962438915249418,0.987189825241073,
0.962438915249418,0.987189825241073,0.962438915249418,0.987189825241073),
(1.,0.974927912181824,1.,0.974927912181824,1.,0.974927912181824,1.,0.974927912181824,
1.)))
REPRESENTATION_ITEM('')
SURFACE()
);
#449=(
BOUNDED_SURFACE()
B_SPLINE_SURFACE(3,2,((#29436,#29437,#29438,#29439,#29440,#29441,#29442,
#29443,#29444),(#29445,#29446,#29447,#29448,#29449,#29450,#29451,#29452,
#29453),(#29454,#29455,#29456,#29457,#29458,#29459,#29460,#29461,#29462),
(#29463,#29464,#29465,#29466,#29467,#29468,#29469,#29470,#29471)),
 .UNSPECIFIED.,.F.,.F.,.F.)
B_SPLINE_SURFACE_WITH_KNOTS((4,4),(3,2,2,2,3),(0.,1.),(0.,0.25,0.5,0.75,
1.),.UNSPECIFIED.)
GEOMETRIC_REPRESENTATION_ITEM()
RATIONAL_B_SPLINE_SURFACE(((1.,0.974927912181824,1.,0.974927912181824,1.,
0.974927912181824,1.,0.974927912181824,1.),(0.987189825241073,0.962438915249418,
0.987189825241073,0.962438915249418,0.987189825241073,0.962438915249418,
0.987189825241073,0.962438915249418,0.987189825241073),(0.987189825241073,
0.962438915249418,0.987189825241073,0.962438915249418,0.987189825241073,
0.962438915249418,0.987189825241073,0.962438915249418,0.987189825241073),
(1.,0.974927912181824,1.,0.974927912181824,1.,0.974927912181824,1.,0.974927912181824,
1.)))
REPRESENTATION_ITEM('')
SURFACE()
);
#450=(
BOUNDED_SURFACE()
B_SPLINE_SURFACE(3,2,((#29479,#29480,#29481,#29482,#29483,#29484,#29485,
#29486,#29487),(#29488,#29489,#29490,#29491,#29492,#29493,#29494,#29495,
#29496),(#29497,#29498,#29499,#29500,#29501,#29502,#29503,#29504,#29505),
(#29506,#29507,#29508,#29509,#29510,#29511,#29512,#29513,#29514)),
 .UNSPECIFIED.,.F.,.F.,.F.)
B_SPLINE_SURFACE_WITH_KNOTS((4,4),(3,2,2,2,3),(0.,1.),(0.,0.25,0.5,0.75,
1.),.UNSPECIFIED.)
GEOMETRIC_REPRESENTATION_ITEM()
RATIONAL_B_SPLINE_SURFACE(((1.,0.974927912181824,1.,0.974927912181824,1.,
0.974927912181824,1.,0.974927912181824,1.),(0.833333333333332,0.812439926818185,
0.833333333333332,0.812439926818185,0.833333333333332,0.812439926818185,
0.833333333333332,0.812439926818185,0.833333333333332),(0.833333333333332,
0.812439926818185,0.833333333333332,0.812439926818185,0.833333333333332,
0.812439926818185,0.833333333333332,0.812439926818185,0.833333333333332),
(1.,0.974927912181824,1.,0.974927912181824,1.,0.974927912181824,1.,0.974927912181824,
1.)))
REPRESENTATION_ITEM('')
SURFACE()
);
#451=(
BOUNDED_SURFACE()
B_SPLINE_SURFACE(3,2,((#29518,#29519,#29520,#29521,#29522,#29523,#29524,
#29525,#29526),(#29527,#29528,#29529,#29530,#29531,#29532,#29533,#29534,
#29535),(#29536,#29537,#29538,#29539,#29540,#29541,#29542,#29543,#29544),
(#29545,#29546,#29547,#29548,#29549,#29550,#29551,#29552,#29553)),
 .UNSPECIFIED.,.F.,.F.,.F.)
B_SPLINE_SURFACE_WITH_KNOTS((4,4),(3,2,2,2,3),(0.,1.),(0.,0.25,0.5,0.75,
1.),.UNSPECIFIED.)
GEOMETRIC_REPRESENTATION_ITEM()
RATIONAL_B_SPLINE_SURFACE(((1.,0.974927912181824,1.,0.974927912181824,1.,
0.974927912181824,1.,0.974927912181824,1.),(0.987189825241073,0.962438915249418,
0.987189825241073,0.962438915249418,0.987189825241073,0.962438915249418,
0.987189825241073,0.962438915249418,0.987189825241073),(0.987189825241073,
0.962438915249418,0.987189825241073,0.962438915249418,0.987189825241073,
0.962438915249418,0.987189825241073,0.962438915249418,0.987189825241073),
(1.,0.974927912181824,1.,0.974927912181824,1.,0.974927912181824,1.,0.974927912181824,
1.)))
REPRESENTATION_ITEM('')
SURFACE()
);
#452=(
BOUNDED_SURFACE()
B_SPLINE_SURFACE(3,2,((#29608,#29609,#29610,#29611,#29612,#29613,#29614,
#29615,#29616),(#29617,#29618,#29619,#29620,#29621,#29622,#29623,#29624,
#29625),(#29626,#29627,#29628,#29629,#29630,#29631,#29632,#29633,#29634),
(#29635,#29636,#29637,#29638,#29639,#29640,#29641,#29642,#29643)),
 .UNSPECIFIED.,.F.,.F.,.F.)
B_SPLINE_SURFACE_WITH_KNOTS((4,4),(3,2,2,2,3),(0.,1.),(0.,0.25,0.5,0.75,
1.),.UNSPECIFIED.)
GEOMETRIC_REPRESENTATION_ITEM()
RATIONAL_B_SPLINE_SURFACE(((1.,0.974927912181824,1.,0.974927912181824,1.,
0.974927912181824,1.,0.974927912181824,1.),(0.987189825241073,0.962438915249418,
0.987189825241073,0.962438915249418,0.987189825241073,0.962438915249418,
0.987189825241073,0.962438915249418,0.987189825241073),(0.987189825241073,
0.962438915249418,0.987189825241073,0.962438915249418,0.987189825241073,
0.962438915249418,0.987189825241073,0.962438915249418,0.987189825241073),
(1.,0.974927912181824,1.,0.974927912181824,1.,0.974927912181824,1.,0.974927912181824,
1.)))
REPRESENTATION_ITEM('')
SURFACE()
);
#453=(
BOUNDED_SURFACE()
B_SPLINE_SURFACE(3,2,((#29651,#29652,#29653,#29654,#29655,#29656,#29657,
#29658,#29659),(#29660,#29661,#29662,#29663,#29664,#29665,#29666,#29667,
#29668),(#29669,#29670,#29671,#29672,#29673,#29674,#29675,#29676,#29677),
(#29678,#29679,#29680,#29681,#29682,#29683,#29684,#29685,#29686)),
 .UNSPECIFIED.,.F.,.F.,.F.)
B_SPLINE_SURFACE_WITH_KNOTS((4,4),(3,2,2,2,3),(0.,1.),(0.,0.25,0.5,0.75,
1.),.UNSPECIFIED.)
GEOMETRIC_REPRESENTATION_ITEM()
RATIONAL_B_SPLINE_SURFACE(((1.,0.974927912181824,1.,0.974927912181824,1.,
0.974927912181824,1.,0.974927912181824,1.),(0.833333333333332,0.812439926818185,
0.833333333333332,0.812439926818185,0.833333333333332,0.812439926818185,
0.833333333333332,0.812439926818185,0.833333333333332),(0.833333333333332,
0.812439926818185,0.833333333333332,0.812439926818185,0.833333333333332,
0.812439926818185,0.833333333333332,0.812439926818185,0.833333333333332),
(1.,0.974927912181824,1.,0.974927912181824,1.,0.974927912181824,1.,0.974927912181824,
1.)))
REPRESENTATION_ITEM('')
SURFACE()
);
#454=(
BOUNDED_SURFACE()
B_SPLINE_SURFACE(3,2,((#29690,#29691,#29692,#29693,#29694,#29695,#29696,
#29697,#29698),(#29699,#29700,#29701,#29702,#29703,#29704,#29705,#29706,
#29707),(#29708,#29709,#29710,#29711,#29712,#29713,#29714,#29715,#29716),
(#29717,#29718,#29719,#29720,#29721,#29722,#29723,#29724,#29725)),
 .UNSPECIFIED.,.F.,.F.,.F.)
B_SPLINE_SURFACE_WITH_KNOTS((4,4),(3,2,2,2,3),(0.,1.),(0.,0.25,0.5,0.75,
1.),.UNSPECIFIED.)
GEOMETRIC_REPRESENTATION_ITEM()
RATIONAL_B_SPLINE_SURFACE(((1.,0.974927912181824,1.,0.974927912181824,1.,
0.974927912181824,1.,0.974927912181824,1.),(0.987189825241073,0.962438915249418,
0.987189825241073,0.962438915249418,0.987189825241073,0.962438915249418,
0.987189825241073,0.962438915249418,0.987189825241073),(0.987189825241073,
0.962438915249418,0.987189825241073,0.962438915249418,0.987189825241073,
0.962438915249418,0.987189825241073,0.962438915249418,0.987189825241073),
(1.,0.974927912181824,1.,0.974927912181824,1.,0.974927912181824,1.,0.974927912181824,
1.)))
REPRESENTATION_ITEM('')
SURFACE()
);
#455=(
BOUNDED_SURFACE()
B_SPLINE_SURFACE(3,2,((#29780,#29781,#29782,#29783,#29784,#29785,#29786,
#29787,#29788),(#29789,#29790,#29791,#29792,#29793,#29794,#29795,#29796,
#29797),(#29798,#29799,#29800,#29801,#29802,#29803,#29804,#29805,#29806),
(#29807,#29808,#29809,#29810,#29811,#29812,#29813,#29814,#29815)),
 .UNSPECIFIED.,.F.,.F.,.F.)
B_SPLINE_SURFACE_WITH_KNOTS((4,4),(3,2,2,2,3),(0.,1.),(0.,0.25,0.5,0.75,
1.),.UNSPECIFIED.)
GEOMETRIC_REPRESENTATION_ITEM()
RATIONAL_B_SPLINE_SURFACE(((1.,0.974927912181824,1.,0.974927912181824,1.,
0.974927912181824,1.,0.974927912181824,1.),(0.987189825241073,0.962438915249418,
0.987189825241073,0.962438915249418,0.987189825241073,0.962438915249418,
0.987189825241073,0.962438915249418,0.987189825241073),(0.987189825241073,
0.962438915249418,0.987189825241073,0.962438915249418,0.987189825241073,
0.962438915249418,0.987189825241073,0.962438915249418,0.987189825241073),
(1.,0.974927912181824,1.,0.974927912181824,1.,0.974927912181824,1.,0.974927912181824,
1.)))
REPRESENTATION_ITEM('')
SURFACE()
);
#456=(
BOUNDED_SURFACE()
B_SPLINE_SURFACE(3,2,((#29823,#29824,#29825,#29826,#29827,#29828,#29829,
#29830,#29831),(#29832,#29833,#29834,#29835,#29836,#29837,#29838,#29839,
#29840),(#29841,#29842,#29843,#29844,#29845,#29846,#29847,#29848,#29849),
(#29850,#29851,#29852,#29853,#29854,#29855,#29856,#29857,#29858)),
 .UNSPECIFIED.,.F.,.F.,.F.)
B_SPLINE_SURFACE_WITH_KNOTS((4,4),(3,2,2,2,3),(0.,1.),(0.,0.25,0.5,0.75,
1.),.UNSPECIFIED.)
GEOMETRIC_REPRESENTATION_ITEM()
RATIONAL_B_SPLINE_SURFACE(((1.,0.974927912181824,1.,0.974927912181824,1.,
0.974927912181824,1.,0.974927912181824,1.),(0.833333333333332,0.812439926818185,
0.833333333333332,0.812439926818185,0.833333333333332,0.812439926818185,
0.833333333333332,0.812439926818185,0.833333333333332),(0.833333333333332,
0.812439926818185,0.833333333333332,0.812439926818185,0.833333333333332,
0.812439926818185,0.833333333333332,0.812439926818185,0.833333333333332),
(1.,0.974927912181824,1.,0.974927912181824,1.,0.974927912181824,1.,0.974927912181824,
1.)))
REPRESENTATION_ITEM('')
SURFACE()
);
#457=(
BOUNDED_SURFACE()
B_SPLINE_SURFACE(3,2,((#29862,#29863,#29864,#29865,#29866,#29867,#29868,
#29869,#29870),(#29871,#29872,#29873,#29874,#29875,#29876,#29877,#29878,
#29879),(#29880,#29881,#29882,#29883,#29884,#29885,#29886,#29887,#29888),
(#29889,#29890,#29891,#29892,#29893,#29894,#29895,#29896,#29897)),
 .UNSPECIFIED.,.F.,.F.,.F.)
B_SPLINE_SURFACE_WITH_KNOTS((4,4),(3,2,2,2,3),(0.,1.),(0.,0.25,0.5,0.75,
1.),.UNSPECIFIED.)
GEOMETRIC_REPRESENTATION_ITEM()
RATIONAL_B_SPLINE_SURFACE(((1.,0.974927912181824,1.,0.974927912181824,1.,
0.974927912181824,1.,0.974927912181824,1.),(0.987189825241073,0.962438915249418,
0.987189825241073,0.962438915249418,0.987189825241073,0.962438915249418,
0.987189825241073,0.962438915249418,0.987189825241073),(0.987189825241073,
0.962438915249418,0.987189825241073,0.962438915249418,0.987189825241073,
0.962438915249418,0.987189825241073,0.962438915249418,0.987189825241073),
(1.,0.974927912181824,1.,0.974927912181824,1.,0.974927912181824,1.,0.974927912181824,
1.)))
REPRESENTATION_ITEM('')
SURFACE()
);
#458=(
BOUNDED_SURFACE()
B_SPLINE_SURFACE(3,2,((#29952,#29953,#29954,#29955,#29956,#29957,#29958,
#29959,#29960),(#29961,#29962,#29963,#29964,#29965,#29966,#29967,#29968,
#29969),(#29970,#29971,#29972,#29973,#29974,#29975,#29976,#29977,#29978),
(#29979,#29980,#29981,#29982,#29983,#29984,#29985,#29986,#29987)),
 .UNSPECIFIED.,.F.,.F.,.F.)
B_SPLINE_SURFACE_WITH_KNOTS((4,4),(3,2,2,2,3),(0.,1.),(0.,0.25,0.5,0.75,
1.),.UNSPECIFIED.)
GEOMETRIC_REPRESENTATION_ITEM()
RATIONAL_B_SPLINE_SURFACE(((1.,0.974927912181824,1.,0.974927912181824,1.,
0.974927912181824,1.,0.974927912181824,1.),(0.987189825241073,0.962438915249418,
0.987189825241073,0.962438915249418,0.987189825241073,0.962438915249418,
0.987189825241073,0.962438915249418,0.987189825241073),(0.987189825241073,
0.962438915249418,0.987189825241073,0.962438915249418,0.987189825241073,
0.962438915249418,0.987189825241073,0.962438915249418,0.987189825241073),
(1.,0.974927912181824,1.,0.974927912181824,1.,0.974927912181824,1.,0.974927912181824,
1.)))
REPRESENTATION_ITEM('')
SURFACE()
);
#459=(
BOUNDED_SURFACE()
B_SPLINE_SURFACE(3,2,((#29995,#29996,#29997,#29998,#29999,#30000,#30001,
#30002,#30003),(#30004,#30005,#30006,#30007,#30008,#30009,#30010,#30011,
#30012),(#30013,#30014,#30015,#30016,#30017,#30018,#30019,#30020,#30021),
(#30022,#30023,#30024,#30025,#30026,#30027,#30028,#30029,#30030)),
 .UNSPECIFIED.,.F.,.F.,.F.)
B_SPLINE_SURFACE_WITH_KNOTS((4,4),(3,2,2,2,3),(0.,1.),(0.,0.25,0.5,0.75,
1.),.UNSPECIFIED.)
GEOMETRIC_REPRESENTATION_ITEM()
RATIONAL_B_SPLINE_SURFACE(((1.,0.974927912181824,1.,0.974927912181824,1.,
0.974927912181824,1.,0.974927912181824,1.),(0.833333333333333,0.812439926818186,
0.833333333333333,0.812439926818186,0.833333333333333,0.812439926818186,
0.833333333333333,0.812439926818186,0.833333333333333),(0.833333333333333,
0.812439926818186,0.833333333333333,0.812439926818186,0.833333333333333,
0.812439926818186,0.833333333333333,0.812439926818186,0.833333333333333),
(1.,0.974927912181824,1.,0.974927912181824,1.,0.974927912181824,1.,0.974927912181824,
1.)))
REPRESENTATION_ITEM('')
SURFACE()
);
#460=(
BOUNDED_SURFACE()
B_SPLINE_SURFACE(3,2,((#30034,#30035,#30036,#30037,#30038,#30039,#30040,
#30041,#30042),(#30043,#30044,#30045,#30046,#30047,#30048,#30049,#30050,
#30051),(#30052,#30053,#30054,#30055,#30056,#30057,#30058,#30059,#30060),
(#30061,#30062,#30063,#30064,#30065,#30066,#30067,#30068,#30069)),
 .UNSPECIFIED.,.F.,.F.,.F.)
B_SPLINE_SURFACE_WITH_KNOTS((4,4),(3,2,2,2,3),(0.,1.),(0.,0.25,0.5,0.75,
1.),.UNSPECIFIED.)
GEOMETRIC_REPRESENTATION_ITEM()
RATIONAL_B_SPLINE_SURFACE(((1.,0.974927912181824,1.,0.974927912181824,1.,
0.974927912181824,1.,0.974927912181824,1.),(0.987189825241073,0.962438915249418,
0.987189825241073,0.962438915249418,0.987189825241073,0.962438915249418,
0.987189825241073,0.962438915249418,0.987189825241073),(0.987189825241073,
0.962438915249418,0.987189825241073,0.962438915249418,0.987189825241073,
0.962438915249418,0.987189825241073,0.962438915249418,0.987189825241073),
(1.,0.974927912181824,1.,0.974927912181824,1.,0.974927912181824,1.,0.974927912181824,
1.)))
REPRESENTATION_ITEM('')
SURFACE()
);
#461=(
BOUNDED_SURFACE()
B_SPLINE_SURFACE(3,2,((#30077,#30078,#30079,#30080,#30081,#30082,#30083,
#30084,#30085),(#30086,#30087,#30088,#30089,#30090,#30091,#30092,#30093,
#30094),(#30095,#30096,#30097,#30098,#30099,#30100,#30101,#30102,#30103),
(#30104,#30105,#30106,#30107,#30108,#30109,#30110,#30111,#30112)),
 .UNSPECIFIED.,.F.,.F.,.F.)
B_SPLINE_SURFACE_WITH_KNOTS((4,4),(3,2,2,2,3),(0.,1.),(0.,0.25,0.5,0.75,
1.),.UNSPECIFIED.)
GEOMETRIC_REPRESENTATION_ITEM()
RATIONAL_B_SPLINE_SURFACE(((1.,0.974927912181824,1.,0.974927912181824,1.,
0.974927912181824,1.,0.974927912181824,1.),(0.987189825241073,0.962438915249418,
0.987189825241073,0.962438915249418,0.987189825241073,0.962438915249418,
0.987189825241073,0.962438915249418,0.987189825241073),(0.987189825241073,
0.962438915249418,0.987189825241073,0.962438915249418,0.987189825241073,
0.962438915249418,0.987189825241073,0.962438915249418,0.987189825241073),
(1.,0.974927912181824,1.,0.974927912181824,1.,0.974927912181824,1.,0.974927912181824,
1.)))
REPRESENTATION_ITEM('')
SURFACE()
);
#462=(
BOUNDED_SURFACE()
B_SPLINE_SURFACE(3,2,((#30120,#30121,#30122,#30123,#30124,#30125,#30126,
#30127,#30128),(#30129,#30130,#30131,#30132,#30133,#30134,#30135,#30136,
#30137),(#30138,#30139,#30140,#30141,#30142,#30143,#30144,#30145,#30146),
(#30147,#30148,#30149,#30150,#30151,#30152,#30153,#30154,#30155)),
 .UNSPECIFIED.,.F.,.F.,.F.)
B_SPLINE_SURFACE_WITH_KNOTS((4,4),(3,2,2,2,3),(0.,1.),(0.,0.25,0.5,0.75,
1.),.UNSPECIFIED.)
GEOMETRIC_REPRESENTATION_ITEM()
RATIONAL_B_SPLINE_SURFACE(((1.,0.974927912181824,1.,0.974927912181824,1.,
0.974927912181824,1.,0.974927912181824,1.),(0.833333333333332,0.812439926818185,
0.833333333333332,0.812439926818185,0.833333333333332,0.812439926818185,
0.833333333333332,0.812439926818185,0.833333333333332),(0.833333333333332,
0.812439926818185,0.833333333333332,0.812439926818185,0.833333333333332,
0.812439926818185,0.833333333333332,0.812439926818185,0.833333333333332),
(1.,0.974927912181824,1.,0.974927912181824,1.,0.974927912181824,1.,0.974927912181824,
1.)))
REPRESENTATION_ITEM('')
SURFACE()
);
#463=(
BOUNDED_SURFACE()
B_SPLINE_SURFACE(3,3,((#30159,#30160,#30161,#30162,#30163,#30164,#30165,
#30166,#30167,#30168,#30169,#30170),(#30171,#30172,#30173,#30174,#30175,
#30176,#30177,#30178,#30179,#30180,#30181,#30182),(#30183,#30184,#30185,
#30186,#30187,#30188,#30189,#30190,#30191,#30192,#30193,#30194),(#30195,
#30196,#30197,#30198,#30199,#30200,#30201,#30202,#30203,#30204,#30205,#30206)),
 .UNSPECIFIED.,.F.,.F.,.F.)
B_SPLINE_SURFACE_WITH_KNOTS((4,4),(4,2,2,2,2,4),(0.,1.),(0.,0.0783698352504338,
0.308777376437326,0.539184917624882,0.769592458812441,1.),.UNSPECIFIED.)
GEOMETRIC_REPRESENTATION_ITEM()
RATIONAL_B_SPLINE_SURFACE(((1.,1.,1.,1.,1.,1.,1.,1.,1.,1.,1.,1.),(0.833333333333332,
0.833333333333332,0.833333333333332,0.833333333333332,0.833333333333332,
0.833333333333332,0.833333333333332,0.833333333333332,0.833333333333332,
0.833333333333332,0.833333333333332,0.833333333333332),(0.833333333333332,
0.833333333333332,0.833333333333332,0.833333333333332,0.833333333333332,
0.833333333333332,0.833333333333332,0.833333333333332,0.833333333333332,
0.833333333333332,0.833333333333332,0.833333333333332),(1.,1.,1.,1.,1.,
1.,1.,1.,1.,1.,1.,1.)))
REPRESENTATION_ITEM('')
SURFACE()
);
#464=(
BOUNDED_SURFACE()
B_SPLINE_SURFACE(3,3,((#30223,#30224,#30225,#30226,#30227,#30228,#30229,
#30230,#30231,#30232,#30233,#30234),(#30235,#30236,#30237,#30238,#30239,
#30240,#30241,#30242,#30243,#30244,#30245,#30246),(#30247,#30248,#30249,
#30250,#30251,#30252,#30253,#30254,#30255,#30256,#30257,#30258),(#30259,
#30260,#30261,#30262,#30263,#30264,#30265,#30266,#30267,#30268,#30269,#30270)),
 .UNSPECIFIED.,.F.,.F.,.F.)
B_SPLINE_SURFACE_WITH_KNOTS((4,4),(4,2,2,2,2,4),(0.,1.),(0.,0.0783698352504338,
0.308777376437326,0.539184917624882,0.769592458812441,1.),.UNSPECIFIED.)
GEOMETRIC_REPRESENTATION_ITEM()
RATIONAL_B_SPLINE_SURFACE(((1.,1.,1.,1.,1.,1.,1.,1.,1.,1.,1.,1.),(0.987189825241073,
0.987189825241073,0.987189825241073,0.987189825241073,0.987189825241073,
0.987189825241073,0.987189825241073,0.987189825241073,0.987189825241073,
0.987189825241073,0.987189825241073,0.987189825241073),(0.987189825241073,
0.987189825241073,0.987189825241073,0.987189825241073,0.987189825241073,
0.987189825241073,0.987189825241073,0.987189825241073,0.987189825241073,
0.987189825241073,0.987189825241073,0.987189825241073),(1.,1.,1.,1.,1.,
1.,1.,1.,1.,1.,1.,1.)))
REPRESENTATION_ITEM('')
SURFACE()
);
#465=(
BOUNDED_SURFACE()
B_SPLINE_SURFACE(3,3,((#30271,#30272,#30273,#30274,#30275,#30276,#30277,
#30278,#30279,#30280,#30281,#30282),(#30283,#30284,#30285,#30286,#30287,
#30288,#30289,#30290,#30291,#30292,#30293,#30294),(#30295,#30296,#30297,
#30298,#30299,#30300,#30301,#30302,#30303,#30304,#30305,#30306),(#30307,
#30308,#30309,#30310,#30311,#30312,#30313,#30314,#30315,#30316,#30317,#30318)),
 .UNSPECIFIED.,.F.,.F.,.F.)
B_SPLINE_SURFACE_WITH_KNOTS((4,4),(4,2,2,2,2,4),(0.,1.),(0.,0.0783698352504338,
0.308777376437326,0.539184917624882,0.769592458812441,1.),.UNSPECIFIED.)
GEOMETRIC_REPRESENTATION_ITEM()
RATIONAL_B_SPLINE_SURFACE(((1.,1.,1.,1.,1.,1.,1.,1.,1.,1.,1.,1.),(0.987189825241073,
0.987189825241073,0.987189825241073,0.987189825241073,0.987189825241073,
0.987189825241073,0.987189825241073,0.987189825241073,0.987189825241073,
0.987189825241073,0.987189825241073,0.987189825241073),(0.987189825241073,
0.987189825241073,0.987189825241073,0.987189825241073,0.987189825241073,
0.987189825241073,0.987189825241073,0.987189825241073,0.987189825241073,
0.987189825241073,0.987189825241073,0.987189825241073),(1.,1.,1.,1.,1.,
1.,1.,1.,1.,1.,1.,1.)))
REPRESENTATION_ITEM('')
SURFACE()
);
#466=(
BOUNDED_SURFACE()
B_SPLINE_SURFACE(3,3,((#30319,#30320,#30321,#30322,#30323,#30324,#30325,
#30326,#30327,#30328,#30329,#30330),(#30331,#30332,#30333,#30334,#30335,
#30336,#30337,#30338,#30339,#30340,#30341,#30342),(#30343,#30344,#30345,
#30346,#30347,#30348,#30349,#30350,#30351,#30352,#30353,#30354),(#30355,
#30356,#30357,#30358,#30359,#30360,#30361,#30362,#30363,#30364,#30365,#30366)),
 .UNSPECIFIED.,.F.,.F.,.F.)
B_SPLINE_SURFACE_WITH_KNOTS((4,4),(4,2,2,2,2,4),(0.,1.),(0.,0.0783698388401176,
0.308777379129589,0.539184919419725,0.769592459709862,1.),.UNSPECIFIED.)
GEOMETRIC_REPRESENTATION_ITEM()
RATIONAL_B_SPLINE_SURFACE(((1.,1.,1.,1.,1.,1.,1.,1.,1.,1.,1.,1.),(0.833333333333333,
0.833333333333333,0.833333333333333,0.833333333333333,0.833333333333333,
0.833333333333333,0.833333333333333,0.833333333333333,0.833333333333333,
0.833333333333333,0.833333333333333,0.833333333333333),(0.833333333333333,
0.833333333333333,0.833333333333333,0.833333333333333,0.833333333333333,
0.833333333333333,0.833333333333333,0.833333333333333,0.833333333333333,
0.833333333333333,0.833333333333333,0.833333333333333),(1.,1.,1.,1.,1.,
1.,1.,1.,1.,1.,1.,1.)))
REPRESENTATION_ITEM('')
SURFACE()
);
#467=(
BOUNDED_SURFACE()
B_SPLINE_SURFACE(3,3,((#30383,#30384,#30385,#30386,#30387,#30388,#30389,
#30390,#30391,#30392,#30393,#30394),(#30395,#30396,#30397,#30398,#30399,
#30400,#30401,#30402,#30403,#30404,#30405,#30406),(#30407,#30408,#30409,
#30410,#30411,#30412,#30413,#30414,#30415,#30416,#30417,#30418),(#30419,
#30420,#30421,#30422,#30423,#30424,#30425,#30426,#30427,#30428,#30429,#30430)),
 .UNSPECIFIED.,.F.,.F.,.F.)
B_SPLINE_SURFACE_WITH_KNOTS((4,4),(4,2,2,2,2,4),(0.,1.),(0.,0.0783698388401176,
0.308777379129589,0.539184919419725,0.769592459709862,1.),.UNSPECIFIED.)
GEOMETRIC_REPRESENTATION_ITEM()
RATIONAL_B_SPLINE_SURFACE(((1.,1.,1.,1.,1.,1.,1.,1.,1.,1.,1.,1.),(0.987189825241073,
0.987189825241073,0.987189825241073,0.987189825241073,0.987189825241073,
0.987189825241073,0.987189825241073,0.987189825241073,0.987189825241073,
0.987189825241073,0.987189825241073,0.987189825241073),(0.987189825241073,
0.987189825241073,0.987189825241073,0.987189825241073,0.987189825241073,
0.987189825241073,0.987189825241073,0.987189825241073,0.987189825241073,
0.987189825241073,0.987189825241073,0.987189825241073),(1.,1.,1.,1.,1.,
1.,1.,1.,1.,1.,1.,1.)))
REPRESENTATION_ITEM('')
SURFACE()
);
#468=(
BOUNDED_SURFACE()
B_SPLINE_SURFACE(3,3,((#30431,#30432,#30433,#30434,#30435,#30436,#30437,
#30438,#30439,#30440,#30441,#30442),(#30443,#30444,#30445,#30446,#30447,
#30448,#30449,#30450,#30451,#30452,#30453,#30454),(#30455,#30456,#30457,
#30458,#30459,#30460,#30461,#30462,#30463,#30464,#30465,#30466),(#30467,
#30468,#30469,#30470,#30471,#30472,#30473,#30474,#30475,#30476,#30477,#30478)),
 .UNSPECIFIED.,.F.,.F.,.F.)
B_SPLINE_SURFACE_WITH_KNOTS((4,4),(4,2,2,2,2,4),(0.,1.),(0.,0.0783698388401176,
0.308777379129589,0.539184919419725,0.769592459709862,1.),.UNSPECIFIED.)
GEOMETRIC_REPRESENTATION_ITEM()
RATIONAL_B_SPLINE_SURFACE(((1.,1.,1.,1.,1.,1.,1.,1.,1.,1.,1.,1.),(0.987189825241073,
0.987189825241073,0.987189825241073,0.987189825241073,0.987189825241073,
0.987189825241073,0.987189825241073,0.987189825241073,0.987189825241073,
0.987189825241073,0.987189825241073,0.987189825241073),(0.987189825241073,
0.987189825241073,0.987189825241073,0.987189825241073,0.987189825241073,
0.987189825241073,0.987189825241073,0.987189825241073,0.987189825241073,
0.987189825241073,0.987189825241073,0.987189825241073),(1.,1.,1.,1.,1.,
1.,1.,1.,1.,1.,1.,1.)))
REPRESENTATION_ITEM('')
SURFACE()
);
#469=(
BOUNDED_SURFACE()
B_SPLINE_SURFACE(3,3,((#30479,#30480,#30481,#30482,#30483,#30484,#30485,
#30486,#30487,#30488,#30489,#30490,#30491,#30492),(#30493,#30494,#30495,
#30496,#30497,#30498,#30499,#30500,#30501,#30502,#30503,#30504,#30505,#30506),
(#30507,#30508,#30509,#30510,#30511,#30512,#30513,#30514,#30515,#30516,
#30517,#30518,#30519,#30520),(#30521,#30522,#30523,#30524,#30525,#30526,
#30527,#30528,#30529,#30530,#30531,#30532,#30533,#30534)),.UNSPECIFIED.,
 .F.,.F.,.F.)
B_SPLINE_SURFACE_WITH_KNOTS((4,4),(4,2,2,2,2,2,4),(0.,1.),(0.,0.0183879322611553,
0.0783698437311047,0.308777382797829,0.539184921865218,0.769592460932609,
1.),.UNSPECIFIED.)
GEOMETRIC_REPRESENTATION_ITEM()
RATIONAL_B_SPLINE_SURFACE(((1.,1.,1.,1.,1.,1.,1.,1.,1.,1.,1.,1.,1.,1.),
(0.833333333333331,0.833333333333331,0.833333333333331,0.833333333333331,
0.833333333333331,0.833333333333331,0.833333333333331,0.833333333333331,
0.833333333333331,0.833333333333331,0.833333333333331,0.833333333333331,
0.833333333333331,0.833333333333331),(0.833333333333331,0.833333333333331,
0.833333333333331,0.833333333333331,0.833333333333331,0.833333333333331,
0.833333333333331,0.833333333333331,0.833333333333331,0.833333333333331,
0.833333333333331,0.833333333333331,0.833333333333331,0.833333333333331),
(1.,1.,1.,1.,1.,1.,1.,1.,1.,1.,1.,1.,1.,1.)))
REPRESENTATION_ITEM('')
SURFACE()
);
#470=(
BOUNDED_SURFACE()
B_SPLINE_SURFACE(3,3,((#30553,#30554,#30555,#30556,#30557,#30558,#30559,
#30560,#30561,#30562,#30563,#30564,#30565,#30566),(#30567,#30568,#30569,
#30570,#30571,#30572,#30573,#30574,#30575,#30576,#30577,#30578,#30579,#30580),
(#30581,#30582,#30583,#30584,#30585,#30586,#30587,#30588,#30589,#30590,
#30591,#30592,#30593,#30594),(#30595,#30596,#30597,#30598,#30599,#30600,
#30601,#30602,#30603,#30604,#30605,#30606,#30607,#30608)),.UNSPECIFIED.,
 .F.,.F.,.F.)
B_SPLINE_SURFACE_WITH_KNOTS((4,4),(4,2,2,2,2,2,4),(0.,1.),(0.,0.0183879322611553,
0.0783698437311047,0.308777382797829,0.539184921865218,0.769592460932609,
1.),.UNSPECIFIED.)
GEOMETRIC_REPRESENTATION_ITEM()
RATIONAL_B_SPLINE_SURFACE(((1.,1.,1.,1.,1.,1.,1.,1.,1.,1.,1.,1.,1.,1.),
(0.987189825241073,0.987189825241073,0.987189825241073,0.987189825241073,
0.987189825241073,0.987189825241073,0.987189825241073,0.987189825241073,
0.987189825241073,0.987189825241073,0.987189825241073,0.987189825241073,
0.987189825241073,0.987189825241073),(0.987189825241073,0.987189825241073,
0.987189825241073,0.987189825241073,0.987189825241073,0.987189825241073,
0.987189825241073,0.987189825241073,0.987189825241073,0.987189825241073,
0.987189825241073,0.987189825241073,0.987189825241073,0.987189825241073),
(1.,1.,1.,1.,1.,1.,1.,1.,1.,1.,1.,1.,1.,1.)))
REPRESENTATION_ITEM('')
SURFACE()
);
#471=(
BOUNDED_SURFACE()
B_SPLINE_SURFACE(3,3,((#30609,#30610,#30611,#30612,#30613,#30614,#30615,
#30616,#30617,#30618,#30619,#30620,#30621,#30622),(#30623,#30624,#30625,
#30626,#30627,#30628,#30629,#30630,#30631,#30632,#30633,#30634,#30635,#30636),
(#30637,#30638,#30639,#30640,#30641,#30642,#30643,#30644,#30645,#30646,
#30647,#30648,#30649,#30650),(#30651,#30652,#30653,#30654,#30655,#30656,
#30657,#30658,#30659,#30660,#30661,#30662,#30663,#30664)),.UNSPECIFIED.,
 .F.,.F.,.F.)
B_SPLINE_SURFACE_WITH_KNOTS((4,4),(4,2,2,2,2,2,4),(0.,1.),(0.,0.0183879322611553,
0.0783698437311047,0.308777382797829,0.539184921865218,0.769592460932609,
1.),.UNSPECIFIED.)
GEOMETRIC_REPRESENTATION_ITEM()
RATIONAL_B_SPLINE_SURFACE(((1.,1.,1.,1.,1.,1.,1.,1.,1.,1.,1.,1.,1.,1.),
(0.987189825241073,0.987189825241073,0.987189825241073,0.987189825241073,
0.987189825241073,0.987189825241073,0.987189825241073,0.987189825241073,
0.987189825241073,0.987189825241073,0.987189825241073,0.987189825241073,
0.987189825241073,0.987189825241073),(0.987189825241073,0.987189825241073,
0.987189825241073,0.987189825241073,0.987189825241073,0.987189825241073,
0.987189825241073,0.987189825241073,0.987189825241073,0.987189825241073,
0.987189825241073,0.987189825241073,0.987189825241073,0.987189825241073),
(1.,1.,1.,1.,1.,1.,1.,1.,1.,1.,1.,1.,1.,1.)))
REPRESENTATION_ITEM('')
SURFACE()
);
#472=(
BOUNDED_SURFACE()
B_SPLINE_SURFACE(3,3,((#30665,#30666,#30667,#30668,#30669,#30670,#30671,
#30672,#30673,#30674,#30675,#30676),(#30677,#30678,#30679,#30680,#30681,
#30682,#30683,#30684,#30685,#30686,#30687,#30688),(#30689,#30690,#30691,
#30692,#30693,#30694,#30695,#30696,#30697,#30698,#30699,#30700),(#30701,
#30702,#30703,#30704,#30705,#30706,#30707,#30708,#30709,#30710,#30711,#30712)),
 .UNSPECIFIED.,.F.,.F.,.F.)
B_SPLINE_SURFACE_WITH_KNOTS((4,4),(4,2,2,2,2,4),(0.,1.),(0.,0.0783698481609191,
0.30877738612019,0.539184924080125,0.769592462040062,1.),.UNSPECIFIED.)
GEOMETRIC_REPRESENTATION_ITEM()
RATIONAL_B_SPLINE_SURFACE(((1.,1.,1.,1.,1.,1.,1.,1.,1.,1.,1.,1.),(0.833333333333333,
0.833333333333333,0.833333333333333,0.833333333333333,0.833333333333333,
0.833333333333333,0.833333333333333,0.833333333333333,0.833333333333333,
0.833333333333333,0.833333333333333,0.833333333333333),(0.833333333333333,
0.833333333333333,0.833333333333333,0.833333333333333,0.833333333333333,
0.833333333333333,0.833333333333333,0.833333333333333,0.833333333333333,
0.833333333333333,0.833333333333333,0.833333333333333),(1.,1.,1.,1.,1.,
1.,1.,1.,1.,1.,1.,1.)))
REPRESENTATION_ITEM('')
SURFACE()
);
#473=(
BOUNDED_SURFACE()
B_SPLINE_SURFACE(3,3,((#30729,#30730,#30731,#30732,#30733,#30734,#30735,
#30736,#30737,#30738,#30739,#30740),(#30741,#30742,#30743,#30744,#30745,
#30746,#30747,#30748,#30749,#30750,#30751,#30752),(#30753,#30754,#30755,
#30756,#30757,#30758,#30759,#30760,#30761,#30762,#30763,#30764),(#30765,
#30766,#30767,#30768,#30769,#30770,#30771,#30772,#30773,#30774,#30775,#30776)),
 .UNSPECIFIED.,.F.,.F.,.F.)
B_SPLINE_SURFACE_WITH_KNOTS((4,4),(4,2,2,2,2,4),(0.,1.),(0.,0.0783698481609191,
0.30877738612019,0.539184924080125,0.769592462040062,1.),.UNSPECIFIED.)
GEOMETRIC_REPRESENTATION_ITEM()
RATIONAL_B_SPLINE_SURFACE(((1.,1.,1.,1.,1.,1.,1.,1.,1.,1.,1.,1.),(0.987189825241073,
0.987189825241073,0.987189825241073,0.987189825241073,0.987189825241073,
0.987189825241073,0.987189825241073,0.987189825241073,0.987189825241073,
0.987189825241073,0.987189825241073,0.987189825241073),(0.987189825241073,
0.987189825241073,0.987189825241073,0.987189825241073,0.987189825241073,
0.987189825241073,0.987189825241073,0.987189825241073,0.987189825241073,
0.987189825241073,0.987189825241073,0.987189825241073),(1.,1.,1.,1.,1.,
1.,1.,1.,1.,1.,1.,1.)))
REPRESENTATION_ITEM('')
SURFACE()
);
#474=(
BOUNDED_SURFACE()
B_SPLINE_SURFACE(3,3,((#30777,#30778,#30779,#30780,#30781,#30782,#30783,
#30784,#30785,#30786,#30787,#30788),(#30789,#30790,#30791,#30792,#30793,
#30794,#30795,#30796,#30797,#30798,#30799,#30800),(#30801,#30802,#30803,
#30804,#30805,#30806,#30807,#30808,#30809,#30810,#30811,#30812),(#30813,
#30814,#30815,#30816,#30817,#30818,#30819,#30820,#30821,#30822,#30823,#30824)),
 .UNSPECIFIED.,.F.,.F.,.F.)
B_SPLINE_SURFACE_WITH_KNOTS((4,4),(4,2,2,2,2,4),(0.,1.),(0.,0.0783698481609191,
0.30877738612019,0.539184924080125,0.769592462040062,1.),.UNSPECIFIED.)
GEOMETRIC_REPRESENTATION_ITEM()
RATIONAL_B_SPLINE_SURFACE(((1.,1.,1.,1.,1.,1.,1.,1.,1.,1.,1.,1.),(0.987189825241073,
0.987189825241073,0.987189825241073,0.987189825241073,0.987189825241073,
0.987189825241073,0.987189825241073,0.987189825241073,0.987189825241073,
0.987189825241073,0.987189825241073,0.987189825241073),(0.987189825241073,
0.987189825241073,0.987189825241073,0.987189825241073,0.987189825241073,
0.987189825241073,0.987189825241073,0.987189825241073,0.987189825241073,
0.987189825241073,0.987189825241073,0.987189825241073),(1.,1.,1.,1.,1.,
1.,1.,1.,1.,1.,1.,1.)))
REPRESENTATION_ITEM('')
SURFACE()
);
#475=(
BOUNDED_SURFACE()
B_SPLINE_SURFACE(3,3,((#30825,#30826,#30827,#30828,#30829,#30830,#30831,
#30832,#30833,#30834,#30835,#30836),(#30837,#30838,#30839,#30840,#30841,
#30842,#30843,#30844,#30845,#30846,#30847,#30848),(#30849,#30850,#30851,
#30852,#30853,#30854,#30855,#30856,#30857,#30858,#30859,#30860),(#30861,
#30862,#30863,#30864,#30865,#30866,#30867,#30868,#30869,#30870,#30871,#30872)),
 .UNSPECIFIED.,.F.,.F.,.F.)
B_SPLINE_SURFACE_WITH_KNOTS((4,4),(4,2,2,2,2,4),(0.,1.),(0.,0.0783698504851113,
0.308777387863334,0.539184925242222,0.769592462621111,1.),.UNSPECIFIED.)
GEOMETRIC_REPRESENTATION_ITEM()
RATIONAL_B_SPLINE_SURFACE(((1.,1.,1.,1.,1.,1.,1.,1.,1.,1.,1.,1.),(0.833333333333332,
0.833333333333332,0.833333333333332,0.833333333333332,0.833333333333332,
0.833333333333332,0.833333333333332,0.833333333333332,0.833333333333332,
0.833333333333332,0.833333333333332,0.833333333333332),(0.833333333333332,
0.833333333333332,0.833333333333332,0.833333333333332,0.833333333333332,
0.833333333333332,0.833333333333332,0.833333333333332,0.833333333333332,
0.833333333333332,0.833333333333332,0.833333333333332),(1.,1.,1.,1.,1.,
1.,1.,1.,1.,1.,1.,1.)))
REPRESENTATION_ITEM('')
SURFACE()
);
#476=(
BOUNDED_SURFACE()
B_SPLINE_SURFACE(3,3,((#30889,#30890,#30891,#30892,#30893,#30894,#30895,
#30896,#30897,#30898,#30899,#30900),(#30901,#30902,#30903,#30904,#30905,
#30906,#30907,#30908,#30909,#30910,#30911,#30912),(#30913,#30914,#30915,
#30916,#30917,#30918,#30919,#30920,#30921,#30922,#30923,#30924),(#30925,
#30926,#30927,#30928,#30929,#30930,#30931,#30932,#30933,#30934,#30935,#30936)),
 .UNSPECIFIED.,.F.,.F.,.F.)
B_SPLINE_SURFACE_WITH_KNOTS((4,4),(4,2,2,2,2,4),(0.,1.),(0.,0.0783698504851113,
0.308777387863334,0.539184925242222,0.769592462621111,1.),.UNSPECIFIED.)
GEOMETRIC_REPRESENTATION_ITEM()
RATIONAL_B_SPLINE_SURFACE(((1.,1.,1.,1.,1.,1.,1.,1.,1.,1.,1.,1.),(0.987189825241073,
0.987189825241073,0.987189825241073,0.987189825241073,0.987189825241073,
0.987189825241073,0.987189825241073,0.987189825241073,0.987189825241073,
0.987189825241073,0.987189825241073,0.987189825241073),(0.987189825241073,
0.987189825241073,0.987189825241073,0.987189825241073,0.987189825241073,
0.987189825241073,0.987189825241073,0.987189825241073,0.987189825241073,
0.987189825241073,0.987189825241073,0.987189825241073),(1.,1.,1.,1.,1.,
1.,1.,1.,1.,1.,1.,1.)))
REPRESENTATION_ITEM('')
SURFACE()
);
#477=(
BOUNDED_SURFACE()
B_SPLINE_SURFACE(3,3,((#30937,#30938,#30939,#30940,#30941,#30942,#30943,
#30944,#30945,#30946,#30947,#30948),(#30949,#30950,#30951,#30952,#30953,
#30954,#30955,#30956,#30957,#30958,#30959,#30960),(#30961,#30962,#30963,
#30964,#30965,#30966,#30967,#30968,#30969,#30970,#30971,#30972),(#30973,
#30974,#30975,#30976,#30977,#30978,#30979,#30980,#30981,#30982,#30983,#30984)),
 .UNSPECIFIED.,.F.,.F.,.F.)
B_SPLINE_SURFACE_WITH_KNOTS((4,4),(4,2,2,2,2,4),(0.,1.),(0.,0.0783698504851113,
0.308777387863334,0.539184925242222,0.769592462621111,1.),.UNSPECIFIED.)
GEOMETRIC_REPRESENTATION_ITEM()
RATIONAL_B_SPLINE_SURFACE(((1.,1.,1.,1.,1.,1.,1.,1.,1.,1.,1.,1.),(0.987189825241073,
0.987189825241073,0.987189825241073,0.987189825241073,0.987189825241073,
0.987189825241073,0.987189825241073,0.987189825241073,0.987189825241073,
0.987189825241073,0.987189825241073,0.987189825241073),(0.987189825241073,
0.987189825241073,0.987189825241073,0.987189825241073,0.987189825241073,
0.987189825241073,0.987189825241073,0.987189825241073,0.987189825241073,
0.987189825241073,0.987189825241073,0.987189825241073),(1.,1.,1.,1.,1.,
1.,1.,1.,1.,1.,1.,1.)))
REPRESENTATION_ITEM('')
SURFACE()
);
#478=(
BOUNDED_SURFACE()
B_SPLINE_SURFACE(3,3,((#30985,#30986,#30987,#30988,#30989,#30990,#30991,
#30992,#30993,#30994,#30995,#30996),(#30997,#30998,#30999,#31000,#31001,
#31002,#31003,#31004,#31005,#31006,#31007,#31008),(#31009,#31010,#31011,
#31012,#31013,#31014,#31015,#31016,#31017,#31018,#31019,#31020),(#31021,
#31022,#31023,#31024,#31025,#31026,#31027,#31028,#31029,#31030,#31031,#31032)),
 .UNSPECIFIED.,.F.,.F.,.F.)
B_SPLINE_SURFACE_WITH_KNOTS((4,4),(4,2,2,2,2,4),(0.,1.),(0.,0.0783698504851048,
0.308777387863329,0.539184925242218,0.769592462621109,1.),.UNSPECIFIED.)
GEOMETRIC_REPRESENTATION_ITEM()
RATIONAL_B_SPLINE_SURFACE(((1.,1.,1.,1.,1.,1.,1.,1.,1.,1.,1.,1.),(0.833333333333332,
0.833333333333332,0.833333333333332,0.833333333333332,0.833333333333332,
0.833333333333332,0.833333333333332,0.833333333333332,0.833333333333332,
0.833333333333332,0.833333333333332,0.833333333333332),(0.833333333333332,
0.833333333333332,0.833333333333332,0.833333333333332,0.833333333333332,
0.833333333333332,0.833333333333332,0.833333333333332,0.833333333333332,
0.833333333333332,0.833333333333332,0.833333333333332),(1.,1.,1.,1.,1.,
1.,1.,1.,1.,1.,1.,1.)))
REPRESENTATION_ITEM('')
SURFACE()
);
#479=(
BOUNDED_SURFACE()
B_SPLINE_SURFACE(3,3,((#31049,#31050,#31051,#31052,#31053,#31054,#31055,
#31056,#31057,#31058,#31059,#31060),(#31061,#31062,#31063,#31064,#31065,
#31066,#31067,#31068,#31069,#31070,#31071,#31072),(#31073,#31074,#31075,
#31076,#31077,#31078,#31079,#31080,#31081,#31082,#31083,#31084),(#31085,
#31086,#31087,#31088,#31089,#31090,#31091,#31092,#31093,#31094,#31095,#31096)),
 .UNSPECIFIED.,.F.,.F.,.F.)
B_SPLINE_SURFACE_WITH_KNOTS((4,4),(4,2,2,2,2,4),(0.,1.),(0.,0.0783698504851048,
0.308777387863329,0.539184925242218,0.769592462621109,1.),.UNSPECIFIED.)
GEOMETRIC_REPRESENTATION_ITEM()
RATIONAL_B_SPLINE_SURFACE(((1.,1.,1.,1.,1.,1.,1.,1.,1.,1.,1.,1.),(0.987189825241073,
0.987189825241073,0.987189825241073,0.987189825241073,0.987189825241073,
0.987189825241073,0.987189825241073,0.987189825241073,0.987189825241073,
0.987189825241073,0.987189825241073,0.987189825241073),(0.987189825241073,
0.987189825241073,0.987189825241073,0.987189825241073,0.987189825241073,
0.987189825241073,0.987189825241073,0.987189825241073,0.987189825241073,
0.987189825241073,0.987189825241073,0.987189825241073),(1.,1.,1.,1.,1.,
1.,1.,1.,1.,1.,1.,1.)))
REPRESENTATION_ITEM('')
SURFACE()
);
#480=(
BOUNDED_SURFACE()
B_SPLINE_SURFACE(3,3,((#31097,#31098,#31099,#31100,#31101,#31102,#31103,
#31104,#31105,#31106,#31107,#31108),(#31109,#31110,#31111,#31112,#31113,
#31114,#31115,#31116,#31117,#31118,#31119,#31120),(#31121,#31122,#31123,
#31124,#31125,#31126,#31127,#31128,#31129,#31130,#31131,#31132),(#31133,
#31134,#31135,#31136,#31137,#31138,#31139,#31140,#31141,#31142,#31143,#31144)),
 .UNSPECIFIED.,.F.,.F.,.F.)
B_SPLINE_SURFACE_WITH_KNOTS((4,4),(4,2,2,2,2,4),(0.,1.),(0.,0.0783698504851048,
0.308777387863329,0.539184925242218,0.769592462621109,1.),.UNSPECIFIED.)
GEOMETRIC_REPRESENTATION_ITEM()
RATIONAL_B_SPLINE_SURFACE(((1.,1.,1.,1.,1.,1.,1.,1.,1.,1.,1.,1.),(0.987189825241073,
0.987189825241073,0.987189825241073,0.987189825241073,0.987189825241073,
0.987189825241073,0.987189825241073,0.987189825241073,0.987189825241073,
0.987189825241073,0.987189825241073,0.987189825241073),(0.987189825241073,
0.987189825241073,0.987189825241073,0.987189825241073,0.987189825241073,
0.987189825241073,0.987189825241073,0.987189825241073,0.987189825241073,
0.987189825241073,0.987189825241073,0.987189825241073),(1.,1.,1.,1.,1.,
1.,1.,1.,1.,1.,1.,1.)))
REPRESENTATION_ITEM('')
SURFACE()
);
#481=(
BOUNDED_SURFACE()
B_SPLINE_SURFACE(3,3,((#31145,#31146,#31147,#31148,#31149,#31150,#31151,
#31152,#31153,#31154,#31155,#31156),(#31157,#31158,#31159,#31160,#31161,
#31162,#31163,#31164,#31165,#31166,#31167,#31168),(#31169,#31170,#31171,
#31172,#31173,#31174,#31175,#31176,#31177,#31178,#31179,#31180),(#31181,
#31182,#31183,#31184,#31185,#31186,#31187,#31188,#31189,#31190,#31191,#31192)),
 .UNSPECIFIED.,.F.,.F.,.F.)
B_SPLINE_SURFACE_WITH_KNOTS((4,4),(4,2,2,2,2,4),(0.,1.),(0.,0.0783698481609166,
0.308777386120188,0.539184924080124,0.769592462040062,1.),.UNSPECIFIED.)
GEOMETRIC_REPRESENTATION_ITEM()
RATIONAL_B_SPLINE_SURFACE(((1.,1.,1.,1.,1.,1.,1.,1.,1.,1.,1.,1.),(0.833333333333333,
0.833333333333333,0.833333333333333,0.833333333333333,0.833333333333333,
0.833333333333333,0.833333333333333,0.833333333333333,0.833333333333333,
0.833333333333333,0.833333333333333,0.833333333333333),(0.833333333333333,
0.833333333333333,0.833333333333333,0.833333333333333,0.833333333333333,
0.833333333333333,0.833333333333333,0.833333333333333,0.833333333333333,
0.833333333333333,0.833333333333333,0.833333333333333),(1.,1.,1.,1.,1.,
1.,1.,1.,1.,1.,1.,1.)))
REPRESENTATION_ITEM('')
SURFACE()
);
#482=(
BOUNDED_SURFACE()
B_SPLINE_SURFACE(3,3,((#31209,#31210,#31211,#31212,#31213,#31214,#31215,
#31216,#31217,#31218,#31219,#31220),(#31221,#31222,#31223,#31224,#31225,
#31226,#31227,#31228,#31229,#31230,#31231,#31232),(#31233,#31234,#31235,
#31236,#31237,#31238,#31239,#31240,#31241,#31242,#31243,#31244),(#31245,
#31246,#31247,#31248,#31249,#31250,#31251,#31252,#31253,#31254,#31255,#31256)),
 .UNSPECIFIED.,.F.,.F.,.F.)
B_SPLINE_SURFACE_WITH_KNOTS((4,4),(4,2,2,2,2,4),(0.,1.),(0.,0.0783698481609166,
0.308777386120188,0.539184924080124,0.769592462040062,1.),.UNSPECIFIED.)
GEOMETRIC_REPRESENTATION_ITEM()
RATIONAL_B_SPLINE_SURFACE(((1.,1.,1.,1.,1.,1.,1.,1.,1.,1.,1.,1.),(0.987189825241073,
0.987189825241073,0.987189825241073,0.987189825241073,0.987189825241073,
0.987189825241073,0.987189825241073,0.987189825241073,0.987189825241073,
0.987189825241073,0.987189825241073,0.987189825241073),(0.987189825241073,
0.987189825241073,0.987189825241073,0.987189825241073,0.987189825241073,
0.987189825241073,0.987189825241073,0.987189825241073,0.987189825241073,
0.987189825241073,0.987189825241073,0.987189825241073),(1.,1.,1.,1.,1.,
1.,1.,1.,1.,1.,1.,1.)))
REPRESENTATION_ITEM('')
SURFACE()
);
#483=(
BOUNDED_SURFACE()
B_SPLINE_SURFACE(3,3,((#31257,#31258,#31259,#31260,#31261,#31262,#31263,
#31264,#31265,#31266,#31267,#31268),(#31269,#31270,#31271,#31272,#31273,
#31274,#31275,#31276,#31277,#31278,#31279,#31280),(#31281,#31282,#31283,
#31284,#31285,#31286,#31287,#31288,#31289,#31290,#31291,#31292),(#31293,
#31294,#31295,#31296,#31297,#31298,#31299,#31300,#31301,#31302,#31303,#31304)),
 .UNSPECIFIED.,.F.,.F.,.F.)
B_SPLINE_SURFACE_WITH_KNOTS((4,4),(4,2,2,2,2,4),(0.,1.),(0.,0.0783698481609166,
0.308777386120188,0.539184924080124,0.769592462040062,1.),.UNSPECIFIED.)
GEOMETRIC_REPRESENTATION_ITEM()
RATIONAL_B_SPLINE_SURFACE(((1.,1.,1.,1.,1.,1.,1.,1.,1.,1.,1.,1.),(0.987189825241073,
0.987189825241073,0.987189825241073,0.987189825241073,0.987189825241073,
0.987189825241073,0.987189825241073,0.987189825241073,0.987189825241073,
0.987189825241073,0.987189825241073,0.987189825241073),(0.987189825241073,
0.987189825241073,0.987189825241073,0.987189825241073,0.987189825241073,
0.987189825241073,0.987189825241073,0.987189825241073,0.987189825241073,
0.987189825241073,0.987189825241073,0.987189825241073),(1.,1.,1.,1.,1.,
1.,1.,1.,1.,1.,1.,1.)))
REPRESENTATION_ITEM('')
SURFACE()
);
#484=(
BOUNDED_SURFACE()
B_SPLINE_SURFACE(3,3,((#31305,#31306,#31307,#31308,#31309,#31310,#31311,
#31312,#31313,#31314,#31315,#31316),(#31317,#31318,#31319,#31320,#31321,
#31322,#31323,#31324,#31325,#31326,#31327,#31328),(#31329,#31330,#31331,
#31332,#31333,#31334,#31335,#31336,#31337,#31338,#31339,#31340),(#31341,
#31342,#31343,#31344,#31345,#31346,#31347,#31348,#31349,#31350,#31351,#31352)),
 .UNSPECIFIED.,.F.,.F.,.F.)
B_SPLINE_SURFACE_WITH_KNOTS((4,4),(4,2,2,2,2,4),(0.,1.),(0.,0.0783698437311068,
0.308777382797831,0.539184921865219,0.769592460932609,1.),.UNSPECIFIED.)
GEOMETRIC_REPRESENTATION_ITEM()
RATIONAL_B_SPLINE_SURFACE(((1.,1.,1.,1.,1.,1.,1.,1.,1.,1.,1.,1.),(0.833333333333331,
0.833333333333331,0.833333333333331,0.833333333333331,0.833333333333331,
0.833333333333331,0.833333333333331,0.833333333333331,0.833333333333331,
0.833333333333331,0.833333333333331,0.833333333333331),(0.833333333333331,
0.833333333333331,0.833333333333331,0.833333333333331,0.833333333333331,
0.833333333333331,0.833333333333331,0.833333333333331,0.833333333333331,
0.833333333333331,0.833333333333331,0.833333333333331),(1.,1.,1.,1.,1.,
1.,1.,1.,1.,1.,1.,1.)))
REPRESENTATION_ITEM('')
SURFACE()
);
#485=(
BOUNDED_SURFACE()
B_SPLINE_SURFACE(3,3,((#31369,#31370,#31371,#31372,#31373,#31374,#31375,
#31376,#31377,#31378,#31379,#31380),(#31381,#31382,#31383,#31384,#31385,
#31386,#31387,#31388,#31389,#31390,#31391,#31392),(#31393,#31394,#31395,
#31396,#31397,#31398,#31399,#31400,#31401,#31402,#31403,#31404),(#31405,
#31406,#31407,#31408,#31409,#31410,#31411,#31412,#31413,#31414,#31415,#31416)),
 .UNSPECIFIED.,.F.,.F.,.F.)
B_SPLINE_SURFACE_WITH_KNOTS((4,4),(4,2,2,2,2,4),(0.,1.),(0.,0.0783698437311068,
0.308777382797831,0.539184921865219,0.769592460932609,1.),.UNSPECIFIED.)
GEOMETRIC_REPRESENTATION_ITEM()
RATIONAL_B_SPLINE_SURFACE(((1.,1.,1.,1.,1.,1.,1.,1.,1.,1.,1.,1.),(0.987189825241073,
0.987189825241073,0.987189825241073,0.987189825241073,0.987189825241073,
0.987189825241073,0.987189825241073,0.987189825241073,0.987189825241073,
0.987189825241073,0.987189825241073,0.987189825241073),(0.987189825241073,
0.987189825241073,0.987189825241073,0.987189825241073,0.987189825241073,
0.987189825241073,0.987189825241073,0.987189825241073,0.987189825241073,
0.987189825241073,0.987189825241073,0.987189825241073),(1.,1.,1.,1.,1.,
1.,1.,1.,1.,1.,1.,1.)))
REPRESENTATION_ITEM('')
SURFACE()
);
#486=(
BOUNDED_SURFACE()
B_SPLINE_SURFACE(3,3,((#31417,#31418,#31419,#31420,#31421,#31422,#31423,
#31424,#31425,#31426,#31427,#31428),(#31429,#31430,#31431,#31432,#31433,
#31434,#31435,#31436,#31437,#31438,#31439,#31440),(#31441,#31442,#31443,
#31444,#31445,#31446,#31447,#31448,#31449,#31450,#31451,#31452),(#31453,
#31454,#31455,#31456,#31457,#31458,#31459,#31460,#31461,#31462,#31463,#31464)),
 .UNSPECIFIED.,.F.,.F.,.F.)
B_SPLINE_SURFACE_WITH_KNOTS((4,4),(4,2,2,2,2,4),(0.,1.),(0.,0.0783698437311068,
0.308777382797831,0.539184921865219,0.769592460932609,1.),.UNSPECIFIED.)
GEOMETRIC_REPRESENTATION_ITEM()
RATIONAL_B_SPLINE_SURFACE(((1.,1.,1.,1.,1.,1.,1.,1.,1.,1.,1.,1.),(0.987189825241073,
0.987189825241073,0.987189825241073,0.987189825241073,0.987189825241073,
0.987189825241073,0.987189825241073,0.987189825241073,0.987189825241073,
0.987189825241073,0.987189825241073,0.987189825241073),(0.987189825241073,
0.987189825241073,0.987189825241073,0.987189825241073,0.987189825241073,
0.987189825241073,0.987189825241073,0.987189825241073,0.987189825241073,
0.987189825241073,0.987189825241073,0.987189825241073),(1.,1.,1.,1.,1.,
1.,1.,1.,1.,1.,1.,1.)))
REPRESENTATION_ITEM('')
SURFACE()
);
#487=(
BOUNDED_SURFACE()
B_SPLINE_SURFACE(3,3,((#31465,#31466,#31467,#31468,#31469,#31470,#31471,
#31472,#31473,#31474,#31475,#31476),(#31477,#31478,#31479,#31480,#31481,
#31482,#31483,#31484,#31485,#31486,#31487,#31488),(#31489,#31490,#31491,
#31492,#31493,#31494,#31495,#31496,#31497,#31498,#31499,#31500),(#31501,
#31502,#31503,#31504,#31505,#31506,#31507,#31508,#31509,#31510,#31511,#31512)),
 .UNSPECIFIED.,.F.,.F.,.F.)
B_SPLINE_SURFACE_WITH_KNOTS((4,4),(4,2,2,2,2,4),(0.,1.),(0.,0.078369838840124,
0.308777379129593,0.539184919419728,0.769592459709864,1.),.UNSPECIFIED.)
GEOMETRIC_REPRESENTATION_ITEM()
RATIONAL_B_SPLINE_SURFACE(((1.,1.,1.,1.,1.,1.,1.,1.,1.,1.,1.,1.),(0.833333333333332,
0.833333333333332,0.833333333333332,0.833333333333332,0.833333333333332,
0.833333333333332,0.833333333333332,0.833333333333332,0.833333333333332,
0.833333333333332,0.833333333333332,0.833333333333332),(0.833333333333332,
0.833333333333332,0.833333333333332,0.833333333333332,0.833333333333332,
0.833333333333332,0.833333333333332,0.833333333333332,0.833333333333332,
0.833333333333332,0.833333333333332,0.833333333333332),(1.,1.,1.,1.,1.,
1.,1.,1.,1.,1.,1.,1.)))
REPRESENTATION_ITEM('')
SURFACE()
);
#488=(
BOUNDED_SURFACE()
B_SPLINE_SURFACE(3,3,((#31529,#31530,#31531,#31532,#31533,#31534,#31535,
#31536,#31537,#31538,#31539,#31540),(#31541,#31542,#31543,#31544,#31545,
#31546,#31547,#31548,#31549,#31550,#31551,#31552),(#31553,#31554,#31555,
#31556,#31557,#31558,#31559,#31560,#31561,#31562,#31563,#31564),(#31565,
#31566,#31567,#31568,#31569,#31570,#31571,#31572,#31573,#31574,#31575,#31576)),
 .UNSPECIFIED.,.F.,.F.,.F.)
B_SPLINE_SURFACE_WITH_KNOTS((4,4),(4,2,2,2,2,4),(0.,1.),(0.,0.078369838840124,
0.308777379129593,0.539184919419728,0.769592459709864,1.),.UNSPECIFIED.)
GEOMETRIC_REPRESENTATION_ITEM()
RATIONAL_B_SPLINE_SURFACE(((1.,1.,1.,1.,1.,1.,1.,1.,1.,1.,1.,1.),(0.987189825241073,
0.987189825241073,0.987189825241073,0.987189825241073,0.987189825241073,
0.987189825241073,0.987189825241073,0.987189825241073,0.987189825241073,
0.987189825241073,0.987189825241073,0.987189825241073),(0.987189825241073,
0.987189825241073,0.987189825241073,0.987189825241073,0.987189825241073,
0.987189825241073,0.987189825241073,0.987189825241073,0.987189825241073,
0.987189825241073,0.987189825241073,0.987189825241073),(1.,1.,1.,1.,1.,
1.,1.,1.,1.,1.,1.,1.)))
REPRESENTATION_ITEM('')
SURFACE()
);
#489=(
BOUNDED_SURFACE()
B_SPLINE_SURFACE(3,3,((#31577,#31578,#31579,#31580,#31581,#31582,#31583,
#31584,#31585,#31586,#31587,#31588),(#31589,#31590,#31591,#31592,#31593,
#31594,#31595,#31596,#31597,#31598,#31599,#31600),(#31601,#31602,#31603,
#31604,#31605,#31606,#31607,#31608,#31609,#31610,#31611,#31612),(#31613,
#31614,#31615,#31616,#31617,#31618,#31619,#31620,#31621,#31622,#31623,#31624)),
 .UNSPECIFIED.,.F.,.F.,.F.)
B_SPLINE_SURFACE_WITH_KNOTS((4,4),(4,2,2,2,2,4),(0.,1.),(0.,0.078369838840124,
0.308777379129593,0.539184919419728,0.769592459709864,1.),.UNSPECIFIED.)
GEOMETRIC_REPRESENTATION_ITEM()
RATIONAL_B_SPLINE_SURFACE(((1.,1.,1.,1.,1.,1.,1.,1.,1.,1.,1.,1.),(0.987189825241073,
0.987189825241073,0.987189825241073,0.987189825241073,0.987189825241073,
0.987189825241073,0.987189825241073,0.987189825241073,0.987189825241073,
0.987189825241073,0.987189825241073,0.987189825241073),(0.987189825241073,
0.987189825241073,0.987189825241073,0.987189825241073,0.987189825241073,
0.987189825241073,0.987189825241073,0.987189825241073,0.987189825241073,
0.987189825241073,0.987189825241073,0.987189825241073),(1.,1.,1.,1.,1.,
1.,1.,1.,1.,1.,1.,1.)))
REPRESENTATION_ITEM('')
SURFACE()
);
#490=(
BOUNDED_SURFACE()
B_SPLINE_SURFACE(3,3,((#31625,#31626,#31627,#31628,#31629,#31630,#31631,
#31632,#31633,#31634,#31635,#31636),(#31637,#31638,#31639,#31640,#31641,
#31642,#31643,#31644,#31645,#31646,#31647,#31648),(#31649,#31650,#31651,
#31652,#31653,#31654,#31655,#31656,#31657,#31658,#31659,#31660),(#31661,
#31662,#31663,#31664,#31665,#31666,#31667,#31668,#31669,#31670,#31671,#31672)),
 .UNSPECIFIED.,.F.,.F.,.F.)
B_SPLINE_SURFACE_WITH_KNOTS((4,4),(4,2,2,2,2,4),(0.,1.),(0.,0.0783698352504276,
0.308777376437321,0.539184917624879,0.76959245881244,1.),.UNSPECIFIED.)
GEOMETRIC_REPRESENTATION_ITEM()
RATIONAL_B_SPLINE_SURFACE(((1.,1.,1.,1.,1.,1.,1.,1.,1.,1.,1.,1.),(0.833333333333332,
0.833333333333332,0.833333333333332,0.833333333333332,0.833333333333332,
0.833333333333332,0.833333333333332,0.833333333333332,0.833333333333332,
0.833333333333332,0.833333333333332,0.833333333333332),(0.833333333333332,
0.833333333333332,0.833333333333332,0.833333333333332,0.833333333333332,
0.833333333333332,0.833333333333332,0.833333333333332,0.833333333333332,
0.833333333333332,0.833333333333332,0.833333333333332),(1.,1.,1.,1.,1.,
1.,1.,1.,1.,1.,1.,1.)))
REPRESENTATION_ITEM('')
SURFACE()
);
#491=(
BOUNDED_SURFACE()
B_SPLINE_SURFACE(3,3,((#31689,#31690,#31691,#31692,#31693,#31694,#31695,
#31696,#31697,#31698,#31699,#31700),(#31701,#31702,#31703,#31704,#31705,
#31706,#31707,#31708,#31709,#31710,#31711,#31712),(#31713,#31714,#31715,
#31716,#31717,#31718,#31719,#31720,#31721,#31722,#31723,#31724),(#31725,
#31726,#31727,#31728,#31729,#31730,#31731,#31732,#31733,#31734,#31735,#31736)),
 .UNSPECIFIED.,.F.,.F.,.F.)
B_SPLINE_SURFACE_WITH_KNOTS((4,4),(4,2,2,2,2,4),(0.,1.),(0.,0.0783698352504276,
0.308777376437321,0.539184917624879,0.76959245881244,1.),.UNSPECIFIED.)
GEOMETRIC_REPRESENTATION_ITEM()
RATIONAL_B_SPLINE_SURFACE(((1.,1.,1.,1.,1.,1.,1.,1.,1.,1.,1.,1.),(0.987189825241073,
0.987189825241073,0.987189825241073,0.987189825241073,0.987189825241073,
0.987189825241073,0.987189825241073,0.987189825241073,0.987189825241073,
0.987189825241073,0.987189825241073,0.987189825241073),(0.987189825241073,
0.987189825241073,0.987189825241073,0.987189825241073,0.987189825241073,
0.987189825241073,0.987189825241073,0.987189825241073,0.987189825241073,
0.987189825241073,0.987189825241073,0.987189825241073),(1.,1.,1.,1.,1.,
1.,1.,1.,1.,1.,1.,1.)))
REPRESENTATION_ITEM('')
SURFACE()
);
#492=(
BOUNDED_SURFACE()
B_SPLINE_SURFACE(3,3,((#31737,#31738,#31739,#31740,#31741,#31742,#31743,
#31744,#31745,#31746,#31747,#31748),(#31749,#31750,#31751,#31752,#31753,
#31754,#31755,#31756,#31757,#31758,#31759,#31760),(#31761,#31762,#31763,
#31764,#31765,#31766,#31767,#31768,#31769,#31770,#31771,#31772),(#31773,
#31774,#31775,#31776,#31777,#31778,#31779,#31780,#31781,#31782,#31783,#31784)),
 .UNSPECIFIED.,.F.,.F.,.F.)
B_SPLINE_SURFACE_WITH_KNOTS((4,4),(4,2,2,2,2,4),(0.,1.),(0.,0.0783698352504276,
0.308777376437321,0.539184917624879,0.76959245881244,1.),.UNSPECIFIED.)
GEOMETRIC_REPRESENTATION_ITEM()
RATIONAL_B_SPLINE_SURFACE(((1.,1.,1.,1.,1.,1.,1.,1.,1.,1.,1.,1.),(0.987189825241073,
0.987189825241073,0.987189825241073,0.987189825241073,0.987189825241073,
0.987189825241073,0.987189825241073,0.987189825241073,0.987189825241073,
0.987189825241073,0.987189825241073,0.987189825241073),(0.987189825241073,
0.987189825241073,0.987189825241073,0.987189825241073,0.987189825241073,
0.987189825241073,0.987189825241073,0.987189825241073,0.987189825241073,
0.987189825241073,0.987189825241073,0.987189825241073),(1.,1.,1.,1.,1.,
1.,1.,1.,1.,1.,1.,1.)))
REPRESENTATION_ITEM('')
SURFACE()
);
#493=(
BOUNDED_SURFACE()
B_SPLINE_SURFACE(3,3,((#31785,#31786,#31787,#31788,#31789,#31790,#31791,
#31792,#31793,#31794,#31795,#31796),(#31797,#31798,#31799,#31800,#31801,
#31802,#31803,#31804,#31805,#31806,#31807,#31808),(#31809,#31810,#31811,
#31812,#31813,#31814,#31815,#31816,#31817,#31818,#31819,#31820),(#31821,
#31822,#31823,#31824,#31825,#31826,#31827,#31828,#31829,#31830,#31831,#31832)),
 .UNSPECIFIED.,.F.,.F.,.F.)
B_SPLINE_SURFACE_WITH_KNOTS((4,4),(4,2,2,2,2,4),(0.,1.),(0.,0.0783698293107417,
0.308777371982557,0.539184914655036,0.769592457327518,1.),.UNSPECIFIED.)
GEOMETRIC_REPRESENTATION_ITEM()
RATIONAL_B_SPLINE_SURFACE(((1.,1.,1.,1.,1.,1.,1.,1.,1.,1.,1.,1.),(0.833333333333332,
0.833333333333332,0.833333333333332,0.833333333333332,0.833333333333332,
0.833333333333332,0.833333333333332,0.833333333333332,0.833333333333332,
0.833333333333332,0.833333333333332,0.833333333333332),(0.833333333333332,
0.833333333333332,0.833333333333332,0.833333333333332,0.833333333333332,
0.833333333333332,0.833333333333332,0.833333333333332,0.833333333333332,
0.833333333333332,0.833333333333332,0.833333333333332),(1.,1.,1.,1.,1.,
1.,1.,1.,1.,1.,1.,1.)))
REPRESENTATION_ITEM('')
SURFACE()
);
#494=(
BOUNDED_SURFACE()
B_SPLINE_SURFACE(3,3,((#31849,#31850,#31851,#31852,#31853,#31854,#31855,
#31856,#31857,#31858,#31859,#31860),(#31861,#31862,#31863,#31864,#31865,
#31866,#31867,#31868,#31869,#31870,#31871,#31872),(#31873,#31874,#31875,
#31876,#31877,#31878,#31879,#31880,#31881,#31882,#31883,#31884),(#31885,
#31886,#31887,#31888,#31889,#31890,#31891,#31892,#31893,#31894,#31895,#31896)),
 .UNSPECIFIED.,.F.,.F.,.F.)
B_SPLINE_SURFACE_WITH_KNOTS((4,4),(4,2,2,2,2,4),(0.,1.),(0.,0.0783698293107417,
0.308777371982557,0.539184914655036,0.769592457327518,1.),.UNSPECIFIED.)
GEOMETRIC_REPRESENTATION_ITEM()
RATIONAL_B_SPLINE_SURFACE(((1.,1.,1.,1.,1.,1.,1.,1.,1.,1.,1.,1.),(0.987189825241073,
0.987189825241073,0.987189825241073,0.987189825241073,0.987189825241073,
0.987189825241073,0.987189825241073,0.987189825241073,0.987189825241073,
0.987189825241073,0.987189825241073,0.987189825241073),(0.987189825241073,
0.987189825241073,0.987189825241073,0.987189825241073,0.987189825241073,
0.987189825241073,0.987189825241073,0.987189825241073,0.987189825241073,
0.987189825241073,0.987189825241073,0.987189825241073),(1.,1.,1.,1.,1.,
1.,1.,1.,1.,1.,1.,1.)))
REPRESENTATION_ITEM('')
SURFACE()
);
#495=(
BOUNDED_SURFACE()
B_SPLINE_SURFACE(3,3,((#31897,#31898,#31899,#31900,#31901,#31902,#31903,
#31904,#31905,#31906,#31907,#31908),(#31909,#31910,#31911,#31912,#31913,
#31914,#31915,#31916,#31917,#31918,#31919,#31920),(#31921,#31922,#31923,
#31924,#31925,#31926,#31927,#31928,#31929,#31930,#31931,#31932),(#31933,
#31934,#31935,#31936,#31937,#31938,#31939,#31940,#31941,#31942,#31943,#31944)),
 .UNSPECIFIED.,.F.,.F.,.F.)
B_SPLINE_SURFACE_WITH_KNOTS((4,4),(4,2,2,2,2,4),(0.,1.),(0.,0.0783698293107417,
0.308777371982557,0.539184914655036,0.769592457327518,1.),.UNSPECIFIED.)
GEOMETRIC_REPRESENTATION_ITEM()
RATIONAL_B_SPLINE_SURFACE(((1.,1.,1.,1.,1.,1.,1.,1.,1.,1.,1.,1.),(0.987189825241073,
0.987189825241073,0.987189825241073,0.987189825241073,0.987189825241073,
0.987189825241073,0.987189825241073,0.987189825241073,0.987189825241073,
0.987189825241073,0.987189825241073,0.987189825241073),(0.987189825241073,
0.987189825241073,0.987189825241073,0.987189825241073,0.987189825241073,
0.987189825241073,0.987189825241073,0.987189825241073,0.987189825241073,
0.987189825241073,0.987189825241073,0.987189825241073),(1.,1.,1.,1.,1.,
1.,1.,1.,1.,1.,1.,1.)))
REPRESENTATION_ITEM('')
SURFACE()
);
#496=(
BOUNDED_SURFACE()
B_SPLINE_SURFACE(3,3,((#31945,#31946,#31947,#31948,#31949,#31950,#31951,
#31952,#31953,#31954,#31955,#31956,#31957,#31958),(#31959,#31960,#31961,
#31962,#31963,#31964,#31965,#31966,#31967,#31968,#31969,#31970,#31971,#31972),
(#31973,#31974,#31975,#31976,#31977,#31978,#31979,#31980,#31981,#31982,
#31983,#31984,#31985,#31986),(#31987,#31988,#31989,#31990,#31991,#31992,
#31993,#31994,#31995,#31996,#31997,#31998,#31999,#32000)),.UNSPECIFIED.,
 .F.,.F.,.F.)
B_SPLINE_SURFACE_WITH_KNOTS((4,4),(4,2,2,2,2,2,4),(0.,1.),(0.,0.0183879232268621,
0.0783698352504225,0.308777376437317,0.539184917624877,0.769592458812438,
1.),.UNSPECIFIED.)
GEOMETRIC_REPRESENTATION_ITEM()
RATIONAL_B_SPLINE_SURFACE(((1.,1.,1.,1.,1.,1.,1.,1.,1.,1.,1.,1.,1.,1.),
(0.833333333333332,0.833333333333332,0.833333333333332,0.833333333333332,
0.833333333333332,0.833333333333332,0.833333333333332,0.833333333333332,
0.833333333333332,0.833333333333332,0.833333333333332,0.833333333333332,
0.833333333333332,0.833333333333332),(0.833333333333332,0.833333333333332,
0.833333333333332,0.833333333333332,0.833333333333332,0.833333333333332,
0.833333333333332,0.833333333333332,0.833333333333332,0.833333333333332,
0.833333333333332,0.833333333333332,0.833333333333332,0.833333333333332),
(1.,1.,1.,1.,1.,1.,1.,1.,1.,1.,1.,1.,1.,1.)))
REPRESENTATION_ITEM('')
SURFACE()
);
#497=(
BOUNDED_SURFACE()
B_SPLINE_SURFACE(3,3,((#32019,#32020,#32021,#32022,#32023,#32024,#32025,
#32026,#32027,#32028,#32029,#32030,#32031,#32032),(#32033,#32034,#32035,
#32036,#32037,#32038,#32039,#32040,#32041,#32042,#32043,#32044,#32045,#32046),
(#32047,#32048,#32049,#32050,#32051,#32052,#32053,#32054,#32055,#32056,
#32057,#32058,#32059,#32060),(#32061,#32062,#32063,#32064,#32065,#32066,
#32067,#32068,#32069,#32070,#32071,#32072,#32073,#32074)),.UNSPECIFIED.,
 .F.,.F.,.F.)
B_SPLINE_SURFACE_WITH_KNOTS((4,4),(4,2,2,2,2,2,4),(0.,1.),(0.,0.0183879232268621,
0.0783698352504225,0.308777376437317,0.539184917624877,0.769592458812438,
1.),.UNSPECIFIED.)
GEOMETRIC_REPRESENTATION_ITEM()
RATIONAL_B_SPLINE_SURFACE(((1.,1.,1.,1.,1.,1.,1.,1.,1.,1.,1.,1.,1.,1.),
(0.987189825241073,0.987189825241073,0.987189825241073,0.987189825241073,
0.987189825241073,0.987189825241073,0.987189825241073,0.987189825241073,
0.987189825241073,0.987189825241073,0.987189825241073,0.987189825241073,
0.987189825241073,0.987189825241073),(0.987189825241073,0.987189825241073,
0.987189825241073,0.987189825241073,0.987189825241073,0.987189825241073,
0.987189825241073,0.987189825241073,0.987189825241073,0.987189825241073,
0.987189825241073,0.987189825241073,0.987189825241073,0.987189825241073),
(1.,1.,1.,1.,1.,1.,1.,1.,1.,1.,1.,1.,1.,1.)))
REPRESENTATION_ITEM('')
SURFACE()
);
#498=(
BOUNDED_SURFACE()
B_SPLINE_SURFACE(3,3,((#32075,#32076,#32077,#32078,#32079,#32080,#32081,
#32082,#32083,#32084,#32085,#32086,#32087,#32088),(#32089,#32090,#32091,
#32092,#32093,#32094,#32095,#32096,#32097,#32098,#32099,#32100,#32101,#32102),
(#32103,#32104,#32105,#32106,#32107,#32108,#32109,#32110,#32111,#32112,
#32113,#32114,#32115,#32116),(#32117,#32118,#32119,#32120,#32121,#32122,
#32123,#32124,#32125,#32126,#32127,#32128,#32129,#32130)),.UNSPECIFIED.,
 .F.,.F.,.F.)
B_SPLINE_SURFACE_WITH_KNOTS((4,4),(4,2,2,2,2,2,4),(0.,1.),(0.,0.0183879232268621,
0.0783698352504225,0.308777376437317,0.539184917624877,0.769592458812438,
1.),.UNSPECIFIED.)
GEOMETRIC_REPRESENTATION_ITEM()
RATIONAL_B_SPLINE_SURFACE(((1.,1.,1.,1.,1.,1.,1.,1.,1.,1.,1.,1.,1.,1.),
(0.987189825241073,0.987189825241073,0.987189825241073,0.987189825241073,
0.987189825241073,0.987189825241073,0.987189825241073,0.987189825241073,
0.987189825241073,0.987189825241073,0.987189825241073,0.987189825241073,
0.987189825241073,0.987189825241073),(0.987189825241073,0.987189825241073,
0.987189825241073,0.987189825241073,0.987189825241073,0.987189825241073,
0.987189825241073,0.987189825241073,0.987189825241073,0.987189825241073,
0.987189825241073,0.987189825241073,0.987189825241073,0.987189825241073),
(1.,1.,1.,1.,1.,1.,1.,1.,1.,1.,1.,1.,1.,1.)))
REPRESENTATION_ITEM('')
SURFACE()
);
#499=(
BOUNDED_SURFACE()
B_SPLINE_SURFACE(3,3,((#32131,#32132,#32133,#32134,#32135,#32136,#32137,
#32138,#32139,#32140,#32141,#32142),(#32143,#32144,#32145,#32146,#32147,
#32148,#32149,#32150,#32151,#32152,#32153,#32154),(#32155,#32156,#32157,
#32158,#32159,#32160,#32161,#32162,#32163,#32164,#32165,#32166),(#32167,
#32168,#32169,#32170,#32171,#32172,#32173,#32174,#32175,#32176,#32177,#32178)),
 .UNSPECIFIED.,.F.,.F.,.F.)
B_SPLINE_SURFACE_WITH_KNOTS((4,4),(4,2,2,2,2,4),(0.,1.),(0.,0.0783698388401176,
0.308777379129589,0.539184919419725,0.769592459709862,1.),.UNSPECIFIED.)
GEOMETRIC_REPRESENTATION_ITEM()
RATIONAL_B_SPLINE_SURFACE(((1.,1.,1.,1.,1.,1.,1.,1.,1.,1.,1.,1.),(0.833333333333331,
0.833333333333331,0.833333333333331,0.833333333333331,0.833333333333331,
0.833333333333331,0.833333333333331,0.833333333333331,0.833333333333331,
0.833333333333331,0.833333333333331,0.833333333333331),(0.833333333333331,
0.833333333333331,0.833333333333331,0.833333333333331,0.833333333333331,
0.833333333333331,0.833333333333331,0.833333333333331,0.833333333333331,
0.833333333333331,0.833333333333331,0.833333333333331),(1.,1.,1.,1.,1.,
1.,1.,1.,1.,1.,1.,1.)))
REPRESENTATION_ITEM('')
SURFACE()
);
#500=(
BOUNDED_SURFACE()
B_SPLINE_SURFACE(3,3,((#32195,#32196,#32197,#32198,#32199,#32200,#32201,
#32202,#32203,#32204,#32205,#32206),(#32207,#32208,#32209,#32210,#32211,
#32212,#32213,#32214,#32215,#32216,#32217,#32218),(#32219,#32220,#32221,
#32222,#32223,#32224,#32225,#32226,#32227,#32228,#32229,#32230),(#32231,
#32232,#32233,#32234,#32235,#32236,#32237,#32238,#32239,#32240,#32241,#32242)),
 .UNSPECIFIED.,.F.,.F.,.F.)
B_SPLINE_SURFACE_WITH_KNOTS((4,4),(4,2,2,2,2,4),(0.,1.),(0.,0.0783698388401176,
0.308777379129589,0.539184919419725,0.769592459709862,1.),.UNSPECIFIED.)
GEOMETRIC_REPRESENTATION_ITEM()
RATIONAL_B_SPLINE_SURFACE(((1.,1.,1.,1.,1.,1.,1.,1.,1.,1.,1.,1.),(0.987189825241073,
0.987189825241073,0.987189825241073,0.987189825241073,0.987189825241073,
0.987189825241073,0.987189825241073,0.987189825241073,0.987189825241073,
0.987189825241073,0.987189825241073,0.987189825241073),(0.987189825241073,
0.987189825241073,0.987189825241073,0.987189825241073,0.987189825241073,
0.987189825241073,0.987189825241073,0.987189825241073,0.987189825241073,
0.987189825241073,0.987189825241073,0.987189825241073),(1.,1.,1.,1.,1.,
1.,1.,1.,1.,1.,1.,1.)))
REPRESENTATION_ITEM('')
SURFACE()
);
#501=(
BOUNDED_SURFACE()
B_SPLINE_SURFACE(3,3,((#32243,#32244,#32245,#32246,#32247,#32248,#32249,
#32250,#32251,#32252,#32253,#32254),(#32255,#32256,#32257,#32258,#32259,
#32260,#32261,#32262,#32263,#32264,#32265,#32266),(#32267,#32268,#32269,
#32270,#32271,#32272,#32273,#32274,#32275,#32276,#32277,#32278),(#32279,
#32280,#32281,#32282,#32283,#32284,#32285,#32286,#32287,#32288,#32289,#32290)),
 .UNSPECIFIED.,.F.,.F.,.F.)
B_SPLINE_SURFACE_WITH_KNOTS((4,4),(4,2,2,2,2,4),(0.,1.),(0.,0.0783698388401176,
0.308777379129589,0.539184919419725,0.769592459709862,1.),.UNSPECIFIED.)
GEOMETRIC_REPRESENTATION_ITEM()
RATIONAL_B_SPLINE_SURFACE(((1.,1.,1.,1.,1.,1.,1.,1.,1.,1.,1.,1.),(0.987189825241073,
0.987189825241073,0.987189825241073,0.987189825241073,0.987189825241073,
0.987189825241073,0.987189825241073,0.987189825241073,0.987189825241073,
0.987189825241073,0.987189825241073,0.987189825241073),(0.987189825241073,
0.987189825241073,0.987189825241073,0.987189825241073,0.987189825241073,
0.987189825241073,0.987189825241073,0.987189825241073,0.987189825241073,
0.987189825241073,0.987189825241073,0.987189825241073),(1.,1.,1.,1.,1.,
1.,1.,1.,1.,1.,1.,1.)))
REPRESENTATION_ITEM('')
SURFACE()
);
#502=(
BOUNDED_SURFACE()
B_SPLINE_SURFACE(3,3,((#32291,#32292,#32293,#32294,#32295,#32296,#32297,
#32298,#32299,#32300,#32301,#32302),(#32303,#32304,#32305,#32306,#32307,
#32308,#32309,#32310,#32311,#32312,#32313,#32314),(#32315,#32316,#32317,
#32318,#32319,#32320,#32321,#32322,#32323,#32324,#32325,#32326),(#32327,
#32328,#32329,#32330,#32331,#32332,#32333,#32334,#32335,#32336,#32337,#32338)),
 .UNSPECIFIED.,.F.,.F.,.F.)
B_SPLINE_SURFACE_WITH_KNOTS((4,4),(4,2,2,2,2,4),(0.,1.),(0.,0.0783698437311062,
0.30877738279783,0.539184921865219,0.76959246093261,1.),.UNSPECIFIED.)
GEOMETRIC_REPRESENTATION_ITEM()
RATIONAL_B_SPLINE_SURFACE(((1.,1.,1.,1.,1.,1.,1.,1.,1.,1.,1.,1.),(0.833333333333332,
0.833333333333332,0.833333333333332,0.833333333333332,0.833333333333332,
0.833333333333332,0.833333333333332,0.833333333333332,0.833333333333332,
0.833333333333332,0.833333333333332,0.833333333333332),(0.833333333333332,
0.833333333333332,0.833333333333332,0.833333333333332,0.833333333333332,
0.833333333333332,0.833333333333332,0.833333333333332,0.833333333333332,
0.833333333333332,0.833333333333332,0.833333333333332),(1.,1.,1.,1.,1.,
1.,1.,1.,1.,1.,1.,1.)))
REPRESENTATION_ITEM('')
SURFACE()
);
#503=(
BOUNDED_SURFACE()
B_SPLINE_SURFACE(3,3,((#32355,#32356,#32357,#32358,#32359,#32360,#32361,
#32362,#32363,#32364,#32365,#32366),(#32367,#32368,#32369,#32370,#32371,
#32372,#32373,#32374,#32375,#32376,#32377,#32378),(#32379,#32380,#32381,
#32382,#32383,#32384,#32385,#32386,#32387,#32388,#32389,#32390),(#32391,
#32392,#32393,#32394,#32395,#32396,#32397,#32398,#32399,#32400,#32401,#32402)),
 .UNSPECIFIED.,.F.,.F.,.F.)
B_SPLINE_SURFACE_WITH_KNOTS((4,4),(4,2,2,2,2,4),(0.,1.),(0.,0.0783698437311062,
0.30877738279783,0.539184921865219,0.76959246093261,1.),.UNSPECIFIED.)
GEOMETRIC_REPRESENTATION_ITEM()
RATIONAL_B_SPLINE_SURFACE(((1.,1.,1.,1.,1.,1.,1.,1.,1.,1.,1.,1.),(0.987189825241073,
0.987189825241073,0.987189825241073,0.987189825241073,0.987189825241073,
0.987189825241073,0.987189825241073,0.987189825241073,0.987189825241073,
0.987189825241073,0.987189825241073,0.987189825241073),(0.987189825241073,
0.987189825241073,0.987189825241073,0.987189825241073,0.987189825241073,
0.987189825241073,0.987189825241073,0.987189825241073,0.987189825241073,
0.987189825241073,0.987189825241073,0.987189825241073),(1.,1.,1.,1.,1.,
1.,1.,1.,1.,1.,1.,1.)))
REPRESENTATION_ITEM('')
SURFACE()
);
#504=(
BOUNDED_SURFACE()
B_SPLINE_SURFACE(3,3,((#32403,#32404,#32405,#32406,#32407,#32408,#32409,
#32410,#32411,#32412,#32413,#32414),(#32415,#32416,#32417,#32418,#32419,
#32420,#32421,#32422,#32423,#32424,#32425,#32426),(#32427,#32428,#32429,
#32430,#32431,#32432,#32433,#32434,#32435,#32436,#32437,#32438),(#32439,
#32440,#32441,#32442,#32443,#32444,#32445,#32446,#32447,#32448,#32449,#32450)),
 .UNSPECIFIED.,.F.,.F.,.F.)
B_SPLINE_SURFACE_WITH_KNOTS((4,4),(4,2,2,2,2,4),(0.,1.),(0.,0.0783698437311062,
0.30877738279783,0.539184921865219,0.76959246093261,1.),.UNSPECIFIED.)
GEOMETRIC_REPRESENTATION_ITEM()
RATIONAL_B_SPLINE_SURFACE(((1.,1.,1.,1.,1.,1.,1.,1.,1.,1.,1.,1.),(0.987189825241073,
0.987189825241073,0.987189825241073,0.987189825241073,0.987189825241073,
0.987189825241073,0.987189825241073,0.987189825241073,0.987189825241073,
0.987189825241073,0.987189825241073,0.987189825241073),(0.987189825241073,
0.987189825241073,0.987189825241073,0.987189825241073,0.987189825241073,
0.987189825241073,0.987189825241073,0.987189825241073,0.987189825241073,
0.987189825241073,0.987189825241073,0.987189825241073),(1.,1.,1.,1.,1.,
1.,1.,1.,1.,1.,1.,1.)))
REPRESENTATION_ITEM('')
SURFACE()
);
#505=(
BOUNDED_SURFACE()
B_SPLINE_SURFACE(3,3,((#32451,#32452,#32453,#32454,#32455,#32456,#32457,
#32458,#32459,#32460,#32461,#32462),(#32463,#32464,#32465,#32466,#32467,
#32468,#32469,#32470,#32471,#32472,#32473,#32474),(#32475,#32476,#32477,
#32478,#32479,#32480,#32481,#32482,#32483,#32484,#32485,#32486),(#32487,
#32488,#32489,#32490,#32491,#32492,#32493,#32494,#32495,#32496,#32497,#32498)),
 .UNSPECIFIED.,.F.,.F.,.F.)
B_SPLINE_SURFACE_WITH_KNOTS((4,4),(4,2,2,2,2,4),(0.,1.),(0.,0.0783698481609152,
0.308777386120187,0.539184924080123,0.769592462040061,1.),.UNSPECIFIED.)
GEOMETRIC_REPRESENTATION_ITEM()
RATIONAL_B_SPLINE_SURFACE(((1.,1.,1.,1.,1.,1.,1.,1.,1.,1.,1.,1.),(0.987189825241073,
0.987189825241073,0.987189825241073,0.987189825241073,0.987189825241073,
0.987189825241073,0.987189825241073,0.987189825241073,0.987189825241073,
0.987189825241073,0.987189825241073,0.987189825241073),(0.987189825241073,
0.987189825241073,0.987189825241073,0.987189825241073,0.987189825241073,
0.987189825241073,0.987189825241073,0.987189825241073,0.987189825241073,
0.987189825241073,0.987189825241073,0.987189825241073),(1.,1.,1.,1.,1.,
1.,1.,1.,1.,1.,1.,1.)))
REPRESENTATION_ITEM('')
SURFACE()
);
#506=(
BOUNDED_SURFACE()
B_SPLINE_SURFACE(3,3,((#32507,#32508,#32509,#32510,#32511,#32512,#32513,
#32514,#32515,#32516,#32517,#32518),(#32519,#32520,#32521,#32522,#32523,
#32524,#32525,#32526,#32527,#32528,#32529,#32530),(#32531,#32532,#32533,
#32534,#32535,#32536,#32537,#32538,#32539,#32540,#32541,#32542),(#32543,
#32544,#32545,#32546,#32547,#32548,#32549,#32550,#32551,#32552,#32553,#32554)),
 .UNSPECIFIED.,.F.,.F.,.F.)
B_SPLINE_SURFACE_WITH_KNOTS((4,4),(4,2,2,2,2,4),(0.,1.),(0.,0.0783698481609152,
0.308777386120187,0.539184924080123,0.769592462040061,1.),.UNSPECIFIED.)
GEOMETRIC_REPRESENTATION_ITEM()
RATIONAL_B_SPLINE_SURFACE(((1.,1.,1.,1.,1.,1.,1.,1.,1.,1.,1.,1.),(0.987189825241073,
0.987189825241073,0.987189825241073,0.987189825241073,0.987189825241073,
0.987189825241073,0.987189825241073,0.987189825241073,0.987189825241073,
0.987189825241073,0.987189825241073,0.987189825241073),(0.987189825241073,
0.987189825241073,0.987189825241073,0.987189825241073,0.987189825241073,
0.987189825241073,0.987189825241073,0.987189825241073,0.987189825241073,
0.987189825241073,0.987189825241073,0.987189825241073),(1.,1.,1.,1.,1.,
1.,1.,1.,1.,1.,1.,1.)))
REPRESENTATION_ITEM('')
SURFACE()
);
#507=(
BOUNDED_SURFACE()
B_SPLINE_SURFACE(3,3,((#32563,#32564,#32565,#32566,#32567,#32568,#32569,
#32570,#32571,#32572,#32573,#32574),(#32575,#32576,#32577,#32578,#32579,
#32580,#32581,#32582,#32583,#32584,#32585,#32586),(#32587,#32588,#32589,
#32590,#32591,#32592,#32593,#32594,#32595,#32596,#32597,#32598),(#32599,
#32600,#32601,#32602,#32603,#32604,#32605,#32606,#32607,#32608,#32609,#32610)),
 .UNSPECIFIED.,.F.,.F.,.F.)
B_SPLINE_SURFACE_WITH_KNOTS((4,4),(4,2,2,2,2,4),(0.,1.),(0.,0.0783698481609152,
0.308777386120187,0.539184924080123,0.769592462040061,1.),.UNSPECIFIED.)
GEOMETRIC_REPRESENTATION_ITEM()
RATIONAL_B_SPLINE_SURFACE(((1.,1.,1.,1.,1.,1.,1.,1.,1.,1.,1.,1.),(0.833333333333331,
0.833333333333331,0.833333333333331,0.833333333333331,0.833333333333331,
0.833333333333331,0.833333333333331,0.833333333333331,0.833333333333331,
0.833333333333331,0.833333333333331,0.833333333333331),(0.833333333333331,
0.833333333333331,0.833333333333331,0.833333333333331,0.833333333333331,
0.833333333333331,0.833333333333331,0.833333333333331,0.833333333333331,
0.833333333333331,0.833333333333331,0.833333333333331),(1.,1.,1.,1.,1.,
1.,1.,1.,1.,1.,1.,1.)))
REPRESENTATION_ITEM('')
SURFACE()
);
#508=(
BOUNDED_SURFACE()
B_SPLINE_SURFACE(3,3,((#32611,#32612,#32613,#32614,#32615,#32616,#32617,
#32618,#32619,#32620,#32621,#32622),(#32623,#32624,#32625,#32626,#32627,
#32628,#32629,#32630,#32631,#32632,#32633,#32634),(#32635,#32636,#32637,
#32638,#32639,#32640,#32641,#32642,#32643,#32644,#32645,#32646),(#32647,
#32648,#32649,#32650,#32651,#32652,#32653,#32654,#32655,#32656,#32657,#32658)),
 .UNSPECIFIED.,.F.,.F.,.F.)
B_SPLINE_SURFACE_WITH_KNOTS((4,4),(4,2,2,2,2,4),(0.,1.),(0.,0.0783698504851105,
0.308777387863333,0.539184925242221,0.76959246262111,1.),.UNSPECIFIED.)
GEOMETRIC_REPRESENTATION_ITEM()
RATIONAL_B_SPLINE_SURFACE(((1.,1.,1.,1.,1.,1.,1.,1.,1.,1.,1.,1.),(0.833333333333333,
0.833333333333333,0.833333333333333,0.833333333333333,0.833333333333333,
0.833333333333333,0.833333333333333,0.833333333333333,0.833333333333333,
0.833333333333333,0.833333333333333,0.833333333333333),(0.833333333333333,
0.833333333333333,0.833333333333333,0.833333333333333,0.833333333333333,
0.833333333333333,0.833333333333333,0.833333333333333,0.833333333333333,
0.833333333333333,0.833333333333333,0.833333333333333),(1.,1.,1.,1.,1.,
1.,1.,1.,1.,1.,1.,1.)))
REPRESENTATION_ITEM('')
SURFACE()
);
#509=(
BOUNDED_SURFACE()
B_SPLINE_SURFACE(3,3,((#32675,#32676,#32677,#32678,#32679,#32680,#32681,
#32682,#32683,#32684,#32685,#32686),(#32687,#32688,#32689,#32690,#32691,
#32692,#32693,#32694,#32695,#32696,#32697,#32698),(#32699,#32700,#32701,
#32702,#32703,#32704,#32705,#32706,#32707,#32708,#32709,#32710),(#32711,
#32712,#32713,#32714,#32715,#32716,#32717,#32718,#32719,#32720,#32721,#32722)),
 .UNSPECIFIED.,.F.,.F.,.F.)
B_SPLINE_SURFACE_WITH_KNOTS((4,4),(4,2,2,2,2,4),(0.,1.),(0.,0.0783698504851105,
0.308777387863333,0.539184925242221,0.76959246262111,1.),.UNSPECIFIED.)
GEOMETRIC_REPRESENTATION_ITEM()
RATIONAL_B_SPLINE_SURFACE(((1.,1.,1.,1.,1.,1.,1.,1.,1.,1.,1.,1.),(0.987189825241073,
0.987189825241073,0.987189825241073,0.987189825241073,0.987189825241073,
0.987189825241073,0.987189825241073,0.987189825241073,0.987189825241073,
0.987189825241073,0.987189825241073,0.987189825241073),(0.987189825241073,
0.987189825241073,0.987189825241073,0.987189825241073,0.987189825241073,
0.987189825241073,0.987189825241073,0.987189825241073,0.987189825241073,
0.987189825241073,0.987189825241073,0.987189825241073),(1.,1.,1.,1.,1.,
1.,1.,1.,1.,1.,1.,1.)))
REPRESENTATION_ITEM('')
SURFACE()
);
#510=(
BOUNDED_SURFACE()
B_SPLINE_SURFACE(3,3,((#32723,#32724,#32725,#32726,#32727,#32728,#32729,
#32730,#32731,#32732,#32733,#32734),(#32735,#32736,#32737,#32738,#32739,
#32740,#32741,#32742,#32743,#32744,#32745,#32746),(#32747,#32748,#32749,
#32750,#32751,#32752,#32753,#32754,#32755,#32756,#32757,#32758),(#32759,
#32760,#32761,#32762,#32763,#32764,#32765,#32766,#32767,#32768,#32769,#32770)),
 .UNSPECIFIED.,.F.,.F.,.F.)
B_SPLINE_SURFACE_WITH_KNOTS((4,4),(4,2,2,2,2,4),(0.,1.),(0.,0.0783698504851105,
0.308777387863333,0.539184925242221,0.76959246262111,1.),.UNSPECIFIED.)
GEOMETRIC_REPRESENTATION_ITEM()
RATIONAL_B_SPLINE_SURFACE(((1.,1.,1.,1.,1.,1.,1.,1.,1.,1.,1.,1.),(0.987189825241073,
0.987189825241073,0.987189825241073,0.987189825241073,0.987189825241073,
0.987189825241073,0.987189825241073,0.987189825241073,0.987189825241073,
0.987189825241073,0.987189825241073,0.987189825241073),(0.987189825241073,
0.987189825241073,0.987189825241073,0.987189825241073,0.987189825241073,
0.987189825241073,0.987189825241073,0.987189825241073,0.987189825241073,
0.987189825241073,0.987189825241073,0.987189825241073),(1.,1.,1.,1.,1.,
1.,1.,1.,1.,1.,1.,1.)))
REPRESENTATION_ITEM('')
SURFACE()
);
#511=(
BOUNDED_SURFACE()
B_SPLINE_SURFACE(3,3,((#32771,#32772,#32773,#32774,#32775,#32776,#32777,
#32778,#32779,#32780,#32781,#32782),(#32783,#32784,#32785,#32786,#32787,
#32788,#32789,#32790,#32791,#32792,#32793,#32794),(#32795,#32796,#32797,
#32798,#32799,#32800,#32801,#32802,#32803,#32804,#32805,#32806),(#32807,
#32808,#32809,#32810,#32811,#32812,#32813,#32814,#32815,#32816,#32817,#32818)),
 .UNSPECIFIED.,.F.,.F.,.F.)
B_SPLINE_SURFACE_WITH_KNOTS((4,4),(4,2,2,2,2,4),(0.,1.),(0.,0.0783698504851009,
0.308777387863326,0.539184925242216,0.769592462621108,1.),.UNSPECIFIED.)
GEOMETRIC_REPRESENTATION_ITEM()
RATIONAL_B_SPLINE_SURFACE(((1.,1.,1.,1.,1.,1.,1.,1.,1.,1.,1.,1.),(0.833333333333333,
0.833333333333333,0.833333333333333,0.833333333333333,0.833333333333333,
0.833333333333333,0.833333333333333,0.833333333333333,0.833333333333333,
0.833333333333333,0.833333333333333,0.833333333333333),(0.833333333333333,
0.833333333333333,0.833333333333333,0.833333333333333,0.833333333333333,
0.833333333333333,0.833333333333333,0.833333333333333,0.833333333333333,
0.833333333333333,0.833333333333333,0.833333333333333),(1.,1.,1.,1.,1.,
1.,1.,1.,1.,1.,1.,1.)))
REPRESENTATION_ITEM('')
SURFACE()
);
#512=(
BOUNDED_SURFACE()
B_SPLINE_SURFACE(3,3,((#32835,#32836,#32837,#32838,#32839,#32840,#32841,
#32842,#32843,#32844,#32845,#32846),(#32847,#32848,#32849,#32850,#32851,
#32852,#32853,#32854,#32855,#32856,#32857,#32858),(#32859,#32860,#32861,
#32862,#32863,#32864,#32865,#32866,#32867,#32868,#32869,#32870),(#32871,
#32872,#32873,#32874,#32875,#32876,#32877,#32878,#32879,#32880,#32881,#32882)),
 .UNSPECIFIED.,.F.,.F.,.F.)
B_SPLINE_SURFACE_WITH_KNOTS((4,4),(4,2,2,2,2,4),(0.,1.),(0.,0.0783698504851009,
0.308777387863326,0.539184925242216,0.769592462621108,1.),.UNSPECIFIED.)
GEOMETRIC_REPRESENTATION_ITEM()
RATIONAL_B_SPLINE_SURFACE(((1.,1.,1.,1.,1.,1.,1.,1.,1.,1.,1.,1.),(0.987189825241073,
0.987189825241073,0.987189825241073,0.987189825241073,0.987189825241073,
0.987189825241073,0.987189825241073,0.987189825241073,0.987189825241073,
0.987189825241073,0.987189825241073,0.987189825241073),(0.987189825241073,
0.987189825241073,0.987189825241073,0.987189825241073,0.987189825241073,
0.987189825241073,0.987189825241073,0.987189825241073,0.987189825241073,
0.987189825241073,0.987189825241073,0.987189825241073),(1.,1.,1.,1.,1.,
1.,1.,1.,1.,1.,1.,1.)))
REPRESENTATION_ITEM('')
SURFACE()
);
#513=(
BOUNDED_SURFACE()
B_SPLINE_SURFACE(3,3,((#32883,#32884,#32885,#32886,#32887,#32888,#32889,
#32890,#32891,#32892,#32893,#32894),(#32895,#32896,#32897,#32898,#32899,
#32900,#32901,#32902,#32903,#32904,#32905,#32906),(#32907,#32908,#32909,
#32910,#32911,#32912,#32913,#32914,#32915,#32916,#32917,#32918),(#32919,
#32920,#32921,#32922,#32923,#32924,#32925,#32926,#32927,#32928,#32929,#32930)),
 .UNSPECIFIED.,.F.,.F.,.F.)
B_SPLINE_SURFACE_WITH_KNOTS((4,4),(4,2,2,2,2,4),(0.,1.),(0.,0.0783698504851009,
0.308777387863326,0.539184925242216,0.769592462621108,1.),.UNSPECIFIED.)
GEOMETRIC_REPRESENTATION_ITEM()
RATIONAL_B_SPLINE_SURFACE(((1.,1.,1.,1.,1.,1.,1.,1.,1.,1.,1.,1.),(0.987189825241073,
0.987189825241073,0.987189825241073,0.987189825241073,0.987189825241073,
0.987189825241073,0.987189825241073,0.987189825241073,0.987189825241073,
0.987189825241073,0.987189825241073,0.987189825241073),(0.987189825241073,
0.987189825241073,0.987189825241073,0.987189825241073,0.987189825241073,
0.987189825241073,0.987189825241073,0.987189825241073,0.987189825241073,
0.987189825241073,0.987189825241073,0.987189825241073),(1.,1.,1.,1.,1.,
1.,1.,1.,1.,1.,1.,1.)))
REPRESENTATION_ITEM('')
SURFACE()
);
#514=(
BOUNDED_SURFACE()
B_SPLINE_SURFACE(3,3,((#32931,#32932,#32933,#32934,#32935,#32936,#32937,
#32938,#32939,#32940,#32941,#32942),(#32943,#32944,#32945,#32946,#32947,
#32948,#32949,#32950,#32951,#32952,#32953,#32954),(#32955,#32956,#32957,
#32958,#32959,#32960,#32961,#32962,#32963,#32964,#32965,#32966),(#32967,
#32968,#32969,#32970,#32971,#32972,#32973,#32974,#32975,#32976,#32977,#32978)),
 .UNSPECIFIED.,.F.,.F.,.F.)
B_SPLINE_SURFACE_WITH_KNOTS((4,4),(4,2,2,2,2,4),(0.,1.),(0.,0.0783698481609159,
0.308777386120187,0.539184924080124,0.769592462040061,1.),.UNSPECIFIED.)
GEOMETRIC_REPRESENTATION_ITEM()
RATIONAL_B_SPLINE_SURFACE(((1.,1.,1.,1.,1.,1.,1.,1.,1.,1.,1.,1.),(0.833333333333332,
0.833333333333332,0.833333333333332,0.833333333333332,0.833333333333332,
0.833333333333332,0.833333333333332,0.833333333333332,0.833333333333332,
0.833333333333332,0.833333333333332,0.833333333333332),(0.833333333333332,
0.833333333333332,0.833333333333332,0.833333333333332,0.833333333333332,
0.833333333333332,0.833333333333332,0.833333333333332,0.833333333333332,
0.833333333333332,0.833333333333332,0.833333333333332),(1.,1.,1.,1.,1.,
1.,1.,1.,1.,1.,1.,1.)))
REPRESENTATION_ITEM('')
SURFACE()
);
#515=(
BOUNDED_SURFACE()
B_SPLINE_SURFACE(3,3,((#32995,#32996,#32997,#32998,#32999,#33000,#33001,
#33002,#33003,#33004,#33005,#33006),(#33007,#33008,#33009,#33010,#33011,
#33012,#33013,#33014,#33015,#33016,#33017,#33018),(#33019,#33020,#33021,
#33022,#33023,#33024,#33025,#33026,#33027,#33028,#33029,#33030),(#33031,
#33032,#33033,#33034,#33035,#33036,#33037,#33038,#33039,#33040,#33041,#33042)),
 .UNSPECIFIED.,.F.,.F.,.F.)
B_SPLINE_SURFACE_WITH_KNOTS((4,4),(4,2,2,2,2,4),(0.,1.),(0.,0.0783698481609159,
0.308777386120187,0.539184924080124,0.769592462040061,1.),.UNSPECIFIED.)
GEOMETRIC_REPRESENTATION_ITEM()
RATIONAL_B_SPLINE_SURFACE(((1.,1.,1.,1.,1.,1.,1.,1.,1.,1.,1.,1.),(0.987189825241073,
0.987189825241073,0.987189825241073,0.987189825241073,0.987189825241073,
0.987189825241073,0.987189825241073,0.987189825241073,0.987189825241073,
0.987189825241073,0.987189825241073,0.987189825241073),(0.987189825241073,
0.987189825241073,0.987189825241073,0.987189825241073,0.987189825241073,
0.987189825241073,0.987189825241073,0.987189825241073,0.987189825241073,
0.987189825241073,0.987189825241073,0.987189825241073),(1.,1.,1.,1.,1.,
1.,1.,1.,1.,1.,1.,1.)))
REPRESENTATION_ITEM('')
SURFACE()
);
#516=(
BOUNDED_SURFACE()
B_SPLINE_SURFACE(3,3,((#33043,#33044,#33045,#33046,#33047,#33048,#33049,
#33050,#33051,#33052,#33053,#33054),(#33055,#33056,#33057,#33058,#33059,
#33060,#33061,#33062,#33063,#33064,#33065,#33066),(#33067,#33068,#33069,
#33070,#33071,#33072,#33073,#33074,#33075,#33076,#33077,#33078),(#33079,
#33080,#33081,#33082,#33083,#33084,#33085,#33086,#33087,#33088,#33089,#33090)),
 .UNSPECIFIED.,.F.,.F.,.F.)
B_SPLINE_SURFACE_WITH_KNOTS((4,4),(4,2,2,2,2,4),(0.,1.),(0.,0.0783698481609159,
0.308777386120187,0.539184924080124,0.769592462040061,1.),.UNSPECIFIED.)
GEOMETRIC_REPRESENTATION_ITEM()
RATIONAL_B_SPLINE_SURFACE(((1.,1.,1.,1.,1.,1.,1.,1.,1.,1.,1.,1.),(0.987189825241073,
0.987189825241073,0.987189825241073,0.987189825241073,0.987189825241073,
0.987189825241073,0.987189825241073,0.987189825241073,0.987189825241073,
0.987189825241073,0.987189825241073,0.987189825241073),(0.987189825241073,
0.987189825241073,0.987189825241073,0.987189825241073,0.987189825241073,
0.987189825241073,0.987189825241073,0.987189825241073,0.987189825241073,
0.987189825241073,0.987189825241073,0.987189825241073),(1.,1.,1.,1.,1.,
1.,1.,1.,1.,1.,1.,1.)))
REPRESENTATION_ITEM('')
SURFACE()
);
#517=(
BOUNDED_SURFACE()
B_SPLINE_SURFACE(3,3,((#33091,#33092,#33093,#33094,#33095,#33096,#33097,
#33098,#33099,#33100,#33101,#33102),(#33103,#33104,#33105,#33106,#33107,
#33108,#33109,#33110,#33111,#33112,#33113,#33114),(#33115,#33116,#33117,
#33118,#33119,#33120,#33121,#33122,#33123,#33124,#33125,#33126),(#33127,
#33128,#33129,#33130,#33131,#33132,#33133,#33134,#33135,#33136,#33137,#33138)),
 .UNSPECIFIED.,.F.,.F.,.F.)
B_SPLINE_SURFACE_WITH_KNOTS((4,4),(4,2,2,2,2,4),(0.,1.),(0.,0.0783698437310911,
0.308777382797819,0.539184921865211,0.769592460932606,1.),.UNSPECIFIED.)
GEOMETRIC_REPRESENTATION_ITEM()
RATIONAL_B_SPLINE_SURFACE(((1.,1.,1.,1.,1.,1.,1.,1.,1.,1.,1.,1.),(0.833333333333333,
0.833333333333333,0.833333333333333,0.833333333333333,0.833333333333333,
0.833333333333333,0.833333333333333,0.833333333333333,0.833333333333333,
0.833333333333333,0.833333333333333,0.833333333333333),(0.833333333333333,
0.833333333333333,0.833333333333333,0.833333333333333,0.833333333333333,
0.833333333333333,0.833333333333333,0.833333333333333,0.833333333333333,
0.833333333333333,0.833333333333333,0.833333333333333),(1.,1.,1.,1.,1.,
1.,1.,1.,1.,1.,1.,1.)))
REPRESENTATION_ITEM('')
SURFACE()
);
#518=(
BOUNDED_SURFACE()
B_SPLINE_SURFACE(3,3,((#33155,#33156,#33157,#33158,#33159,#33160,#33161,
#33162,#33163,#33164,#33165,#33166),(#33167,#33168,#33169,#33170,#33171,
#33172,#33173,#33174,#33175,#33176,#33177,#33178),(#33179,#33180,#33181,
#33182,#33183,#33184,#33185,#33186,#33187,#33188,#33189,#33190),(#33191,
#33192,#33193,#33194,#33195,#33196,#33197,#33198,#33199,#33200,#33201,#33202)),
 .UNSPECIFIED.,.F.,.F.,.F.)
B_SPLINE_SURFACE_WITH_KNOTS((4,4),(4,2,2,2,2,4),(0.,1.),(0.,0.0783698437310911,
0.308777382797819,0.539184921865211,0.769592460932606,1.),.UNSPECIFIED.)
GEOMETRIC_REPRESENTATION_ITEM()
RATIONAL_B_SPLINE_SURFACE(((1.,1.,1.,1.,1.,1.,1.,1.,1.,1.,1.,1.),(0.987189825241073,
0.987189825241073,0.987189825241073,0.987189825241073,0.987189825241073,
0.987189825241073,0.987189825241073,0.987189825241073,0.987189825241073,
0.987189825241073,0.987189825241073,0.987189825241073),(0.987189825241073,
0.987189825241073,0.987189825241073,0.987189825241073,0.987189825241073,
0.987189825241073,0.987189825241073,0.987189825241073,0.987189825241073,
0.987189825241073,0.987189825241073,0.987189825241073),(1.,1.,1.,1.,1.,
1.,1.,1.,1.,1.,1.,1.)))
REPRESENTATION_ITEM('')
SURFACE()
);
#519=(
BOUNDED_SURFACE()
B_SPLINE_SURFACE(3,3,((#33203,#33204,#33205,#33206,#33207,#33208,#33209,
#33210,#33211,#33212,#33213,#33214),(#33215,#33216,#33217,#33218,#33219,
#33220,#33221,#33222,#33223,#33224,#33225,#33226),(#33227,#33228,#33229,
#33230,#33231,#33232,#33233,#33234,#33235,#33236,#33237,#33238),(#33239,
#33240,#33241,#33242,#33243,#33244,#33245,#33246,#33247,#33248,#33249,#33250)),
 .UNSPECIFIED.,.F.,.F.,.F.)
B_SPLINE_SURFACE_WITH_KNOTS((4,4),(4,2,2,2,2,4),(0.,1.),(0.,0.0783698437310911,
0.308777382797819,0.539184921865211,0.769592460932606,1.),.UNSPECIFIED.)
GEOMETRIC_REPRESENTATION_ITEM()
RATIONAL_B_SPLINE_SURFACE(((1.,1.,1.,1.,1.,1.,1.,1.,1.,1.,1.,1.),(0.987189825241073,
0.987189825241073,0.987189825241073,0.987189825241073,0.987189825241073,
0.987189825241073,0.987189825241073,0.987189825241073,0.987189825241073,
0.987189825241073,0.987189825241073,0.987189825241073),(0.987189825241073,
0.987189825241073,0.987189825241073,0.987189825241073,0.987189825241073,
0.987189825241073,0.987189825241073,0.987189825241073,0.987189825241073,
0.987189825241073,0.987189825241073,0.987189825241073),(1.,1.,1.,1.,1.,
1.,1.,1.,1.,1.,1.,1.)))
REPRESENTATION_ITEM('')
SURFACE()
);
#520=(
BOUNDED_SURFACE()
B_SPLINE_SURFACE(3,3,((#33251,#33252,#33253,#33254,#33255,#33256,#33257,
#33258,#33259,#33260,#33261,#33262),(#33263,#33264,#33265,#33266,#33267,
#33268,#33269,#33270,#33271,#33272,#33273,#33274),(#33275,#33276,#33277,
#33278,#33279,#33280,#33281,#33282,#33283,#33284,#33285,#33286),(#33287,
#33288,#33289,#33290,#33291,#33292,#33293,#33294,#33295,#33296,#33297,#33298)),
 .UNSPECIFIED.,.F.,.F.,.F.)
B_SPLINE_SURFACE_WITH_KNOTS((4,4),(4,2,2,2,2,4),(0.,1.),(0.,0.0783698388401225,
0.308777379129592,0.539184919419727,0.769592459709863,1.),.UNSPECIFIED.)
GEOMETRIC_REPRESENTATION_ITEM()
RATIONAL_B_SPLINE_SURFACE(((1.,1.,1.,1.,1.,1.,1.,1.,1.,1.,1.,1.),(0.833333333333332,
0.833333333333332,0.833333333333332,0.833333333333332,0.833333333333332,
0.833333333333332,0.833333333333332,0.833333333333332,0.833333333333332,
0.833333333333332,0.833333333333332,0.833333333333332),(0.833333333333332,
0.833333333333332,0.833333333333332,0.833333333333332,0.833333333333332,
0.833333333333332,0.833333333333332,0.833333333333332,0.833333333333332,
0.833333333333332,0.833333333333332,0.833333333333332),(1.,1.,1.,1.,1.,
1.,1.,1.,1.,1.,1.,1.)))
REPRESENTATION_ITEM('')
SURFACE()
);
#521=(
BOUNDED_SURFACE()
B_SPLINE_SURFACE(3,3,((#33315,#33316,#33317,#33318,#33319,#33320,#33321,
#33322,#33323,#33324,#33325,#33326),(#33327,#33328,#33329,#33330,#33331,
#33332,#33333,#33334,#33335,#33336,#33337,#33338),(#33339,#33340,#33341,
#33342,#33343,#33344,#33345,#33346,#33347,#33348,#33349,#33350),(#33351,
#33352,#33353,#33354,#33355,#33356,#33357,#33358,#33359,#33360,#33361,#33362)),
 .UNSPECIFIED.,.F.,.F.,.F.)
B_SPLINE_SURFACE_WITH_KNOTS((4,4),(4,2,2,2,2,4),(0.,1.),(0.,0.0783698388401225,
0.308777379129592,0.539184919419727,0.769592459709863,1.),.UNSPECIFIED.)
GEOMETRIC_REPRESENTATION_ITEM()
RATIONAL_B_SPLINE_SURFACE(((1.,1.,1.,1.,1.,1.,1.,1.,1.,1.,1.,1.),(0.987189825241073,
0.987189825241073,0.987189825241073,0.987189825241073,0.987189825241073,
0.987189825241073,0.987189825241073,0.987189825241073,0.987189825241073,
0.987189825241073,0.987189825241073,0.987189825241073),(0.987189825241073,
0.987189825241073,0.987189825241073,0.987189825241073,0.987189825241073,
0.987189825241073,0.987189825241073,0.987189825241073,0.987189825241073,
0.987189825241073,0.987189825241073,0.987189825241073),(1.,1.,1.,1.,1.,
1.,1.,1.,1.,1.,1.,1.)))
REPRESENTATION_ITEM('')
SURFACE()
);
#522=(
BOUNDED_SURFACE()
B_SPLINE_SURFACE(3,3,((#33363,#33364,#33365,#33366,#33367,#33368,#33369,
#33370,#33371,#33372,#33373,#33374),(#33375,#33376,#33377,#33378,#33379,
#33380,#33381,#33382,#33383,#33384,#33385,#33386),(#33387,#33388,#33389,
#33390,#33391,#33392,#33393,#33394,#33395,#33396,#33397,#33398),(#33399,
#33400,#33401,#33402,#33403,#33404,#33405,#33406,#33407,#33408,#33409,#33410)),
 .UNSPECIFIED.,.F.,.F.,.F.)
B_SPLINE_SURFACE_WITH_KNOTS((4,4),(4,2,2,2,2,4),(0.,1.),(0.,0.0783698388401225,
0.308777379129592,0.539184919419727,0.769592459709863,1.),.UNSPECIFIED.)
GEOMETRIC_REPRESENTATION_ITEM()
RATIONAL_B_SPLINE_SURFACE(((1.,1.,1.,1.,1.,1.,1.,1.,1.,1.,1.,1.),(0.987189825241073,
0.987189825241073,0.987189825241073,0.987189825241073,0.987189825241073,
0.987189825241073,0.987189825241073,0.987189825241073,0.987189825241073,
0.987189825241073,0.987189825241073,0.987189825241073),(0.987189825241073,
0.987189825241073,0.987189825241073,0.987189825241073,0.987189825241073,
0.987189825241073,0.987189825241073,0.987189825241073,0.987189825241073,
0.987189825241073,0.987189825241073,0.987189825241073),(1.,1.,1.,1.,1.,
1.,1.,1.,1.,1.,1.,1.)))
REPRESENTATION_ITEM('')
SURFACE()
);
#523=(
BOUNDED_SURFACE()
B_SPLINE_SURFACE(3,3,((#33411,#33412,#33413,#33414,#33415,#33416,#33417,
#33418,#33419,#33420,#33421,#33422),(#33423,#33424,#33425,#33426,#33427,
#33428,#33429,#33430,#33431,#33432,#33433,#33434),(#33435,#33436,#33437,
#33438,#33439,#33440,#33441,#33442,#33443,#33444,#33445,#33446),(#33447,
#33448,#33449,#33450,#33451,#33452,#33453,#33454,#33455,#33456,#33457,#33458)),
 .UNSPECIFIED.,.F.,.F.,.F.)
B_SPLINE_SURFACE_WITH_KNOTS((4,4),(4,2,2,2,2,4),(0.,1.),(0.,0.078369835250435,
0.308777376437327,0.539184917624883,0.769592458812442,1.),.UNSPECIFIED.)
GEOMETRIC_REPRESENTATION_ITEM()
RATIONAL_B_SPLINE_SURFACE(((1.,1.,1.,1.,1.,1.,1.,1.,1.,1.,1.,1.),(0.833333333333333,
0.833333333333333,0.833333333333333,0.833333333333333,0.833333333333333,
0.833333333333333,0.833333333333333,0.833333333333333,0.833333333333333,
0.833333333333333,0.833333333333333,0.833333333333333),(0.833333333333333,
0.833333333333333,0.833333333333333,0.833333333333333,0.833333333333333,
0.833333333333333,0.833333333333333,0.833333333333333,0.833333333333333,
0.833333333333333,0.833333333333333,0.833333333333333),(1.,1.,1.,1.,1.,
1.,1.,1.,1.,1.,1.,1.)))
REPRESENTATION_ITEM('')
SURFACE()
);
#524=(
BOUNDED_SURFACE()
B_SPLINE_SURFACE(3,3,((#33475,#33476,#33477,#33478,#33479,#33480,#33481,
#33482,#33483,#33484,#33485,#33486),(#33487,#33488,#33489,#33490,#33491,
#33492,#33493,#33494,#33495,#33496,#33497,#33498),(#33499,#33500,#33501,
#33502,#33503,#33504,#33505,#33506,#33507,#33508,#33509,#33510),(#33511,
#33512,#33513,#33514,#33515,#33516,#33517,#33518,#33519,#33520,#33521,#33522)),
 .UNSPECIFIED.,.F.,.F.,.F.)
B_SPLINE_SURFACE_WITH_KNOTS((4,4),(4,2,2,2,2,4),(0.,1.),(0.,0.078369835250435,
0.308777376437327,0.539184917624883,0.769592458812442,1.),.UNSPECIFIED.)
GEOMETRIC_REPRESENTATION_ITEM()
RATIONAL_B_SPLINE_SURFACE(((1.,1.,1.,1.,1.,1.,1.,1.,1.,1.,1.,1.),(0.987189825241073,
0.987189825241073,0.987189825241073,0.987189825241073,0.987189825241073,
0.987189825241073,0.987189825241073,0.987189825241073,0.987189825241073,
0.987189825241073,0.987189825241073,0.987189825241073),(0.987189825241073,
0.987189825241073,0.987189825241073,0.987189825241073,0.987189825241073,
0.987189825241073,0.987189825241073,0.987189825241073,0.987189825241073,
0.987189825241073,0.987189825241073,0.987189825241073),(1.,1.,1.,1.,1.,
1.,1.,1.,1.,1.,1.,1.)))
REPRESENTATION_ITEM('')
SURFACE()
);
#525=(
BOUNDED_SURFACE()
B_SPLINE_SURFACE(3,3,((#33523,#33524,#33525,#33526,#33527,#33528,#33529,
#33530,#33531,#33532,#33533,#33534),(#33535,#33536,#33537,#33538,#33539,
#33540,#33541,#33542,#33543,#33544,#33545,#33546),(#33547,#33548,#33549,
#33550,#33551,#33552,#33553,#33554,#33555,#33556,#33557,#33558),(#33559,
#33560,#33561,#33562,#33563,#33564,#33565,#33566,#33567,#33568,#33569,#33570)),
 .UNSPECIFIED.,.F.,.F.,.F.)
B_SPLINE_SURFACE_WITH_KNOTS((4,4),(4,2,2,2,2,4),(0.,1.),(0.,0.078369835250435,
0.308777376437327,0.539184917624883,0.769592458812442,1.),.UNSPECIFIED.)
GEOMETRIC_REPRESENTATION_ITEM()
RATIONAL_B_SPLINE_SURFACE(((1.,1.,1.,1.,1.,1.,1.,1.,1.,1.,1.,1.),(0.987189825241073,
0.987189825241073,0.987189825241073,0.987189825241073,0.987189825241073,
0.987189825241073,0.987189825241073,0.987189825241073,0.987189825241073,
0.987189825241073,0.987189825241073,0.987189825241073),(0.987189825241073,
0.987189825241073,0.987189825241073,0.987189825241073,0.987189825241073,
0.987189825241073,0.987189825241073,0.987189825241073,0.987189825241073,
0.987189825241073,0.987189825241073,0.987189825241073),(1.,1.,1.,1.,1.,
1.,1.,1.,1.,1.,1.,1.)))
REPRESENTATION_ITEM('')
SURFACE()
);
#526=(
BOUNDED_SURFACE()
B_SPLINE_SURFACE(3,3,((#33571,#33572,#33573,#33574,#33575,#33576,#33577,
#33578,#33579,#33580,#33581,#33582),(#33583,#33584,#33585,#33586,#33587,
#33588,#33589,#33590,#33591,#33592,#33593,#33594),(#33595,#33596,#33597,
#33598,#33599,#33600,#33601,#33602,#33603,#33604,#33605,#33606),(#33607,
#33608,#33609,#33610,#33611,#33612,#33613,#33614,#33615,#33616,#33617,#33618)),
 .UNSPECIFIED.,.F.,.F.,.F.)
B_SPLINE_SURFACE_WITH_KNOTS((4,4),(4,2,2,2,2,4),(0.,1.),(0.,0.0783698293107414,
0.308777371982556,0.539184914655036,0.769592457327518,1.),.UNSPECIFIED.)
GEOMETRIC_REPRESENTATION_ITEM()
RATIONAL_B_SPLINE_SURFACE(((1.,1.,1.,1.,1.,1.,1.,1.,1.,1.,1.,1.),(0.833333333333332,
0.833333333333332,0.833333333333332,0.833333333333332,0.833333333333332,
0.833333333333332,0.833333333333332,0.833333333333332,0.833333333333332,
0.833333333333332,0.833333333333332,0.833333333333332),(0.833333333333332,
0.833333333333332,0.833333333333332,0.833333333333332,0.833333333333332,
0.833333333333332,0.833333333333332,0.833333333333332,0.833333333333332,
0.833333333333332,0.833333333333332,0.833333333333332),(1.,1.,1.,1.,1.,
1.,1.,1.,1.,1.,1.,1.)))
REPRESENTATION_ITEM('')
SURFACE()
);
#527=(
BOUNDED_SURFACE()
B_SPLINE_SURFACE(3,3,((#33635,#33636,#33637,#33638,#33639,#33640,#33641,
#33642,#33643,#33644,#33645,#33646),(#33647,#33648,#33649,#33650,#33651,
#33652,#33653,#33654,#33655,#33656,#33657,#33658),(#33659,#33660,#33661,
#33662,#33663,#33664,#33665,#33666,#33667,#33668,#33669,#33670),(#33671,
#33672,#33673,#33674,#33675,#33676,#33677,#33678,#33679,#33680,#33681,#33682)),
 .UNSPECIFIED.,.F.,.F.,.F.)
B_SPLINE_SURFACE_WITH_KNOTS((4,4),(4,2,2,2,2,4),(0.,1.),(0.,0.0783698293107414,
0.308777371982556,0.539184914655036,0.769592457327518,1.),.UNSPECIFIED.)
GEOMETRIC_REPRESENTATION_ITEM()
RATIONAL_B_SPLINE_SURFACE(((1.,1.,1.,1.,1.,1.,1.,1.,1.,1.,1.,1.),(0.987189825241073,
0.987189825241073,0.987189825241073,0.987189825241073,0.987189825241073,
0.987189825241073,0.987189825241073,0.987189825241073,0.987189825241073,
0.987189825241073,0.987189825241073,0.987189825241073),(0.987189825241073,
0.987189825241073,0.987189825241073,0.987189825241073,0.987189825241073,
0.987189825241073,0.987189825241073,0.987189825241073,0.987189825241073,
0.987189825241073,0.987189825241073,0.987189825241073),(1.,1.,1.,1.,1.,
1.,1.,1.,1.,1.,1.,1.)))
REPRESENTATION_ITEM('')
SURFACE()
);
#528=(
BOUNDED_SURFACE()
B_SPLINE_SURFACE(3,3,((#33683,#33684,#33685,#33686,#33687,#33688,#33689,
#33690,#33691,#33692,#33693,#33694),(#33695,#33696,#33697,#33698,#33699,
#33700,#33701,#33702,#33703,#33704,#33705,#33706),(#33707,#33708,#33709,
#33710,#33711,#33712,#33713,#33714,#33715,#33716,#33717,#33718),(#33719,
#33720,#33721,#33722,#33723,#33724,#33725,#33726,#33727,#33728,#33729,#33730)),
 .UNSPECIFIED.,.F.,.F.,.F.)
B_SPLINE_SURFACE_WITH_KNOTS((4,4),(4,2,2,2,2,4),(0.,1.),(0.,0.0783698293107414,
0.308777371982556,0.539184914655036,0.769592457327518,1.),.UNSPECIFIED.)
GEOMETRIC_REPRESENTATION_ITEM()
RATIONAL_B_SPLINE_SURFACE(((1.,1.,1.,1.,1.,1.,1.,1.,1.,1.,1.,1.),(0.987189825241073,
0.987189825241073,0.987189825241073,0.987189825241073,0.987189825241073,
0.987189825241073,0.987189825241073,0.987189825241073,0.987189825241073,
0.987189825241073,0.987189825241073,0.987189825241073),(0.987189825241073,
0.987189825241073,0.987189825241073,0.987189825241073,0.987189825241073,
0.987189825241073,0.987189825241073,0.987189825241073,0.987189825241073,
0.987189825241073,0.987189825241073,0.987189825241073),(1.,1.,1.,1.,1.,
1.,1.,1.,1.,1.,1.,1.)))
REPRESENTATION_ITEM('')
SURFACE()
);
#529=(
BOUNDED_SURFACE()
B_SPLINE_SURFACE(3,3,((#33731,#33732,#33733,#33734,#33735,#33736,#33737,
#33738,#33739,#33740,#33741,#33742),(#33743,#33744,#33745,#33746,#33747,
#33748,#33749,#33750,#33751,#33752,#33753,#33754),(#33755,#33756,#33757,
#33758,#33759,#33760,#33761,#33762,#33763,#33764,#33765,#33766),(#33767,
#33768,#33769,#33770,#33771,#33772,#33773,#33774,#33775,#33776,#33777,#33778)),
 .UNSPECIFIED.,.F.,.F.,.F.)
B_SPLINE_SURFACE_WITH_KNOTS((4,4),(4,2,2,2,2,4),(0.,1.),(0.,0.0783698352504223,
0.308777376437317,0.539184917624877,0.769592458812438,1.),.UNSPECIFIED.)
GEOMETRIC_REPRESENTATION_ITEM()
RATIONAL_B_SPLINE_SURFACE(((1.,1.,1.,1.,1.,1.,1.,1.,1.,1.,1.,1.),(0.833333333333332,
0.833333333333332,0.833333333333332,0.833333333333332,0.833333333333332,
0.833333333333332,0.833333333333332,0.833333333333332,0.833333333333332,
0.833333333333332,0.833333333333332,0.833333333333332),(0.833333333333332,
0.833333333333332,0.833333333333332,0.833333333333332,0.833333333333332,
0.833333333333332,0.833333333333332,0.833333333333332,0.833333333333332,
0.833333333333332,0.833333333333332,0.833333333333332),(1.,1.,1.,1.,1.,
1.,1.,1.,1.,1.,1.,1.)))
REPRESENTATION_ITEM('')
SURFACE()
);
#530=(
BOUNDED_SURFACE()
B_SPLINE_SURFACE(3,3,((#33795,#33796,#33797,#33798,#33799,#33800,#33801,
#33802,#33803,#33804,#33805,#33806),(#33807,#33808,#33809,#33810,#33811,
#33812,#33813,#33814,#33815,#33816,#33817,#33818),(#33819,#33820,#33821,
#33822,#33823,#33824,#33825,#33826,#33827,#33828,#33829,#33830),(#33831,
#33832,#33833,#33834,#33835,#33836,#33837,#33838,#33839,#33840,#33841,#33842)),
 .UNSPECIFIED.,.F.,.F.,.F.)
B_SPLINE_SURFACE_WITH_KNOTS((4,4),(4,2,2,2,2,4),(0.,1.),(0.,0.0783698352504223,
0.308777376437317,0.539184917624877,0.769592458812438,1.),.UNSPECIFIED.)
GEOMETRIC_REPRESENTATION_ITEM()
RATIONAL_B_SPLINE_SURFACE(((1.,1.,1.,1.,1.,1.,1.,1.,1.,1.,1.,1.),(0.987189825241073,
0.987189825241073,0.987189825241073,0.987189825241073,0.987189825241073,
0.987189825241073,0.987189825241073,0.987189825241073,0.987189825241073,
0.987189825241073,0.987189825241073,0.987189825241073),(0.987189825241073,
0.987189825241073,0.987189825241073,0.987189825241073,0.987189825241073,
0.987189825241073,0.987189825241073,0.987189825241073,0.987189825241073,
0.987189825241073,0.987189825241073,0.987189825241073),(1.,1.,1.,1.,1.,
1.,1.,1.,1.,1.,1.,1.)))
REPRESENTATION_ITEM('')
SURFACE()
);
#531=(
BOUNDED_SURFACE()
B_SPLINE_SURFACE(3,3,((#33843,#33844,#33845,#33846,#33847,#33848,#33849,
#33850,#33851,#33852,#33853,#33854),(#33855,#33856,#33857,#33858,#33859,
#33860,#33861,#33862,#33863,#33864,#33865,#33866),(#33867,#33868,#33869,
#33870,#33871,#33872,#33873,#33874,#33875,#33876,#33877,#33878),(#33879,
#33880,#33881,#33882,#33883,#33884,#33885,#33886,#33887,#33888,#33889,#33890)),
 .UNSPECIFIED.,.F.,.F.,.F.)
B_SPLINE_SURFACE_WITH_KNOTS((4,4),(4,2,2,2,2,4),(0.,1.),(0.,0.0783698352504223,
0.308777376437317,0.539184917624877,0.769592458812438,1.),.UNSPECIFIED.)
GEOMETRIC_REPRESENTATION_ITEM()
RATIONAL_B_SPLINE_SURFACE(((1.,1.,1.,1.,1.,1.,1.,1.,1.,1.,1.,1.),(0.987189825241073,
0.987189825241073,0.987189825241073,0.987189825241073,0.987189825241073,
0.987189825241073,0.987189825241073,0.987189825241073,0.987189825241073,
0.987189825241073,0.987189825241073,0.987189825241073),(0.987189825241073,
0.987189825241073,0.987189825241073,0.987189825241073,0.987189825241073,
0.987189825241073,0.987189825241073,0.987189825241073,0.987189825241073,
0.987189825241073,0.987189825241073,0.987189825241073),(1.,1.,1.,1.,1.,
1.,1.,1.,1.,1.,1.,1.)))
REPRESENTATION_ITEM('')
SURFACE()
);
#532=(
BOUNDED_SURFACE()
B_SPLINE_SURFACE(3,3,((#33891,#33892,#33893,#33894,#33895,#33896,#33897,
#33898,#33899,#33900,#33901,#33902),(#33903,#33904,#33905,#33906,#33907,
#33908,#33909,#33910,#33911,#33912,#33913,#33914),(#33915,#33916,#33917,
#33918,#33919,#33920,#33921,#33922,#33923,#33924,#33925,#33926),(#33927,
#33928,#33929,#33930,#33931,#33932,#33933,#33934,#33935,#33936,#33937,#33938)),
 .UNSPECIFIED.,.F.,.F.,.F.)
B_SPLINE_SURFACE_WITH_KNOTS((4,4),(4,2,2,2,2,4),(0.,1.),(0.,0.0783698388401235,
0.308777379129593,0.539184919419728,0.769592459709863,1.),.UNSPECIFIED.)
GEOMETRIC_REPRESENTATION_ITEM()
RATIONAL_B_SPLINE_SURFACE(((1.,1.,1.,1.,1.,1.,1.,1.,1.,1.,1.,1.),(0.833333333333332,
0.833333333333332,0.833333333333332,0.833333333333332,0.833333333333332,
0.833333333333332,0.833333333333332,0.833333333333332,0.833333333333332,
0.833333333333332,0.833333333333332,0.833333333333332),(0.833333333333332,
0.833333333333332,0.833333333333332,0.833333333333332,0.833333333333332,
0.833333333333332,0.833333333333332,0.833333333333332,0.833333333333332,
0.833333333333332,0.833333333333332,0.833333333333332),(1.,1.,1.,1.,1.,
1.,1.,1.,1.,1.,1.,1.)))
REPRESENTATION_ITEM('')
SURFACE()
);
#533=(
BOUNDED_SURFACE()
B_SPLINE_SURFACE(3,3,((#33955,#33956,#33957,#33958,#33959,#33960,#33961,
#33962,#33963,#33964,#33965,#33966),(#33967,#33968,#33969,#33970,#33971,
#33972,#33973,#33974,#33975,#33976,#33977,#33978),(#33979,#33980,#33981,
#33982,#33983,#33984,#33985,#33986,#33987,#33988,#33989,#33990),(#33991,
#33992,#33993,#33994,#33995,#33996,#33997,#33998,#33999,#34000,#34001,#34002)),
 .UNSPECIFIED.,.F.,.F.,.F.)
B_SPLINE_SURFACE_WITH_KNOTS((4,4),(4,2,2,2,2,4),(0.,1.),(0.,0.0783698388401235,
0.308777379129593,0.539184919419728,0.769592459709863,1.),.UNSPECIFIED.)
GEOMETRIC_REPRESENTATION_ITEM()
RATIONAL_B_SPLINE_SURFACE(((1.,1.,1.,1.,1.,1.,1.,1.,1.,1.,1.,1.),(0.987189825241073,
0.987189825241073,0.987189825241073,0.987189825241073,0.987189825241073,
0.987189825241073,0.987189825241073,0.987189825241073,0.987189825241073,
0.987189825241073,0.987189825241073,0.987189825241073),(0.987189825241073,
0.987189825241073,0.987189825241073,0.987189825241073,0.987189825241073,
0.987189825241073,0.987189825241073,0.987189825241073,0.987189825241073,
0.987189825241073,0.987189825241073,0.987189825241073),(1.,1.,1.,1.,1.,
1.,1.,1.,1.,1.,1.,1.)))
REPRESENTATION_ITEM('')
SURFACE()
);
#534=(
BOUNDED_SURFACE()
B_SPLINE_SURFACE(3,3,((#34003,#34004,#34005,#34006,#34007,#34008,#34009,
#34010,#34011,#34012,#34013,#34014),(#34015,#34016,#34017,#34018,#34019,
#34020,#34021,#34022,#34023,#34024,#34025,#34026),(#34027,#34028,#34029,
#34030,#34031,#34032,#34033,#34034,#34035,#34036,#34037,#34038),(#34039,
#34040,#34041,#34042,#34043,#34044,#34045,#34046,#34047,#34048,#34049,#34050)),
 .UNSPECIFIED.,.F.,.F.,.F.)
B_SPLINE_SURFACE_WITH_KNOTS((4,4),(4,2,2,2,2,4),(0.,1.),(0.,0.0783698388401235,
0.308777379129593,0.539184919419728,0.769592459709863,1.),.UNSPECIFIED.)
GEOMETRIC_REPRESENTATION_ITEM()
RATIONAL_B_SPLINE_SURFACE(((1.,1.,1.,1.,1.,1.,1.,1.,1.,1.,1.,1.),(0.987189825241073,
0.987189825241073,0.987189825241073,0.987189825241073,0.987189825241073,
0.987189825241073,0.987189825241073,0.987189825241073,0.987189825241073,
0.987189825241073,0.987189825241073,0.987189825241073),(0.987189825241073,
0.987189825241073,0.987189825241073,0.987189825241073,0.987189825241073,
0.987189825241073,0.987189825241073,0.987189825241073,0.987189825241073,
0.987189825241073,0.987189825241073,0.987189825241073),(1.,1.,1.,1.,1.,
1.,1.,1.,1.,1.,1.,1.)))
REPRESENTATION_ITEM('')
SURFACE()
);
#535=(
BOUNDED_SURFACE()
B_SPLINE_SURFACE(3,3,((#34051,#34052,#34053,#34054,#34055,#34056,#34057,
#34058,#34059,#34060,#34061,#34062,#34063,#34064),(#34065,#34066,#34067,
#34068,#34069,#34070,#34071,#34072,#34073,#34074,#34075,#34076,#34077,#34078),
(#34079,#34080,#34081,#34082,#34083,#34084,#34085,#34086,#34087,#34088,
#34089,#34090,#34091,#34092),(#34093,#34094,#34095,#34096,#34097,#34098,
#34099,#34100,#34101,#34102,#34103,#34104,#34105,#34106)),.UNSPECIFIED.,
 .F.,.F.,.F.)
B_SPLINE_SURFACE_WITH_KNOTS((4,4),(4,2,2,2,2,2,4),(0.,1.),(0.,0.0183879322611598,
0.0783698437311081,0.308777382797832,0.53918492186522,0.76959246093261,
1.),.UNSPECIFIED.)
GEOMETRIC_REPRESENTATION_ITEM()
RATIONAL_B_SPLINE_SURFACE(((1.,1.,1.,1.,1.,1.,1.,1.,1.,1.,1.,1.,1.,1.),
(0.833333333333332,0.833333333333332,0.833333333333332,0.833333333333332,
0.833333333333332,0.833333333333332,0.833333333333332,0.833333333333332,
0.833333333333332,0.833333333333332,0.833333333333332,0.833333333333332,
0.833333333333332,0.833333333333332),(0.833333333333332,0.833333333333332,
0.833333333333332,0.833333333333332,0.833333333333332,0.833333333333332,
0.833333333333332,0.833333333333332,0.833333333333332,0.833333333333332,
0.833333333333332,0.833333333333332,0.833333333333332,0.833333333333332),
(1.,1.,1.,1.,1.,1.,1.,1.,1.,1.,1.,1.,1.,1.)))
REPRESENTATION_ITEM('')
SURFACE()
);
#536=(
BOUNDED_SURFACE()
B_SPLINE_SURFACE(3,3,((#34125,#34126,#34127,#34128,#34129,#34130,#34131,
#34132,#34133,#34134,#34135,#34136,#34137,#34138),(#34139,#34140,#34141,
#34142,#34143,#34144,#34145,#34146,#34147,#34148,#34149,#34150,#34151,#34152),
(#34153,#34154,#34155,#34156,#34157,#34158,#34159,#34160,#34161,#34162,
#34163,#34164,#34165,#34166),(#34167,#34168,#34169,#34170,#34171,#34172,
#34173,#34174,#34175,#34176,#34177,#34178,#34179,#34180)),.UNSPECIFIED.,
 .F.,.F.,.F.)
B_SPLINE_SURFACE_WITH_KNOTS((4,4),(4,2,2,2,2,2,4),(0.,1.),(0.,0.0183879322611598,
0.0783698437311081,0.308777382797832,0.53918492186522,0.76959246093261,
1.),.UNSPECIFIED.)
GEOMETRIC_REPRESENTATION_ITEM()
RATIONAL_B_SPLINE_SURFACE(((1.,1.,1.,1.,1.,1.,1.,1.,1.,1.,1.,1.,1.,1.),
(0.987189825241073,0.987189825241073,0.987189825241073,0.987189825241073,
0.987189825241073,0.987189825241073,0.987189825241073,0.987189825241073,
0.987189825241073,0.987189825241073,0.987189825241073,0.987189825241073,
0.987189825241073,0.987189825241073),(0.987189825241073,0.987189825241073,
0.987189825241073,0.987189825241073,0.987189825241073,0.987189825241073,
0.987189825241073,0.987189825241073,0.987189825241073,0.987189825241073,
0.987189825241073,0.987189825241073,0.987189825241073,0.987189825241073),
(1.,1.,1.,1.,1.,1.,1.,1.,1.,1.,1.,1.,1.,1.)))
REPRESENTATION_ITEM('')
SURFACE()
);
#537=(
BOUNDED_SURFACE()
B_SPLINE_SURFACE(3,3,((#34181,#34182,#34183,#34184,#34185,#34186,#34187,
#34188,#34189,#34190,#34191,#34192,#34193,#34194),(#34195,#34196,#34197,
#34198,#34199,#34200,#34201,#34202,#34203,#34204,#34205,#34206,#34207,#34208),
(#34209,#34210,#34211,#34212,#34213,#34214,#34215,#34216,#34217,#34218,
#34219,#34220,#34221,#34222),(#34223,#34224,#34225,#34226,#34227,#34228,
#34229,#34230,#34231,#34232,#34233,#34234,#34235,#34236)),.UNSPECIFIED.,
 .F.,.F.,.F.)
B_SPLINE_SURFACE_WITH_KNOTS((4,4),(4,2,2,2,2,2,4),(0.,1.),(0.,0.0183879322611598,
0.0783698437311081,0.308777382797832,0.53918492186522,0.76959246093261,
1.),.UNSPECIFIED.)
GEOMETRIC_REPRESENTATION_ITEM()
RATIONAL_B_SPLINE_SURFACE(((1.,1.,1.,1.,1.,1.,1.,1.,1.,1.,1.,1.,1.,1.),
(0.987189825241073,0.987189825241073,0.987189825241073,0.987189825241073,
0.987189825241073,0.987189825241073,0.987189825241073,0.987189825241073,
0.987189825241073,0.987189825241073,0.987189825241073,0.987189825241073,
0.987189825241073,0.987189825241073),(0.987189825241073,0.987189825241073,
0.987189825241073,0.987189825241073,0.987189825241073,0.987189825241073,
0.987189825241073,0.987189825241073,0.987189825241073,0.987189825241073,
0.987189825241073,0.987189825241073,0.987189825241073,0.987189825241073),
(1.,1.,1.,1.,1.,1.,1.,1.,1.,1.,1.,1.,1.,1.)))
REPRESENTATION_ITEM('')
SURFACE()
);
#538=(
BOUNDED_SURFACE()
B_SPLINE_SURFACE(3,3,((#34237,#34238,#34239,#34240,#34241,#34242,#34243,
#34244,#34245,#34246,#34247,#34248,#34249,#34250),(#34251,#34252,#34253,
#34254,#34255,#34256,#34257,#34258,#34259,#34260,#34261,#34262,#34263,#34264),
(#34265,#34266,#34267,#34268,#34269,#34270,#34271,#34272,#34273,#34274,
#34275,#34276,#34277,#34278),(#34279,#34280,#34281,#34282,#34283,#34284,
#34285,#34286,#34287,#34288,#34289,#34290,#34291,#34292)),.UNSPECIFIED.,
 .F.,.F.,.F.)
B_SPLINE_SURFACE_WITH_KNOTS((4,4),(4,2,2,2,2,2,4),(0.,1.),(0.,0.0183879369801425,
0.078369848160917,0.308777386120188,0.539184924080124,0.769592462040062,
1.),.UNSPECIFIED.)
GEOMETRIC_REPRESENTATION_ITEM()
RATIONAL_B_SPLINE_SURFACE(((1.,1.,1.,1.,1.,1.,1.,1.,1.,1.,1.,1.,1.,1.),
(0.833333333333333,0.833333333333333,0.833333333333333,0.833333333333333,
0.833333333333333,0.833333333333333,0.833333333333333,0.833333333333333,
0.833333333333333,0.833333333333333,0.833333333333333,0.833333333333333,
0.833333333333333,0.833333333333333),(0.833333333333333,0.833333333333333,
0.833333333333333,0.833333333333333,0.833333333333333,0.833333333333333,
0.833333333333333,0.833333333333333,0.833333333333333,0.833333333333333,
0.833333333333333,0.833333333333333,0.833333333333333,0.833333333333333),
(1.,1.,1.,1.,1.,1.,1.,1.,1.,1.,1.,1.,1.,1.)))
REPRESENTATION_ITEM('')
SURFACE()
);
#539=(
BOUNDED_SURFACE()
B_SPLINE_SURFACE(3,3,((#34311,#34312,#34313,#34314,#34315,#34316,#34317,
#34318,#34319,#34320,#34321,#34322,#34323,#34324),(#34325,#34326,#34327,
#34328,#34329,#34330,#34331,#34332,#34333,#34334,#34335,#34336,#34337,#34338),
(#34339,#34340,#34341,#34342,#34343,#34344,#34345,#34346,#34347,#34348,
#34349,#34350,#34351,#34352),(#34353,#34354,#34355,#34356,#34357,#34358,
#34359,#34360,#34361,#34362,#34363,#34364,#34365,#34366)),.UNSPECIFIED.,
 .F.,.F.,.F.)
B_SPLINE_SURFACE_WITH_KNOTS((4,4),(4,2,2,2,2,2,4),(0.,1.),(0.,0.0183879369801425,
0.078369848160917,0.308777386120188,0.539184924080124,0.769592462040062,
1.),.UNSPECIFIED.)
GEOMETRIC_REPRESENTATION_ITEM()
RATIONAL_B_SPLINE_SURFACE(((1.,1.,1.,1.,1.,1.,1.,1.,1.,1.,1.,1.,1.,1.),
(0.987189825241073,0.987189825241073,0.987189825241073,0.987189825241073,
0.987189825241073,0.987189825241073,0.987189825241073,0.987189825241073,
0.987189825241073,0.987189825241073,0.987189825241073,0.987189825241073,
0.987189825241073,0.987189825241073),(0.987189825241073,0.987189825241073,
0.987189825241073,0.987189825241073,0.987189825241073,0.987189825241073,
0.987189825241073,0.987189825241073,0.987189825241073,0.987189825241073,
0.987189825241073,0.987189825241073,0.987189825241073,0.987189825241073),
(1.,1.,1.,1.,1.,1.,1.,1.,1.,1.,1.,1.,1.,1.)))
REPRESENTATION_ITEM('')
SURFACE()
);
#540=(
BOUNDED_SURFACE()
B_SPLINE_SURFACE(3,3,((#34367,#34368,#34369,#34370,#34371,#34372,#34373,
#34374,#34375,#34376,#34377,#34378,#34379,#34380),(#34381,#34382,#34383,
#34384,#34385,#34386,#34387,#34388,#34389,#34390,#34391,#34392,#34393,#34394),
(#34395,#34396,#34397,#34398,#34399,#34400,#34401,#34402,#34403,#34404,
#34405,#34406,#34407,#34408),(#34409,#34410,#34411,#34412,#34413,#34414,
#34415,#34416,#34417,#34418,#34419,#34420,#34421,#34422)),.UNSPECIFIED.,
 .F.,.F.,.F.)
B_SPLINE_SURFACE_WITH_KNOTS((4,4),(4,2,2,2,2,2,4),(0.,1.),(0.,0.0183879369801425,
0.078369848160917,0.308777386120188,0.539184924080124,0.769592462040062,
1.),.UNSPECIFIED.)
GEOMETRIC_REPRESENTATION_ITEM()
RATIONAL_B_SPLINE_SURFACE(((1.,1.,1.,1.,1.,1.,1.,1.,1.,1.,1.,1.,1.,1.),
(0.987189825241073,0.987189825241073,0.987189825241073,0.987189825241073,
0.987189825241073,0.987189825241073,0.987189825241073,0.987189825241073,
0.987189825241073,0.987189825241073,0.987189825241073,0.987189825241073,
0.987189825241073,0.987189825241073),(0.987189825241073,0.987189825241073,
0.987189825241073,0.987189825241073,0.987189825241073,0.987189825241073,
0.987189825241073,0.987189825241073,0.987189825241073,0.987189825241073,
0.987189825241073,0.987189825241073,0.987189825241073,0.987189825241073),
(1.,1.,1.,1.,1.,1.,1.,1.,1.,1.,1.,1.,1.,1.)))
REPRESENTATION_ITEM('')
SURFACE()
);
#541=(
BOUNDED_SURFACE()
B_SPLINE_SURFACE(3,3,((#34423,#34424,#34425,#34426,#34427,#34428,#34429,
#34430,#34431,#34432,#34433,#34434),(#34435,#34436,#34437,#34438,#34439,
#34440,#34441,#34442,#34443,#34444,#34445,#34446),(#34447,#34448,#34449,
#34450,#34451,#34452,#34453,#34454,#34455,#34456,#34457,#34458),(#34459,
#34460,#34461,#34462,#34463,#34464,#34465,#34466,#34467,#34468,#34469,#34470)),
 .UNSPECIFIED.,.F.,.F.,.F.)
B_SPLINE_SURFACE_WITH_KNOTS((4,4),(4,2,2,2,2,4),(0.,1.),(0.,0.0783698504850856,
0.308777387863315,0.539184925242209,0.769592462621105,1.),.UNSPECIFIED.)
GEOMETRIC_REPRESENTATION_ITEM()
RATIONAL_B_SPLINE_SURFACE(((1.,1.,1.,1.,1.,1.,1.,1.,1.,1.,1.,1.),(0.833333333333333,
0.833333333333333,0.833333333333333,0.833333333333333,0.833333333333333,
0.833333333333333,0.833333333333333,0.833333333333333,0.833333333333333,
0.833333333333333,0.833333333333333,0.833333333333333),(0.833333333333333,
0.833333333333333,0.833333333333333,0.833333333333333,0.833333333333333,
0.833333333333333,0.833333333333333,0.833333333333333,0.833333333333333,
0.833333333333333,0.833333333333333,0.833333333333333),(1.,1.,1.,1.,1.,
1.,1.,1.,1.,1.,1.,1.)))
REPRESENTATION_ITEM('')
SURFACE()
);
#542=(
BOUNDED_SURFACE()
B_SPLINE_SURFACE(3,3,((#34487,#34488,#34489,#34490,#34491,#34492,#34493,
#34494,#34495,#34496,#34497,#34498),(#34499,#34500,#34501,#34502,#34503,
#34504,#34505,#34506,#34507,#34508,#34509,#34510),(#34511,#34512,#34513,
#34514,#34515,#34516,#34517,#34518,#34519,#34520,#34521,#34522),(#34523,
#34524,#34525,#34526,#34527,#34528,#34529,#34530,#34531,#34532,#34533,#34534)),
 .UNSPECIFIED.,.F.,.F.,.F.)
B_SPLINE_SURFACE_WITH_KNOTS((4,4),(4,2,2,2,2,4),(0.,1.),(0.,0.0783698504850856,
0.308777387863315,0.539184925242209,0.769592462621105,1.),.UNSPECIFIED.)
GEOMETRIC_REPRESENTATION_ITEM()
RATIONAL_B_SPLINE_SURFACE(((1.,1.,1.,1.,1.,1.,1.,1.,1.,1.,1.,1.),(0.987189825241073,
0.987189825241073,0.987189825241073,0.987189825241073,0.987189825241073,
0.987189825241073,0.987189825241073,0.987189825241073,0.987189825241073,
0.987189825241073,0.987189825241073,0.987189825241073),(0.987189825241073,
0.987189825241073,0.987189825241073,0.987189825241073,0.987189825241073,
0.987189825241073,0.987189825241073,0.987189825241073,0.987189825241073,
0.987189825241073,0.987189825241073,0.987189825241073),(1.,1.,1.,1.,1.,
1.,1.,1.,1.,1.,1.,1.)))
REPRESENTATION_ITEM('')
SURFACE()
);
#543=(
BOUNDED_SURFACE()
B_SPLINE_SURFACE(3,3,((#34535,#34536,#34537,#34538,#34539,#34540,#34541,
#34542,#34543,#34544,#34545,#34546),(#34547,#34548,#34549,#34550,#34551,
#34552,#34553,#34554,#34555,#34556,#34557,#34558),(#34559,#34560,#34561,
#34562,#34563,#34564,#34565,#34566,#34567,#34568,#34569,#34570),(#34571,
#34572,#34573,#34574,#34575,#34576,#34577,#34578,#34579,#34580,#34581,#34582)),
 .UNSPECIFIED.,.F.,.F.,.F.)
B_SPLINE_SURFACE_WITH_KNOTS((4,4),(4,2,2,2,2,4),(0.,1.),(0.,0.0783698504850856,
0.308777387863315,0.539184925242209,0.769592462621105,1.),.UNSPECIFIED.)
GEOMETRIC_REPRESENTATION_ITEM()
RATIONAL_B_SPLINE_SURFACE(((1.,1.,1.,1.,1.,1.,1.,1.,1.,1.,1.,1.),(0.987189825241073,
0.987189825241073,0.987189825241073,0.987189825241073,0.987189825241073,
0.987189825241073,0.987189825241073,0.987189825241073,0.987189825241073,
0.987189825241073,0.987189825241073,0.987189825241073),(0.987189825241073,
0.987189825241073,0.987189825241073,0.987189825241073,0.987189825241073,
0.987189825241073,0.987189825241073,0.987189825241073,0.987189825241073,
0.987189825241073,0.987189825241073,0.987189825241073),(1.,1.,1.,1.,1.,
1.,1.,1.,1.,1.,1.,1.)))
REPRESENTATION_ITEM('')
SURFACE()
);
#544=(
BOUNDED_SURFACE()
B_SPLINE_SURFACE(3,3,((#34583,#34584,#34585,#34586,#34587,#34588,#34589,
#34590,#34591,#34592,#34593,#34594),(#34595,#34596,#34597,#34598,#34599,
#34600,#34601,#34602,#34603,#34604,#34605,#34606),(#34607,#34608,#34609,
#34610,#34611,#34612,#34613,#34614,#34615,#34616,#34617,#34618),(#34619,
#34620,#34621,#34622,#34623,#34624,#34625,#34626,#34627,#34628,#34629,#34630)),
 .UNSPECIFIED.,.F.,.F.,.F.)
B_SPLINE_SURFACE_WITH_KNOTS((4,4),(4,2,2,2,2,4),(0.,1.),(0.,0.0783698504851055,
0.30877738786333,0.539184925242219,0.769592462621109,1.),.UNSPECIFIED.)
GEOMETRIC_REPRESENTATION_ITEM()
RATIONAL_B_SPLINE_SURFACE(((1.,1.,1.,1.,1.,1.,1.,1.,1.,1.,1.,1.),(0.833333333333332,
0.833333333333332,0.833333333333332,0.833333333333332,0.833333333333332,
0.833333333333332,0.833333333333332,0.833333333333332,0.833333333333332,
0.833333333333332,0.833333333333332,0.833333333333332),(0.833333333333332,
0.833333333333332,0.833333333333332,0.833333333333332,0.833333333333332,
0.833333333333332,0.833333333333332,0.833333333333332,0.833333333333332,
0.833333333333332,0.833333333333332,0.833333333333332),(1.,1.,1.,1.,1.,
1.,1.,1.,1.,1.,1.,1.)))
REPRESENTATION_ITEM('')
SURFACE()
);
#545=(
BOUNDED_SURFACE()
B_SPLINE_SURFACE(3,3,((#34647,#34648,#34649,#34650,#34651,#34652,#34653,
#34654,#34655,#34656,#34657,#34658),(#34659,#34660,#34661,#34662,#34663,
#34664,#34665,#34666,#34667,#34668,#34669,#34670),(#34671,#34672,#34673,
#34674,#34675,#34676,#34677,#34678,#34679,#34680,#34681,#34682),(#34683,
#34684,#34685,#34686,#34687,#34688,#34689,#34690,#34691,#34692,#34693,#34694)),
 .UNSPECIFIED.,.F.,.F.,.F.)
B_SPLINE_SURFACE_WITH_KNOTS((4,4),(4,2,2,2,2,4),(0.,1.),(0.,0.0783698504851055,
0.30877738786333,0.539184925242219,0.769592462621109,1.),.UNSPECIFIED.)
GEOMETRIC_REPRESENTATION_ITEM()
RATIONAL_B_SPLINE_SURFACE(((1.,1.,1.,1.,1.,1.,1.,1.,1.,1.,1.,1.),(0.987189825241073,
0.987189825241073,0.987189825241073,0.987189825241073,0.987189825241073,
0.987189825241073,0.987189825241073,0.987189825241073,0.987189825241073,
0.987189825241073,0.987189825241073,0.987189825241073),(0.987189825241073,
0.987189825241073,0.987189825241073,0.987189825241073,0.987189825241073,
0.987189825241073,0.987189825241073,0.987189825241073,0.987189825241073,
0.987189825241073,0.987189825241073,0.987189825241073),(1.,1.,1.,1.,1.,
1.,1.,1.,1.,1.,1.,1.)))
REPRESENTATION_ITEM('')
SURFACE()
);
#546=(
BOUNDED_SURFACE()
B_SPLINE_SURFACE(3,3,((#34695,#34696,#34697,#34698,#34699,#34700,#34701,
#34702,#34703,#34704,#34705,#34706),(#34707,#34708,#34709,#34710,#34711,
#34712,#34713,#34714,#34715,#34716,#34717,#34718),(#34719,#34720,#34721,
#34722,#34723,#34724,#34725,#34726,#34727,#34728,#34729,#34730),(#34731,
#34732,#34733,#34734,#34735,#34736,#34737,#34738,#34739,#34740,#34741,#34742)),
 .UNSPECIFIED.,.F.,.F.,.F.)
B_SPLINE_SURFACE_WITH_KNOTS((4,4),(4,2,2,2,2,4),(0.,1.),(0.,0.0783698504851055,
0.30877738786333,0.539184925242219,0.769592462621109,1.),.UNSPECIFIED.)
GEOMETRIC_REPRESENTATION_ITEM()
RATIONAL_B_SPLINE_SURFACE(((1.,1.,1.,1.,1.,1.,1.,1.,1.,1.,1.,1.),(0.987189825241073,
0.987189825241073,0.987189825241073,0.987189825241073,0.987189825241073,
0.987189825241073,0.987189825241073,0.987189825241073,0.987189825241073,
0.987189825241073,0.987189825241073,0.987189825241073),(0.987189825241073,
0.987189825241073,0.987189825241073,0.987189825241073,0.987189825241073,
0.987189825241073,0.987189825241073,0.987189825241073,0.987189825241073,
0.987189825241073,0.987189825241073,0.987189825241073),(1.,1.,1.,1.,1.,
1.,1.,1.,1.,1.,1.,1.)))
REPRESENTATION_ITEM('')
SURFACE()
);
#547=(
BOUNDED_SURFACE()
B_SPLINE_SURFACE(3,3,((#34743,#34744,#34745,#34746,#34747,#34748,#34749,
#34750,#34751,#34752,#34753,#34754),(#34755,#34756,#34757,#34758,#34759,
#34760,#34761,#34762,#34763,#34764,#34765,#34766),(#34767,#34768,#34769,
#34770,#34771,#34772,#34773,#34774,#34775,#34776,#34777,#34778),(#34779,
#34780,#34781,#34782,#34783,#34784,#34785,#34786,#34787,#34788,#34789,#34790)),
 .UNSPECIFIED.,.F.,.F.,.F.)
B_SPLINE_SURFACE_WITH_KNOTS((4,4),(4,2,2,2,2,4),(0.,1.),(0.,0.0783698481609002,
0.308777386120176,0.539184924080116,0.769592462040058,1.),.UNSPECIFIED.)
GEOMETRIC_REPRESENTATION_ITEM()
RATIONAL_B_SPLINE_SURFACE(((1.,1.,1.,1.,1.,1.,1.,1.,1.,1.,1.,1.),(0.833333333333333,
0.833333333333333,0.833333333333333,0.833333333333333,0.833333333333333,
0.833333333333333,0.833333333333333,0.833333333333333,0.833333333333333,
0.833333333333333,0.833333333333333,0.833333333333333),(0.833333333333333,
0.833333333333333,0.833333333333333,0.833333333333333,0.833333333333333,
0.833333333333333,0.833333333333333,0.833333333333333,0.833333333333333,
0.833333333333333,0.833333333333333,0.833333333333333),(1.,1.,1.,1.,1.,
1.,1.,1.,1.,1.,1.,1.)))
REPRESENTATION_ITEM('')
SURFACE()
);
#548=(
BOUNDED_SURFACE()
B_SPLINE_SURFACE(3,3,((#34807,#34808,#34809,#34810,#34811,#34812,#34813,
#34814,#34815,#34816,#34817,#34818),(#34819,#34820,#34821,#34822,#34823,
#34824,#34825,#34826,#34827,#34828,#34829,#34830),(#34831,#34832,#34833,
#34834,#34835,#34836,#34837,#34838,#34839,#34840,#34841,#34842),(#34843,
#34844,#34845,#34846,#34847,#34848,#34849,#34850,#34851,#34852,#34853,#34854)),
 .UNSPECIFIED.,.F.,.F.,.F.)
B_SPLINE_SURFACE_WITH_KNOTS((4,4),(4,2,2,2,2,4),(0.,1.),(0.,0.0783698481609002,
0.308777386120176,0.539184924080116,0.769592462040058,1.),.UNSPECIFIED.)
GEOMETRIC_REPRESENTATION_ITEM()
RATIONAL_B_SPLINE_SURFACE(((1.,1.,1.,1.,1.,1.,1.,1.,1.,1.,1.,1.),(0.987189825241073,
0.987189825241073,0.987189825241073,0.987189825241073,0.987189825241073,
0.987189825241073,0.987189825241073,0.987189825241073,0.987189825241073,
0.987189825241073,0.987189825241073,0.987189825241073),(0.987189825241073,
0.987189825241073,0.987189825241073,0.987189825241073,0.987189825241073,
0.987189825241073,0.987189825241073,0.987189825241073,0.987189825241073,
0.987189825241073,0.987189825241073,0.987189825241073),(1.,1.,1.,1.,1.,
1.,1.,1.,1.,1.,1.,1.)))
REPRESENTATION_ITEM('')
SURFACE()
);
#549=(
BOUNDED_SURFACE()
B_SPLINE_SURFACE(3,3,((#34855,#34856,#34857,#34858,#34859,#34860,#34861,
#34862,#34863,#34864,#34865,#34866),(#34867,#34868,#34869,#34870,#34871,
#34872,#34873,#34874,#34875,#34876,#34877,#34878),(#34879,#34880,#34881,
#34882,#34883,#34884,#34885,#34886,#34887,#34888,#34889,#34890),(#34891,
#34892,#34893,#34894,#34895,#34896,#34897,#34898,#34899,#34900,#34901,#34902)),
 .UNSPECIFIED.,.F.,.F.,.F.)
B_SPLINE_SURFACE_WITH_KNOTS((4,4),(4,2,2,2,2,4),(0.,1.),(0.,0.0783698481609002,
0.308777386120176,0.539184924080116,0.769592462040058,1.),.UNSPECIFIED.)
GEOMETRIC_REPRESENTATION_ITEM()
RATIONAL_B_SPLINE_SURFACE(((1.,1.,1.,1.,1.,1.,1.,1.,1.,1.,1.,1.),(0.987189825241073,
0.987189825241073,0.987189825241073,0.987189825241073,0.987189825241073,
0.987189825241073,0.987189825241073,0.987189825241073,0.987189825241073,
0.987189825241073,0.987189825241073,0.987189825241073),(0.987189825241073,
0.987189825241073,0.987189825241073,0.987189825241073,0.987189825241073,
0.987189825241073,0.987189825241073,0.987189825241073,0.987189825241073,
0.987189825241073,0.987189825241073,0.987189825241073),(1.,1.,1.,1.,1.,
1.,1.,1.,1.,1.,1.,1.)))
REPRESENTATION_ITEM('')
SURFACE()
);
#550=(
BOUNDED_SURFACE()
B_SPLINE_SURFACE(3,3,((#34903,#34904,#34905,#34906,#34907,#34908,#34909,
#34910,#34911,#34912,#34913,#34914),(#34915,#34916,#34917,#34918,#34919,
#34920,#34921,#34922,#34923,#34924,#34925,#34926),(#34927,#34928,#34929,
#34930,#34931,#34932,#34933,#34934,#34935,#34936,#34937,#34938),(#34939,
#34940,#34941,#34942,#34943,#34944,#34945,#34946,#34947,#34948,#34949,#34950)),
 .UNSPECIFIED.,.F.,.F.,.F.)
B_SPLINE_SURFACE_WITH_KNOTS((4,4),(4,2,2,2,2,4),(0.,1.),(0.,0.0783698437310988,
0.308777382797825,0.539184921865215,0.769592460932608,1.),.UNSPECIFIED.)
GEOMETRIC_REPRESENTATION_ITEM()
RATIONAL_B_SPLINE_SURFACE(((1.,1.,1.,1.,1.,1.,1.,1.,1.,1.,1.,1.),(0.833333333333332,
0.833333333333332,0.833333333333332,0.833333333333332,0.833333333333332,
0.833333333333332,0.833333333333332,0.833333333333332,0.833333333333332,
0.833333333333332,0.833333333333332,0.833333333333332),(0.833333333333332,
0.833333333333332,0.833333333333332,0.833333333333332,0.833333333333332,
0.833333333333332,0.833333333333332,0.833333333333332,0.833333333333332,
0.833333333333332,0.833333333333332,0.833333333333332),(1.,1.,1.,1.,1.,
1.,1.,1.,1.,1.,1.,1.)))
REPRESENTATION_ITEM('')
SURFACE()
);
#551=(
BOUNDED_SURFACE()
B_SPLINE_SURFACE(3,3,((#34967,#34968,#34969,#34970,#34971,#34972,#34973,
#34974,#34975,#34976,#34977,#34978),(#34979,#34980,#34981,#34982,#34983,
#34984,#34985,#34986,#34987,#34988,#34989,#34990),(#34991,#34992,#34993,
#34994,#34995,#34996,#34997,#34998,#34999,#35000,#35001,#35002),(#35003,
#35004,#35005,#35006,#35007,#35008,#35009,#35010,#35011,#35012,#35013,#35014)),
 .UNSPECIFIED.,.F.,.F.,.F.)
B_SPLINE_SURFACE_WITH_KNOTS((4,4),(4,2,2,2,2,4),(0.,1.),(0.,0.0783698437310988,
0.308777382797825,0.539184921865215,0.769592460932608,1.),.UNSPECIFIED.)
GEOMETRIC_REPRESENTATION_ITEM()
RATIONAL_B_SPLINE_SURFACE(((1.,1.,1.,1.,1.,1.,1.,1.,1.,1.,1.,1.),(0.987189825241073,
0.987189825241073,0.987189825241073,0.987189825241073,0.987189825241073,
0.987189825241073,0.987189825241073,0.987189825241073,0.987189825241073,
0.987189825241073,0.987189825241073,0.987189825241073),(0.987189825241073,
0.987189825241073,0.987189825241073,0.987189825241073,0.987189825241073,
0.987189825241073,0.987189825241073,0.987189825241073,0.987189825241073,
0.987189825241073,0.987189825241073,0.987189825241073),(1.,1.,1.,1.,1.,
1.,1.,1.,1.,1.,1.,1.)))
REPRESENTATION_ITEM('')
SURFACE()
);
#552=(
BOUNDED_SURFACE()
B_SPLINE_SURFACE(3,3,((#35015,#35016,#35017,#35018,#35019,#35020,#35021,
#35022,#35023,#35024,#35025,#35026),(#35027,#35028,#35029,#35030,#35031,
#35032,#35033,#35034,#35035,#35036,#35037,#35038),(#35039,#35040,#35041,
#35042,#35043,#35044,#35045,#35046,#35047,#35048,#35049,#35050),(#35051,
#35052,#35053,#35054,#35055,#35056,#35057,#35058,#35059,#35060,#35061,#35062)),
 .UNSPECIFIED.,.F.,.F.,.F.)
B_SPLINE_SURFACE_WITH_KNOTS((4,4),(4,2,2,2,2,4),(0.,1.),(0.,0.0783698437310988,
0.308777382797825,0.539184921865215,0.769592460932608,1.),.UNSPECIFIED.)
GEOMETRIC_REPRESENTATION_ITEM()
RATIONAL_B_SPLINE_SURFACE(((1.,1.,1.,1.,1.,1.,1.,1.,1.,1.,1.,1.),(0.987189825241073,
0.987189825241073,0.987189825241073,0.987189825241073,0.987189825241073,
0.987189825241073,0.987189825241073,0.987189825241073,0.987189825241073,
0.987189825241073,0.987189825241073,0.987189825241073),(0.987189825241073,
0.987189825241073,0.987189825241073,0.987189825241073,0.987189825241073,
0.987189825241073,0.987189825241073,0.987189825241073,0.987189825241073,
0.987189825241073,0.987189825241073,0.987189825241073),(1.,1.,1.,1.,1.,
1.,1.,1.,1.,1.,1.,1.)))
REPRESENTATION_ITEM('')
SURFACE()
);
#553=(
BOUNDED_SURFACE()
B_SPLINE_SURFACE(3,3,((#35063,#35064,#35065,#35066,#35067,#35068,#35069,
#35070,#35071,#35072,#35073,#35074),(#35075,#35076,#35077,#35078,#35079,
#35080,#35081,#35082,#35083,#35084,#35085,#35086),(#35087,#35088,#35089,
#35090,#35091,#35092,#35093,#35094,#35095,#35096,#35097,#35098),(#35099,
#35100,#35101,#35102,#35103,#35104,#35105,#35106,#35107,#35108,#35109,#35110)),
 .UNSPECIFIED.,.F.,.F.,.F.)
B_SPLINE_SURFACE_WITH_KNOTS((4,4),(4,2,2,2,2,4),(0.,1.),(0.,0.078369838840116,
0.308777379129587,0.539184919419724,0.769592459709862,1.),.UNSPECIFIED.)
GEOMETRIC_REPRESENTATION_ITEM()
RATIONAL_B_SPLINE_SURFACE(((1.,1.,1.,1.,1.,1.,1.,1.,1.,1.,1.,1.),(0.833333333333333,
0.833333333333333,0.833333333333333,0.833333333333333,0.833333333333333,
0.833333333333333,0.833333333333333,0.833333333333333,0.833333333333333,
0.833333333333333,0.833333333333333,0.833333333333333),(0.833333333333333,
0.833333333333333,0.833333333333333,0.833333333333333,0.833333333333333,
0.833333333333333,0.833333333333333,0.833333333333333,0.833333333333333,
0.833333333333333,0.833333333333333,0.833333333333333),(1.,1.,1.,1.,1.,
1.,1.,1.,1.,1.,1.,1.)))
REPRESENTATION_ITEM('')
SURFACE()
);
#554=(
BOUNDED_SURFACE()
B_SPLINE_SURFACE(3,3,((#35127,#35128,#35129,#35130,#35131,#35132,#35133,
#35134,#35135,#35136,#35137,#35138),(#35139,#35140,#35141,#35142,#35143,
#35144,#35145,#35146,#35147,#35148,#35149,#35150),(#35151,#35152,#35153,
#35154,#35155,#35156,#35157,#35158,#35159,#35160,#35161,#35162),(#35163,
#35164,#35165,#35166,#35167,#35168,#35169,#35170,#35171,#35172,#35173,#35174)),
 .UNSPECIFIED.,.F.,.F.,.F.)
B_SPLINE_SURFACE_WITH_KNOTS((4,4),(4,2,2,2,2,4),(0.,1.),(0.,0.078369838840116,
0.308777379129587,0.539184919419724,0.769592459709862,1.),.UNSPECIFIED.)
GEOMETRIC_REPRESENTATION_ITEM()
RATIONAL_B_SPLINE_SURFACE(((1.,1.,1.,1.,1.,1.,1.,1.,1.,1.,1.,1.),(0.987189825241073,
0.987189825241073,0.987189825241073,0.987189825241073,0.987189825241073,
0.987189825241073,0.987189825241073,0.987189825241073,0.987189825241073,
0.987189825241073,0.987189825241073,0.987189825241073),(0.987189825241073,
0.987189825241073,0.987189825241073,0.987189825241073,0.987189825241073,
0.987189825241073,0.987189825241073,0.987189825241073,0.987189825241073,
0.987189825241073,0.987189825241073,0.987189825241073),(1.,1.,1.,1.,1.,
1.,1.,1.,1.,1.,1.,1.)))
REPRESENTATION_ITEM('')
SURFACE()
);
#555=(
BOUNDED_SURFACE()
B_SPLINE_SURFACE(3,3,((#35175,#35176,#35177,#35178,#35179,#35180,#35181,
#35182,#35183,#35184,#35185,#35186),(#35187,#35188,#35189,#35190,#35191,
#35192,#35193,#35194,#35195,#35196,#35197,#35198),(#35199,#35200,#35201,
#35202,#35203,#35204,#35205,#35206,#35207,#35208,#35209,#35210),(#35211,
#35212,#35213,#35214,#35215,#35216,#35217,#35218,#35219,#35220,#35221,#35222)),
 .UNSPECIFIED.,.F.,.F.,.F.)
B_SPLINE_SURFACE_WITH_KNOTS((4,4),(4,2,2,2,2,4),(0.,1.),(0.,0.078369838840116,
0.308777379129587,0.539184919419724,0.769592459709862,1.),.UNSPECIFIED.)
GEOMETRIC_REPRESENTATION_ITEM()
RATIONAL_B_SPLINE_SURFACE(((1.,1.,1.,1.,1.,1.,1.,1.,1.,1.,1.,1.),(0.987189825241073,
0.987189825241073,0.987189825241073,0.987189825241073,0.987189825241073,
0.987189825241073,0.987189825241073,0.987189825241073,0.987189825241073,
0.987189825241073,0.987189825241073,0.987189825241073),(0.987189825241073,
0.987189825241073,0.987189825241073,0.987189825241073,0.987189825241073,
0.987189825241073,0.987189825241073,0.987189825241073,0.987189825241073,
0.987189825241073,0.987189825241073,0.987189825241073),(1.,1.,1.,1.,1.,
1.,1.,1.,1.,1.,1.,1.)))
REPRESENTATION_ITEM('')
SURFACE()
);
#556=(
BOUNDED_SURFACE()
B_SPLINE_SURFACE(3,3,((#35223,#35224,#35225,#35226,#35227,#35228,#35229,
#35230,#35231,#35232,#35233,#35234),(#35235,#35236,#35237,#35238,#35239,
#35240,#35241,#35242,#35243,#35244,#35245,#35246),(#35247,#35248,#35249,
#35250,#35251,#35252,#35253,#35254,#35255,#35256,#35257,#35258),(#35259,
#35260,#35261,#35262,#35263,#35264,#35265,#35266,#35267,#35268,#35269,#35270)),
 .UNSPECIFIED.,.F.,.F.,.F.)
B_SPLINE_SURFACE_WITH_KNOTS((4,4),(4,2,2,2,2,4),(0.,1.),(0.,0.0783698352504284,
0.308777376437322,0.53918491762488,0.76959245881244,1.),.UNSPECIFIED.)
GEOMETRIC_REPRESENTATION_ITEM()
RATIONAL_B_SPLINE_SURFACE(((1.,1.,1.,1.,1.,1.,1.,1.,1.,1.,1.,1.),(0.833333333333332,
0.833333333333332,0.833333333333332,0.833333333333332,0.833333333333332,
0.833333333333332,0.833333333333332,0.833333333333332,0.833333333333332,
0.833333333333332,0.833333333333332,0.833333333333332),(0.833333333333332,
0.833333333333332,0.833333333333332,0.833333333333332,0.833333333333332,
0.833333333333332,0.833333333333332,0.833333333333332,0.833333333333332,
0.833333333333332,0.833333333333332,0.833333333333332),(1.,1.,1.,1.,1.,
1.,1.,1.,1.,1.,1.,1.)))
REPRESENTATION_ITEM('')
SURFACE()
);
#557=(
BOUNDED_SURFACE()
B_SPLINE_SURFACE(3,3,((#35287,#35288,#35289,#35290,#35291,#35292,#35293,
#35294,#35295,#35296,#35297,#35298),(#35299,#35300,#35301,#35302,#35303,
#35304,#35305,#35306,#35307,#35308,#35309,#35310),(#35311,#35312,#35313,
#35314,#35315,#35316,#35317,#35318,#35319,#35320,#35321,#35322),(#35323,
#35324,#35325,#35326,#35327,#35328,#35329,#35330,#35331,#35332,#35333,#35334)),
 .UNSPECIFIED.,.F.,.F.,.F.)
B_SPLINE_SURFACE_WITH_KNOTS((4,4),(4,2,2,2,2,4),(0.,1.),(0.,0.0783698352504284,
0.308777376437322,0.53918491762488,0.76959245881244,1.),.UNSPECIFIED.)
GEOMETRIC_REPRESENTATION_ITEM()
RATIONAL_B_SPLINE_SURFACE(((1.,1.,1.,1.,1.,1.,1.,1.,1.,1.,1.,1.),(0.987189825241073,
0.987189825241073,0.987189825241073,0.987189825241073,0.987189825241073,
0.987189825241073,0.987189825241073,0.987189825241073,0.987189825241073,
0.987189825241073,0.987189825241073,0.987189825241073),(0.987189825241073,
0.987189825241073,0.987189825241073,0.987189825241073,0.987189825241073,
0.987189825241073,0.987189825241073,0.987189825241073,0.987189825241073,
0.987189825241073,0.987189825241073,0.987189825241073),(1.,1.,1.,1.,1.,
1.,1.,1.,1.,1.,1.,1.)))
REPRESENTATION_ITEM('')
SURFACE()
);
#558=(
BOUNDED_SURFACE()
B_SPLINE_SURFACE(3,3,((#35335,#35336,#35337,#35338,#35339,#35340,#35341,
#35342,#35343,#35344,#35345,#35346),(#35347,#35348,#35349,#35350,#35351,
#35352,#35353,#35354,#35355,#35356,#35357,#35358),(#35359,#35360,#35361,
#35362,#35363,#35364,#35365,#35366,#35367,#35368,#35369,#35370),(#35371,
#35372,#35373,#35374,#35375,#35376,#35377,#35378,#35379,#35380,#35381,#35382)),
 .UNSPECIFIED.,.F.,.F.,.F.)
B_SPLINE_SURFACE_WITH_KNOTS((4,4),(4,2,2,2,2,4),(0.,1.),(0.,0.0783698352504284,
0.308777376437322,0.53918491762488,0.76959245881244,1.),.UNSPECIFIED.)
GEOMETRIC_REPRESENTATION_ITEM()
RATIONAL_B_SPLINE_SURFACE(((1.,1.,1.,1.,1.,1.,1.,1.,1.,1.,1.,1.),(0.987189825241073,
0.987189825241073,0.987189825241073,0.987189825241073,0.987189825241073,
0.987189825241073,0.987189825241073,0.987189825241073,0.987189825241073,
0.987189825241073,0.987189825241073,0.987189825241073),(0.987189825241073,
0.987189825241073,0.987189825241073,0.987189825241073,0.987189825241073,
0.987189825241073,0.987189825241073,0.987189825241073,0.987189825241073,
0.987189825241073,0.987189825241073,0.987189825241073),(1.,1.,1.,1.,1.,
1.,1.,1.,1.,1.,1.,1.)))
REPRESENTATION_ITEM('')
SURFACE()
);
#559=(
BOUNDED_SURFACE()
B_SPLINE_SURFACE(3,3,((#35383,#35384,#35385,#35386,#35387,#35388,#35389,
#35390,#35391,#35392,#35393,#35394,#35395,#35396),(#35397,#35398,#35399,
#35400,#35401,#35402,#35403,#35404,#35405,#35406,#35407,#35408,#35409,#35410),
(#35411,#35412,#35413,#35414,#35415,#35416,#35417,#35418,#35419,#35420,
#35421,#35422,#35423,#35424),(#35425,#35426,#35427,#35428,#35429,#35430,
#35431,#35432,#35433,#35434,#35435,#35436,#35437,#35438)),.UNSPECIFIED.,
 .F.,.F.,.F.)
B_SPLINE_SURFACE_WITH_KNOTS((4,4),(4,2,2,2,2,2,4),(0.,1.),(0.,0.0183879168994272,
0.0783698293107271,0.308777371982546,0.53918491465503,0.769592457327514,
1.),.UNSPECIFIED.)
GEOMETRIC_REPRESENTATION_ITEM()
RATIONAL_B_SPLINE_SURFACE(((1.,1.,1.,1.,1.,1.,1.,1.,1.,1.,1.,1.,1.,1.),
(0.833333333333332,0.833333333333332,0.833333333333332,0.833333333333332,
0.833333333333332,0.833333333333332,0.833333333333332,0.833333333333332,
0.833333333333332,0.833333333333332,0.833333333333332,0.833333333333332,
0.833333333333332,0.833333333333332),(0.833333333333332,0.833333333333332,
0.833333333333332,0.833333333333332,0.833333333333332,0.833333333333332,
0.833333333333332,0.833333333333332,0.833333333333332,0.833333333333332,
0.833333333333332,0.833333333333332,0.833333333333332,0.833333333333332),
(1.,1.,1.,1.,1.,1.,1.,1.,1.,1.,1.,1.,1.,1.)))
REPRESENTATION_ITEM('')
SURFACE()
);
#560=(
BOUNDED_SURFACE()
B_SPLINE_SURFACE(3,3,((#35457,#35458,#35459,#35460,#35461,#35462,#35463,
#35464,#35465,#35466,#35467,#35468,#35469,#35470),(#35471,#35472,#35473,
#35474,#35475,#35476,#35477,#35478,#35479,#35480,#35481,#35482,#35483,#35484),
(#35485,#35486,#35487,#35488,#35489,#35490,#35491,#35492,#35493,#35494,
#35495,#35496,#35497,#35498),(#35499,#35500,#35501,#35502,#35503,#35504,
#35505,#35506,#35507,#35508,#35509,#35510,#35511,#35512)),.UNSPECIFIED.,
 .F.,.F.,.F.)
B_SPLINE_SURFACE_WITH_KNOTS((4,4),(4,2,2,2,2,2,4),(0.,1.),(0.,0.0183879168994272,
0.0783698293107271,0.308777371982546,0.53918491465503,0.769592457327514,
1.),.UNSPECIFIED.)
GEOMETRIC_REPRESENTATION_ITEM()
RATIONAL_B_SPLINE_SURFACE(((1.,1.,1.,1.,1.,1.,1.,1.,1.,1.,1.,1.,1.,1.),
(0.987189825241073,0.987189825241073,0.987189825241073,0.987189825241073,
0.987189825241073,0.987189825241073,0.987189825241073,0.987189825241073,
0.987189825241073,0.987189825241073,0.987189825241073,0.987189825241073,
0.987189825241073,0.987189825241073),(0.987189825241073,0.987189825241073,
0.987189825241073,0.987189825241073,0.987189825241073,0.987189825241073,
0.987189825241073,0.987189825241073,0.987189825241073,0.987189825241073,
0.987189825241073,0.987189825241073,0.987189825241073,0.987189825241073),
(1.,1.,1.,1.,1.,1.,1.,1.,1.,1.,1.,1.,1.,1.)))
REPRESENTATION_ITEM('')
SURFACE()
);
#561=(
BOUNDED_SURFACE()
B_SPLINE_SURFACE(3,3,((#35513,#35514,#35515,#35516,#35517,#35518,#35519,
#35520,#35521,#35522,#35523,#35524,#35525,#35526),(#35527,#35528,#35529,
#35530,#35531,#35532,#35533,#35534,#35535,#35536,#35537,#35538,#35539,#35540),
(#35541,#35542,#35543,#35544,#35545,#35546,#35547,#35548,#35549,#35550,
#35551,#35552,#35553,#35554),(#35555,#35556,#35557,#35558,#35559,#35560,
#35561,#35562,#35563,#35564,#35565,#35566,#35567,#35568)),.UNSPECIFIED.,
 .F.,.F.,.F.)
B_SPLINE_SURFACE_WITH_KNOTS((4,4),(4,2,2,2,2,2,4),(0.,1.),(0.,0.0183879168994272,
0.0783698293107271,0.308777371982546,0.53918491465503,0.769592457327514,
1.),.UNSPECIFIED.)
GEOMETRIC_REPRESENTATION_ITEM()
RATIONAL_B_SPLINE_SURFACE(((1.,1.,1.,1.,1.,1.,1.,1.,1.,1.,1.,1.,1.,1.),
(0.987189825241073,0.987189825241073,0.987189825241073,0.987189825241073,
0.987189825241073,0.987189825241073,0.987189825241073,0.987189825241073,
0.987189825241073,0.987189825241073,0.987189825241073,0.987189825241073,
0.987189825241073,0.987189825241073),(0.987189825241073,0.987189825241073,
0.987189825241073,0.987189825241073,0.987189825241073,0.987189825241073,
0.987189825241073,0.987189825241073,0.987189825241073,0.987189825241073,
0.987189825241073,0.987189825241073,0.987189825241073,0.987189825241073),
(1.,1.,1.,1.,1.,1.,1.,1.,1.,1.,1.,1.,1.,1.)))
REPRESENTATION_ITEM('')
SURFACE()
);
#562=(
BOUNDED_SURFACE()
B_SPLINE_SURFACE(3,3,((#35569,#35570,#35571,#35572,#35573,#35574,#35575,
#35576,#35577,#35578,#35579,#35580,#35581,#35582),(#35583,#35584,#35585,
#35586,#35587,#35588,#35589,#35590,#35591,#35592,#35593,#35594,#35595,#35596),
(#35597,#35598,#35599,#35600,#35601,#35602,#35603,#35604,#35605,#35606,
#35607,#35608,#35609,#35610),(#35611,#35612,#35613,#35614,#35615,#35616,
#35617,#35618,#35619,#35620,#35621,#35622,#35623,#35624)),.UNSPECIFIED.,
 .F.,.F.,.F.)
B_SPLINE_SURFACE_WITH_KNOTS((4,4),(4,2,2,2,2,2,4),(0.,1.),(0.,0.0183879232268624,
0.0783698352504226,0.308777376437317,0.539184917624878,0.769592458812438,
1.),.UNSPECIFIED.)
GEOMETRIC_REPRESENTATION_ITEM()
RATIONAL_B_SPLINE_SURFACE(((1.,1.,1.,1.,1.,1.,1.,1.,1.,1.,1.,1.,1.,1.),
(0.833333333333333,0.833333333333333,0.833333333333333,0.833333333333333,
0.833333333333333,0.833333333333333,0.833333333333333,0.833333333333333,
0.833333333333333,0.833333333333333,0.833333333333333,0.833333333333333,
0.833333333333333,0.833333333333333),(0.833333333333333,0.833333333333333,
0.833333333333333,0.833333333333333,0.833333333333333,0.833333333333333,
0.833333333333333,0.833333333333333,0.833333333333333,0.833333333333333,
0.833333333333333,0.833333333333333,0.833333333333333,0.833333333333333),
(1.,1.,1.,1.,1.,1.,1.,1.,1.,1.,1.,1.,1.,1.)))
REPRESENTATION_ITEM('')
SURFACE()
);
#563=(
BOUNDED_SURFACE()
B_SPLINE_SURFACE(3,3,((#35643,#35644,#35645,#35646,#35647,#35648,#35649,
#35650,#35651,#35652,#35653,#35654,#35655,#35656),(#35657,#35658,#35659,
#35660,#35661,#35662,#35663,#35664,#35665,#35666,#35667,#35668,#35669,#35670),
(#35671,#35672,#35673,#35674,#35675,#35676,#35677,#35678,#35679,#35680,
#35681,#35682,#35683,#35684),(#35685,#35686,#35687,#35688,#35689,#35690,
#35691,#35692,#35693,#35694,#35695,#35696,#35697,#35698)),.UNSPECIFIED.,
 .F.,.F.,.F.)
B_SPLINE_SURFACE_WITH_KNOTS((4,4),(4,2,2,2,2,2,4),(0.,1.),(0.,0.0183879232268624,
0.0783698352504226,0.308777376437317,0.539184917624878,0.769592458812438,
1.),.UNSPECIFIED.)
GEOMETRIC_REPRESENTATION_ITEM()
RATIONAL_B_SPLINE_SURFACE(((1.,1.,1.,1.,1.,1.,1.,1.,1.,1.,1.,1.,1.,1.),
(0.987189825241073,0.987189825241073,0.987189825241073,0.987189825241073,
0.987189825241073,0.987189825241073,0.987189825241073,0.987189825241073,
0.987189825241073,0.987189825241073,0.987189825241073,0.987189825241073,
0.987189825241073,0.987189825241073),(0.987189825241073,0.987189825241073,
0.987189825241073,0.987189825241073,0.987189825241073,0.987189825241073,
0.987189825241073,0.987189825241073,0.987189825241073,0.987189825241073,
0.987189825241073,0.987189825241073,0.987189825241073,0.987189825241073),
(1.,1.,1.,1.,1.,1.,1.,1.,1.,1.,1.,1.,1.,1.)))
REPRESENTATION_ITEM('')
SURFACE()
);
#564=(
BOUNDED_SURFACE()
B_SPLINE_SURFACE(3,3,((#35699,#35700,#35701,#35702,#35703,#35704,#35705,
#35706,#35707,#35708,#35709,#35710,#35711,#35712),(#35713,#35714,#35715,
#35716,#35717,#35718,#35719,#35720,#35721,#35722,#35723,#35724,#35725,#35726),
(#35727,#35728,#35729,#35730,#35731,#35732,#35733,#35734,#35735,#35736,
#35737,#35738,#35739,#35740),(#35741,#35742,#35743,#35744,#35745,#35746,
#35747,#35748,#35749,#35750,#35751,#35752,#35753,#35754)),.UNSPECIFIED.,
 .F.,.F.,.F.)
B_SPLINE_SURFACE_WITH_KNOTS((4,4),(4,2,2,2,2,2,4),(0.,1.),(0.,0.0183879232268624,
0.0783698352504226,0.308777376437317,0.539184917624878,0.769592458812438,
1.),.UNSPECIFIED.)
GEOMETRIC_REPRESENTATION_ITEM()
RATIONAL_B_SPLINE_SURFACE(((1.,1.,1.,1.,1.,1.,1.,1.,1.,1.,1.,1.,1.,1.),
(0.987189825241073,0.987189825241073,0.987189825241073,0.987189825241073,
0.987189825241073,0.987189825241073,0.987189825241073,0.987189825241073,
0.987189825241073,0.987189825241073,0.987189825241073,0.987189825241073,
0.987189825241073,0.987189825241073),(0.987189825241073,0.987189825241073,
0.987189825241073,0.987189825241073,0.987189825241073,0.987189825241073,
0.987189825241073,0.987189825241073,0.987189825241073,0.987189825241073,
0.987189825241073,0.987189825241073,0.987189825241073,0.987189825241073),
(1.,1.,1.,1.,1.,1.,1.,1.,1.,1.,1.,1.,1.,1.)))
REPRESENTATION_ITEM('')
SURFACE()
);
#565=(
BOUNDED_SURFACE()
B_SPLINE_SURFACE(3,3,((#35755,#35756,#35757,#35758,#35759,#35760,#35761,
#35762,#35763,#35764,#35765,#35766),(#35767,#35768,#35769,#35770,#35771,
#35772,#35773,#35774,#35775,#35776,#35777,#35778),(#35779,#35780,#35781,
#35782,#35783,#35784,#35785,#35786,#35787,#35788,#35789,#35790),(#35791,
#35792,#35793,#35794,#35795,#35796,#35797,#35798,#35799,#35800,#35801,#35802)),
 .UNSPECIFIED.,.F.,.F.,.F.)
B_SPLINE_SURFACE_WITH_KNOTS((4,4),(4,2,2,2,2,4),(0.,1.),(0.,0.078369838840114,
0.308777379129586,0.539184919419723,0.769592459709861,1.),.UNSPECIFIED.)
GEOMETRIC_REPRESENTATION_ITEM()
RATIONAL_B_SPLINE_SURFACE(((1.,1.,1.,1.,1.,1.,1.,1.,1.,1.,1.,1.),(0.833333333333332,
0.833333333333332,0.833333333333332,0.833333333333332,0.833333333333332,
0.833333333333332,0.833333333333332,0.833333333333332,0.833333333333332,
0.833333333333332,0.833333333333332,0.833333333333332),(0.833333333333332,
0.833333333333332,0.833333333333332,0.833333333333332,0.833333333333332,
0.833333333333332,0.833333333333332,0.833333333333332,0.833333333333332,
0.833333333333332,0.833333333333332,0.833333333333332),(1.,1.,1.,1.,1.,
1.,1.,1.,1.,1.,1.,1.)))
REPRESENTATION_ITEM('')
SURFACE()
);
#566=(
BOUNDED_SURFACE()
B_SPLINE_SURFACE(3,3,((#35819,#35820,#35821,#35822,#35823,#35824,#35825,
#35826,#35827,#35828,#35829,#35830),(#35831,#35832,#35833,#35834,#35835,
#35836,#35837,#35838,#35839,#35840,#35841,#35842),(#35843,#35844,#35845,
#35846,#35847,#35848,#35849,#35850,#35851,#35852,#35853,#35854),(#35855,
#35856,#35857,#35858,#35859,#35860,#35861,#35862,#35863,#35864,#35865,#35866)),
 .UNSPECIFIED.,.F.,.F.,.F.)
B_SPLINE_SURFACE_WITH_KNOTS((4,4),(4,2,2,2,2,4),(0.,1.),(0.,0.078369838840114,
0.308777379129586,0.539184919419723,0.769592459709861,1.),.UNSPECIFIED.)
GEOMETRIC_REPRESENTATION_ITEM()
RATIONAL_B_SPLINE_SURFACE(((1.,1.,1.,1.,1.,1.,1.,1.,1.,1.,1.,1.),(0.987189825241073,
0.987189825241073,0.987189825241073,0.987189825241073,0.987189825241073,
0.987189825241073,0.987189825241073,0.987189825241073,0.987189825241073,
0.987189825241073,0.987189825241073,0.987189825241073),(0.987189825241073,
0.987189825241073,0.987189825241073,0.987189825241073,0.987189825241073,
0.987189825241073,0.987189825241073,0.987189825241073,0.987189825241073,
0.987189825241073,0.987189825241073,0.987189825241073),(1.,1.,1.,1.,1.,
1.,1.,1.,1.,1.,1.,1.)))
REPRESENTATION_ITEM('')
SURFACE()
);
#567=(
BOUNDED_SURFACE()
B_SPLINE_SURFACE(3,3,((#35867,#35868,#35869,#35870,#35871,#35872,#35873,
#35874,#35875,#35876,#35877,#35878),(#35879,#35880,#35881,#35882,#35883,
#35884,#35885,#35886,#35887,#35888,#35889,#35890),(#35891,#35892,#35893,
#35894,#35895,#35896,#35897,#35898,#35899,#35900,#35901,#35902),(#35903,
#35904,#35905,#35906,#35907,#35908,#35909,#35910,#35911,#35912,#35913,#35914)),
 .UNSPECIFIED.,.F.,.F.,.F.)
B_SPLINE_SURFACE_WITH_KNOTS((4,4),(4,2,2,2,2,4),(0.,1.),(0.,0.078369838840114,
0.308777379129586,0.539184919419723,0.769592459709861,1.),.UNSPECIFIED.)
GEOMETRIC_REPRESENTATION_ITEM()
RATIONAL_B_SPLINE_SURFACE(((1.,1.,1.,1.,1.,1.,1.,1.,1.,1.,1.,1.),(0.987189825241073,
0.987189825241073,0.987189825241073,0.987189825241073,0.987189825241073,
0.987189825241073,0.987189825241073,0.987189825241073,0.987189825241073,
0.987189825241073,0.987189825241073,0.987189825241073),(0.987189825241073,
0.987189825241073,0.987189825241073,0.987189825241073,0.987189825241073,
0.987189825241073,0.987189825241073,0.987189825241073,0.987189825241073,
0.987189825241073,0.987189825241073,0.987189825241073),(1.,1.,1.,1.,1.,
1.,1.,1.,1.,1.,1.,1.)))
REPRESENTATION_ITEM('')
SURFACE()
);
#568=(
BOUNDED_SURFACE()
B_SPLINE_SURFACE(3,3,((#35915,#35916,#35917,#35918,#35919,#35920,#35921,
#35922,#35923,#35924,#35925,#35926),(#35927,#35928,#35929,#35930,#35931,
#35932,#35933,#35934,#35935,#35936,#35937,#35938),(#35939,#35940,#35941,
#35942,#35943,#35944,#35945,#35946,#35947,#35948,#35949,#35950),(#35951,
#35952,#35953,#35954,#35955,#35956,#35957,#35958,#35959,#35960,#35961,#35962)),
 .UNSPECIFIED.,.F.,.F.,.F.)
B_SPLINE_SURFACE_WITH_KNOTS((4,4),(4,2,2,2,2,4),(0.,1.),(0.,0.078369843731106,
0.30877738279783,0.539184921865219,0.769592460932609,1.),.UNSPECIFIED.)
GEOMETRIC_REPRESENTATION_ITEM()
RATIONAL_B_SPLINE_SURFACE(((1.,1.,1.,1.,1.,1.,1.,1.,1.,1.,1.,1.),(0.833333333333331,
0.833333333333331,0.833333333333331,0.833333333333331,0.833333333333331,
0.833333333333331,0.833333333333331,0.833333333333331,0.833333333333331,
0.833333333333331,0.833333333333331,0.833333333333331),(0.833333333333331,
0.833333333333331,0.833333333333331,0.833333333333331,0.833333333333331,
0.833333333333331,0.833333333333331,0.833333333333331,0.833333333333331,
0.833333333333331,0.833333333333331,0.833333333333331),(1.,1.,1.,1.,1.,
1.,1.,1.,1.,1.,1.,1.)))
REPRESENTATION_ITEM('')
SURFACE()
);
#569=(
BOUNDED_SURFACE()
B_SPLINE_SURFACE(3,3,((#35979,#35980,#35981,#35982,#35983,#35984,#35985,
#35986,#35987,#35988,#35989,#35990),(#35991,#35992,#35993,#35994,#35995,
#35996,#35997,#35998,#35999,#36000,#36001,#36002),(#36003,#36004,#36005,
#36006,#36007,#36008,#36009,#36010,#36011,#36012,#36013,#36014),(#36015,
#36016,#36017,#36018,#36019,#36020,#36021,#36022,#36023,#36024,#36025,#36026)),
 .UNSPECIFIED.,.F.,.F.,.F.)
B_SPLINE_SURFACE_WITH_KNOTS((4,4),(4,2,2,2,2,4),(0.,1.),(0.,0.078369843731106,
0.30877738279783,0.539184921865219,0.769592460932609,1.),.UNSPECIFIED.)
GEOMETRIC_REPRESENTATION_ITEM()
RATIONAL_B_SPLINE_SURFACE(((1.,1.,1.,1.,1.,1.,1.,1.,1.,1.,1.,1.),(0.987189825241073,
0.987189825241073,0.987189825241073,0.987189825241073,0.987189825241073,
0.987189825241073,0.987189825241073,0.987189825241073,0.987189825241073,
0.987189825241073,0.987189825241073,0.987189825241073),(0.987189825241073,
0.987189825241073,0.987189825241073,0.987189825241073,0.987189825241073,
0.987189825241073,0.987189825241073,0.987189825241073,0.987189825241073,
0.987189825241073,0.987189825241073,0.987189825241073),(1.,1.,1.,1.,1.,
1.,1.,1.,1.,1.,1.,1.)))
REPRESENTATION_ITEM('')
SURFACE()
);
#570=(
BOUNDED_SURFACE()
B_SPLINE_SURFACE(3,3,((#36027,#36028,#36029,#36030,#36031,#36032,#36033,
#36034,#36035,#36036,#36037,#36038),(#36039,#36040,#36041,#36042,#36043,
#36044,#36045,#36046,#36047,#36048,#36049,#36050),(#36051,#36052,#36053,
#36054,#36055,#36056,#36057,#36058,#36059,#36060,#36061,#36062),(#36063,
#36064,#36065,#36066,#36067,#36068,#36069,#36070,#36071,#36072,#36073,#36074)),
 .UNSPECIFIED.,.F.,.F.,.F.)
B_SPLINE_SURFACE_WITH_KNOTS((4,4),(4,2,2,2,2,4),(0.,1.),(0.,0.078369843731106,
0.30877738279783,0.539184921865219,0.769592460932609,1.),.UNSPECIFIED.)
GEOMETRIC_REPRESENTATION_ITEM()
RATIONAL_B_SPLINE_SURFACE(((1.,1.,1.,1.,1.,1.,1.,1.,1.,1.,1.,1.),(0.987189825241073,
0.987189825241073,0.987189825241073,0.987189825241073,0.987189825241073,
0.987189825241073,0.987189825241073,0.987189825241073,0.987189825241073,
0.987189825241073,0.987189825241073,0.987189825241073),(0.987189825241073,
0.987189825241073,0.987189825241073,0.987189825241073,0.987189825241073,
0.987189825241073,0.987189825241073,0.987189825241073,0.987189825241073,
0.987189825241073,0.987189825241073,0.987189825241073),(1.,1.,1.,1.,1.,
1.,1.,1.,1.,1.,1.,1.)))
REPRESENTATION_ITEM('')
SURFACE()
);
#571=(
BOUNDED_SURFACE()
B_SPLINE_SURFACE(3,3,((#36075,#36076,#36077,#36078,#36079,#36080,#36081,
#36082,#36083,#36084,#36085,#36086),(#36087,#36088,#36089,#36090,#36091,
#36092,#36093,#36094,#36095,#36096,#36097,#36098),(#36099,#36100,#36101,
#36102,#36103,#36104,#36105,#36106,#36107,#36108,#36109,#36110),(#36111,
#36112,#36113,#36114,#36115,#36116,#36117,#36118,#36119,#36120,#36121,#36122)),
 .UNSPECIFIED.,.F.,.F.,.F.)
B_SPLINE_SURFACE_WITH_KNOTS((4,4),(4,2,2,2,2,4),(0.,1.),(0.,0.0783698481609171,
0.308777386120188,0.539184924080125,0.769592462040062,1.),.UNSPECIFIED.)
GEOMETRIC_REPRESENTATION_ITEM()
RATIONAL_B_SPLINE_SURFACE(((1.,1.,1.,1.,1.,1.,1.,1.,1.,1.,1.,1.),(0.987189825241073,
0.987189825241073,0.987189825241073,0.987189825241073,0.987189825241073,
0.987189825241073,0.987189825241073,0.987189825241073,0.987189825241073,
0.987189825241073,0.987189825241073,0.987189825241073),(0.987189825241073,
0.987189825241073,0.987189825241073,0.987189825241073,0.987189825241073,
0.987189825241073,0.987189825241073,0.987189825241073,0.987189825241073,
0.987189825241073,0.987189825241073,0.987189825241073),(1.,1.,1.,1.,1.,
1.,1.,1.,1.,1.,1.,1.)))
REPRESENTATION_ITEM('')
SURFACE()
);
#572=(
BOUNDED_SURFACE()
B_SPLINE_SURFACE(3,3,((#36131,#36132,#36133,#36134,#36135,#36136,#36137,
#36138,#36139,#36140,#36141,#36142),(#36143,#36144,#36145,#36146,#36147,
#36148,#36149,#36150,#36151,#36152,#36153,#36154),(#36155,#36156,#36157,
#36158,#36159,#36160,#36161,#36162,#36163,#36164,#36165,#36166),(#36167,
#36168,#36169,#36170,#36171,#36172,#36173,#36174,#36175,#36176,#36177,#36178)),
 .UNSPECIFIED.,.F.,.F.,.F.)
B_SPLINE_SURFACE_WITH_KNOTS((4,4),(4,2,2,2,2,4),(0.,1.),(0.,0.0783698481609171,
0.308777386120188,0.539184924080125,0.769592462040062,1.),.UNSPECIFIED.)
GEOMETRIC_REPRESENTATION_ITEM()
RATIONAL_B_SPLINE_SURFACE(((1.,1.,1.,1.,1.,1.,1.,1.,1.,1.,1.,1.),(0.987189825241073,
0.987189825241073,0.987189825241073,0.987189825241073,0.987189825241073,
0.987189825241073,0.987189825241073,0.987189825241073,0.987189825241073,
0.987189825241073,0.987189825241073,0.987189825241073),(0.987189825241073,
0.987189825241073,0.987189825241073,0.987189825241073,0.987189825241073,
0.987189825241073,0.987189825241073,0.987189825241073,0.987189825241073,
0.987189825241073,0.987189825241073,0.987189825241073),(1.,1.,1.,1.,1.,
1.,1.,1.,1.,1.,1.,1.)))
REPRESENTATION_ITEM('')
SURFACE()
);
#573=(
BOUNDED_SURFACE()
B_SPLINE_SURFACE(3,3,((#36187,#36188,#36189,#36190,#36191,#36192,#36193,
#36194,#36195,#36196,#36197,#36198),(#36199,#36200,#36201,#36202,#36203,
#36204,#36205,#36206,#36207,#36208,#36209,#36210),(#36211,#36212,#36213,
#36214,#36215,#36216,#36217,#36218,#36219,#36220,#36221,#36222),(#36223,
#36224,#36225,#36226,#36227,#36228,#36229,#36230,#36231,#36232,#36233,#36234)),
 .UNSPECIFIED.,.F.,.F.,.F.)
B_SPLINE_SURFACE_WITH_KNOTS((4,4),(4,2,2,2,2,4),(0.,1.),(0.,0.0783698481609171,
0.308777386120188,0.539184924080125,0.769592462040062,1.),.UNSPECIFIED.)
GEOMETRIC_REPRESENTATION_ITEM()
RATIONAL_B_SPLINE_SURFACE(((1.,1.,1.,1.,1.,1.,1.,1.,1.,1.,1.,1.),(0.833333333333332,
0.833333333333332,0.833333333333332,0.833333333333332,0.833333333333332,
0.833333333333332,0.833333333333332,0.833333333333332,0.833333333333332,
0.833333333333332,0.833333333333332,0.833333333333332),(0.833333333333332,
0.833333333333332,0.833333333333332,0.833333333333332,0.833333333333332,
0.833333333333332,0.833333333333332,0.833333333333332,0.833333333333332,
0.833333333333332,0.833333333333332,0.833333333333332),(1.,1.,1.,1.,1.,
1.,1.,1.,1.,1.,1.,1.)))
REPRESENTATION_ITEM('')
SURFACE()
);
#574=(
BOUNDED_SURFACE()
B_SPLINE_SURFACE(3,3,((#36235,#36236,#36237,#36238,#36239,#36240,#36241,
#36242,#36243,#36244,#36245,#36246),(#36247,#36248,#36249,#36250,#36251,
#36252,#36253,#36254,#36255,#36256,#36257,#36258),(#36259,#36260,#36261,
#36262,#36263,#36264,#36265,#36266,#36267,#36268,#36269,#36270),(#36271,
#36272,#36273,#36274,#36275,#36276,#36277,#36278,#36279,#36280,#36281,#36282)),
 .UNSPECIFIED.,.F.,.F.,.F.)
B_SPLINE_SURFACE_WITH_KNOTS((4,4),(4,2,2,2,2,4),(0.,1.),(0.,0.0783698504850854,
0.308777387863314,0.539184925242208,0.769592462621104,1.),.UNSPECIFIED.)
GEOMETRIC_REPRESENTATION_ITEM()
RATIONAL_B_SPLINE_SURFACE(((1.,1.,1.,1.,1.,1.,1.,1.,1.,1.,1.,1.),(0.833333333333333,
0.833333333333333,0.833333333333333,0.833333333333333,0.833333333333333,
0.833333333333333,0.833333333333333,0.833333333333333,0.833333333333333,
0.833333333333333,0.833333333333333,0.833333333333333),(0.833333333333333,
0.833333333333333,0.833333333333333,0.833333333333333,0.833333333333333,
0.833333333333333,0.833333333333333,0.833333333333333,0.833333333333333,
0.833333333333333,0.833333333333333,0.833333333333333),(1.,1.,1.,1.,1.,
1.,1.,1.,1.,1.,1.,1.)))
REPRESENTATION_ITEM('')
SURFACE()
);
#575=(
BOUNDED_SURFACE()
B_SPLINE_SURFACE(3,3,((#36299,#36300,#36301,#36302,#36303,#36304,#36305,
#36306,#36307,#36308,#36309,#36310),(#36311,#36312,#36313,#36314,#36315,
#36316,#36317,#36318,#36319,#36320,#36321,#36322),(#36323,#36324,#36325,
#36326,#36327,#36328,#36329,#36330,#36331,#36332,#36333,#36334),(#36335,
#36336,#36337,#36338,#36339,#36340,#36341,#36342,#36343,#36344,#36345,#36346)),
 .UNSPECIFIED.,.F.,.F.,.F.)
B_SPLINE_SURFACE_WITH_KNOTS((4,4),(4,2,2,2,2,4),(0.,1.),(0.,0.0783698504850854,
0.308777387863314,0.539184925242208,0.769592462621104,1.),.UNSPECIFIED.)
GEOMETRIC_REPRESENTATION_ITEM()
RATIONAL_B_SPLINE_SURFACE(((1.,1.,1.,1.,1.,1.,1.,1.,1.,1.,1.,1.),(0.987189825241073,
0.987189825241073,0.987189825241073,0.987189825241073,0.987189825241073,
0.987189825241073,0.987189825241073,0.987189825241073,0.987189825241073,
0.987189825241073,0.987189825241073,0.987189825241073),(0.987189825241073,
0.987189825241073,0.987189825241073,0.987189825241073,0.987189825241073,
0.987189825241073,0.987189825241073,0.987189825241073,0.987189825241073,
0.987189825241073,0.987189825241073,0.987189825241073),(1.,1.,1.,1.,1.,
1.,1.,1.,1.,1.,1.,1.)))
REPRESENTATION_ITEM('')
SURFACE()
);
#576=(
BOUNDED_SURFACE()
B_SPLINE_SURFACE(3,3,((#36347,#36348,#36349,#36350,#36351,#36352,#36353,
#36354,#36355,#36356,#36357,#36358),(#36359,#36360,#36361,#36362,#36363,
#36364,#36365,#36366,#36367,#36368,#36369,#36370),(#36371,#36372,#36373,
#36374,#36375,#36376,#36377,#36378,#36379,#36380,#36381,#36382),(#36383,
#36384,#36385,#36386,#36387,#36388,#36389,#36390,#36391,#36392,#36393,#36394)),
 .UNSPECIFIED.,.F.,.F.,.F.)
B_SPLINE_SURFACE_WITH_KNOTS((4,4),(4,2,2,2,2,4),(0.,1.),(0.,0.0783698504850854,
0.308777387863314,0.539184925242208,0.769592462621104,1.),.UNSPECIFIED.)
GEOMETRIC_REPRESENTATION_ITEM()
RATIONAL_B_SPLINE_SURFACE(((1.,1.,1.,1.,1.,1.,1.,1.,1.,1.,1.,1.),(0.987189825241073,
0.987189825241073,0.987189825241073,0.987189825241073,0.987189825241073,
0.987189825241073,0.987189825241073,0.987189825241073,0.987189825241073,
0.987189825241073,0.987189825241073,0.987189825241073),(0.987189825241073,
0.987189825241073,0.987189825241073,0.987189825241073,0.987189825241073,
0.987189825241073,0.987189825241073,0.987189825241073,0.987189825241073,
0.987189825241073,0.987189825241073,0.987189825241073),(1.,1.,1.,1.,1.,
1.,1.,1.,1.,1.,1.,1.)))
REPRESENTATION_ITEM('')
SURFACE()
);
#577=(
BOUNDED_SURFACE()
B_SPLINE_SURFACE(3,3,((#36395,#36396,#36397,#36398,#36399,#36400,#36401,
#36402,#36403,#36404,#36405,#36406),(#36407,#36408,#36409,#36410,#36411,
#36412,#36413,#36414,#36415,#36416,#36417,#36418),(#36419,#36420,#36421,
#36422,#36423,#36424,#36425,#36426,#36427,#36428,#36429,#36430),(#36431,
#36432,#36433,#36434,#36435,#36436,#36437,#36438,#36439,#36440,#36441,#36442)),
 .UNSPECIFIED.,.F.,.F.,.F.)
B_SPLINE_SURFACE_WITH_KNOTS((4,4),(4,2,2,2,2,4),(0.,1.),(0.,0.0783698504851048,
0.308777387863329,0.539184925242218,0.769592462621109,1.),.UNSPECIFIED.)
GEOMETRIC_REPRESENTATION_ITEM()
RATIONAL_B_SPLINE_SURFACE(((1.,1.,1.,1.,1.,1.,1.,1.,1.,1.,1.,1.),(0.833333333333332,
0.833333333333332,0.833333333333332,0.833333333333332,0.833333333333332,
0.833333333333332,0.833333333333332,0.833333333333332,0.833333333333332,
0.833333333333332,0.833333333333332,0.833333333333332),(0.833333333333332,
0.833333333333332,0.833333333333332,0.833333333333332,0.833333333333332,
0.833333333333332,0.833333333333332,0.833333333333332,0.833333333333332,
0.833333333333332,0.833333333333332,0.833333333333332),(1.,1.,1.,1.,1.,
1.,1.,1.,1.,1.,1.,1.)))
REPRESENTATION_ITEM('')
SURFACE()
);
#578=(
BOUNDED_SURFACE()
B_SPLINE_SURFACE(3,3,((#36459,#36460,#36461,#36462,#36463,#36464,#36465,
#36466,#36467,#36468,#36469,#36470),(#36471,#36472,#36473,#36474,#36475,
#36476,#36477,#36478,#36479,#36480,#36481,#36482),(#36483,#36484,#36485,
#36486,#36487,#36488,#36489,#36490,#36491,#36492,#36493,#36494),(#36495,
#36496,#36497,#36498,#36499,#36500,#36501,#36502,#36503,#36504,#36505,#36506)),
 .UNSPECIFIED.,.F.,.F.,.F.)
B_SPLINE_SURFACE_WITH_KNOTS((4,4),(4,2,2,2,2,4),(0.,1.),(0.,0.0783698504851048,
0.308777387863329,0.539184925242218,0.769592462621109,1.),.UNSPECIFIED.)
GEOMETRIC_REPRESENTATION_ITEM()
RATIONAL_B_SPLINE_SURFACE(((1.,1.,1.,1.,1.,1.,1.,1.,1.,1.,1.,1.),(0.987189825241073,
0.987189825241073,0.987189825241073,0.987189825241073,0.987189825241073,
0.987189825241073,0.987189825241073,0.987189825241073,0.987189825241073,
0.987189825241073,0.987189825241073,0.987189825241073),(0.987189825241073,
0.987189825241073,0.987189825241073,0.987189825241073,0.987189825241073,
0.987189825241073,0.987189825241073,0.987189825241073,0.987189825241073,
0.987189825241073,0.987189825241073,0.987189825241073),(1.,1.,1.,1.,1.,
1.,1.,1.,1.,1.,1.,1.)))
REPRESENTATION_ITEM('')
SURFACE()
);
#579=(
BOUNDED_SURFACE()
B_SPLINE_SURFACE(3,3,((#36507,#36508,#36509,#36510,#36511,#36512,#36513,
#36514,#36515,#36516,#36517,#36518),(#36519,#36520,#36521,#36522,#36523,
#36524,#36525,#36526,#36527,#36528,#36529,#36530),(#36531,#36532,#36533,
#36534,#36535,#36536,#36537,#36538,#36539,#36540,#36541,#36542),(#36543,
#36544,#36545,#36546,#36547,#36548,#36549,#36550,#36551,#36552,#36553,#36554)),
 .UNSPECIFIED.,.F.,.F.,.F.)
B_SPLINE_SURFACE_WITH_KNOTS((4,4),(4,2,2,2,2,4),(0.,1.),(0.,0.0783698504851048,
0.308777387863329,0.539184925242218,0.769592462621109,1.),.UNSPECIFIED.)
GEOMETRIC_REPRESENTATION_ITEM()
RATIONAL_B_SPLINE_SURFACE(((1.,1.,1.,1.,1.,1.,1.,1.,1.,1.,1.,1.),(0.987189825241073,
0.987189825241073,0.987189825241073,0.987189825241073,0.987189825241073,
0.987189825241073,0.987189825241073,0.987189825241073,0.987189825241073,
0.987189825241073,0.987189825241073,0.987189825241073),(0.987189825241073,
0.987189825241073,0.987189825241073,0.987189825241073,0.987189825241073,
0.987189825241073,0.987189825241073,0.987189825241073,0.987189825241073,
0.987189825241073,0.987189825241073,0.987189825241073),(1.,1.,1.,1.,1.,
1.,1.,1.,1.,1.,1.,1.)))
REPRESENTATION_ITEM('')
SURFACE()
);
#580=(
BOUNDED_SURFACE()
B_SPLINE_SURFACE(3,3,((#36555,#36556,#36557,#36558,#36559,#36560,#36561,
#36562,#36563,#36564,#36565,#36566),(#36567,#36568,#36569,#36570,#36571,
#36572,#36573,#36574,#36575,#36576,#36577,#36578),(#36579,#36580,#36581,
#36582,#36583,#36584,#36585,#36586,#36587,#36588,#36589,#36590),(#36591,
#36592,#36593,#36594,#36595,#36596,#36597,#36598,#36599,#36600,#36601,#36602)),
 .UNSPECIFIED.,.F.,.F.,.F.)
B_SPLINE_SURFACE_WITH_KNOTS((4,4),(4,2,2,2,2,4),(0.,1.),(0.,0.0783698481609187,
0.30877738612019,0.539184924080125,0.769592462040063,1.),.UNSPECIFIED.)
GEOMETRIC_REPRESENTATION_ITEM()
RATIONAL_B_SPLINE_SURFACE(((1.,1.,1.,1.,1.,1.,1.,1.,1.,1.,1.,1.),(0.833333333333332,
0.833333333333332,0.833333333333332,0.833333333333332,0.833333333333332,
0.833333333333332,0.833333333333332,0.833333333333332,0.833333333333332,
0.833333333333332,0.833333333333332,0.833333333333332),(0.833333333333332,
0.833333333333332,0.833333333333332,0.833333333333332,0.833333333333332,
0.833333333333332,0.833333333333332,0.833333333333332,0.833333333333332,
0.833333333333332,0.833333333333332,0.833333333333332),(1.,1.,1.,1.,1.,
1.,1.,1.,1.,1.,1.,1.)))
REPRESENTATION_ITEM('')
SURFACE()
);
#581=(
BOUNDED_SURFACE()
B_SPLINE_SURFACE(3,3,((#36619,#36620,#36621,#36622,#36623,#36624,#36625,
#36626,#36627,#36628,#36629,#36630),(#36631,#36632,#36633,#36634,#36635,
#36636,#36637,#36638,#36639,#36640,#36641,#36642),(#36643,#36644,#36645,
#36646,#36647,#36648,#36649,#36650,#36651,#36652,#36653,#36654),(#36655,
#36656,#36657,#36658,#36659,#36660,#36661,#36662,#36663,#36664,#36665,#36666)),
 .UNSPECIFIED.,.F.,.F.,.F.)
B_SPLINE_SURFACE_WITH_KNOTS((4,4),(4,2,2,2,2,4),(0.,1.),(0.,0.0783698481609187,
0.30877738612019,0.539184924080125,0.769592462040063,1.),.UNSPECIFIED.)
GEOMETRIC_REPRESENTATION_ITEM()
RATIONAL_B_SPLINE_SURFACE(((1.,1.,1.,1.,1.,1.,1.,1.,1.,1.,1.,1.),(0.987189825241073,
0.987189825241073,0.987189825241073,0.987189825241073,0.987189825241073,
0.987189825241073,0.987189825241073,0.987189825241073,0.987189825241073,
0.987189825241073,0.987189825241073,0.987189825241073),(0.987189825241073,
0.987189825241073,0.987189825241073,0.987189825241073,0.987189825241073,
0.987189825241073,0.987189825241073,0.987189825241073,0.987189825241073,
0.987189825241073,0.987189825241073,0.987189825241073),(1.,1.,1.,1.,1.,
1.,1.,1.,1.,1.,1.,1.)))
REPRESENTATION_ITEM('')
SURFACE()
);
#582=(
BOUNDED_SURFACE()
B_SPLINE_SURFACE(3,3,((#36667,#36668,#36669,#36670,#36671,#36672,#36673,
#36674,#36675,#36676,#36677,#36678),(#36679,#36680,#36681,#36682,#36683,
#36684,#36685,#36686,#36687,#36688,#36689,#36690),(#36691,#36692,#36693,
#36694,#36695,#36696,#36697,#36698,#36699,#36700,#36701,#36702),(#36703,
#36704,#36705,#36706,#36707,#36708,#36709,#36710,#36711,#36712,#36713,#36714)),
 .UNSPECIFIED.,.F.,.F.,.F.)
B_SPLINE_SURFACE_WITH_KNOTS((4,4),(4,2,2,2,2,4),(0.,1.),(0.,0.0783698481609187,
0.30877738612019,0.539184924080125,0.769592462040063,1.),.UNSPECIFIED.)
GEOMETRIC_REPRESENTATION_ITEM()
RATIONAL_B_SPLINE_SURFACE(((1.,1.,1.,1.,1.,1.,1.,1.,1.,1.,1.,1.),(0.987189825241073,
0.987189825241073,0.987189825241073,0.987189825241073,0.987189825241073,
0.987189825241073,0.987189825241073,0.987189825241073,0.987189825241073,
0.987189825241073,0.987189825241073,0.987189825241073),(0.987189825241073,
0.987189825241073,0.987189825241073,0.987189825241073,0.987189825241073,
0.987189825241073,0.987189825241073,0.987189825241073,0.987189825241073,
0.987189825241073,0.987189825241073,0.987189825241073),(1.,1.,1.,1.,1.,
1.,1.,1.,1.,1.,1.,1.)))
REPRESENTATION_ITEM('')
SURFACE()
);
#583=(
BOUNDED_SURFACE()
B_SPLINE_SURFACE(3,3,((#36715,#36716,#36717,#36718,#36719,#36720,#36721,
#36722,#36723,#36724,#36725,#36726),(#36727,#36728,#36729,#36730,#36731,
#36732,#36733,#36734,#36735,#36736,#36737,#36738),(#36739,#36740,#36741,
#36742,#36743,#36744,#36745,#36746,#36747,#36748,#36749,#36750),(#36751,
#36752,#36753,#36754,#36755,#36756,#36757,#36758,#36759,#36760,#36761,#36762)),
 .UNSPECIFIED.,.F.,.F.,.F.)
B_SPLINE_SURFACE_WITH_KNOTS((4,4),(4,2,2,2,2,4),(0.,1.),(0.,0.0783698437311103,
0.308777382797833,0.539184921865221,0.76959246093261,1.),.UNSPECIFIED.)
GEOMETRIC_REPRESENTATION_ITEM()
RATIONAL_B_SPLINE_SURFACE(((1.,1.,1.,1.,1.,1.,1.,1.,1.,1.,1.,1.),(0.833333333333332,
0.833333333333332,0.833333333333332,0.833333333333332,0.833333333333332,
0.833333333333332,0.833333333333332,0.833333333333332,0.833333333333332,
0.833333333333332,0.833333333333332,0.833333333333332),(0.833333333333332,
0.833333333333332,0.833333333333332,0.833333333333332,0.833333333333332,
0.833333333333332,0.833333333333332,0.833333333333332,0.833333333333332,
0.833333333333332,0.833333333333332,0.833333333333332),(1.,1.,1.,1.,1.,
1.,1.,1.,1.,1.,1.,1.)))
REPRESENTATION_ITEM('')
SURFACE()
);
#584=(
BOUNDED_SURFACE()
B_SPLINE_SURFACE(3,3,((#36779,#36780,#36781,#36782,#36783,#36784,#36785,
#36786,#36787,#36788,#36789,#36790),(#36791,#36792,#36793,#36794,#36795,
#36796,#36797,#36798,#36799,#36800,#36801,#36802),(#36803,#36804,#36805,
#36806,#36807,#36808,#36809,#36810,#36811,#36812,#36813,#36814),(#36815,
#36816,#36817,#36818,#36819,#36820,#36821,#36822,#36823,#36824,#36825,#36826)),
 .UNSPECIFIED.,.F.,.F.,.F.)
B_SPLINE_SURFACE_WITH_KNOTS((4,4),(4,2,2,2,2,4),(0.,1.),(0.,0.0783698437311103,
0.308777382797833,0.539184921865221,0.76959246093261,1.),.UNSPECIFIED.)
GEOMETRIC_REPRESENTATION_ITEM()
RATIONAL_B_SPLINE_SURFACE(((1.,1.,1.,1.,1.,1.,1.,1.,1.,1.,1.,1.),(0.987189825241073,
0.987189825241073,0.987189825241073,0.987189825241073,0.987189825241073,
0.987189825241073,0.987189825241073,0.987189825241073,0.987189825241073,
0.987189825241073,0.987189825241073,0.987189825241073),(0.987189825241073,
0.987189825241073,0.987189825241073,0.987189825241073,0.987189825241073,
0.987189825241073,0.987189825241073,0.987189825241073,0.987189825241073,
0.987189825241073,0.987189825241073,0.987189825241073),(1.,1.,1.,1.,1.,
1.,1.,1.,1.,1.,1.,1.)))
REPRESENTATION_ITEM('')
SURFACE()
);
#585=(
BOUNDED_SURFACE()
B_SPLINE_SURFACE(3,3,((#36827,#36828,#36829,#36830,#36831,#36832,#36833,
#36834,#36835,#36836,#36837,#36838),(#36839,#36840,#36841,#36842,#36843,
#36844,#36845,#36846,#36847,#36848,#36849,#36850),(#36851,#36852,#36853,
#36854,#36855,#36856,#36857,#36858,#36859,#36860,#36861,#36862),(#36863,
#36864,#36865,#36866,#36867,#36868,#36869,#36870,#36871,#36872,#36873,#36874)),
 .UNSPECIFIED.,.F.,.F.,.F.)
B_SPLINE_SURFACE_WITH_KNOTS((4,4),(4,2,2,2,2,4),(0.,1.),(0.,0.0783698437311103,
0.308777382797833,0.539184921865221,0.76959246093261,1.),.UNSPECIFIED.)
GEOMETRIC_REPRESENTATION_ITEM()
RATIONAL_B_SPLINE_SURFACE(((1.,1.,1.,1.,1.,1.,1.,1.,1.,1.,1.,1.),(0.987189825241073,
0.987189825241073,0.987189825241073,0.987189825241073,0.987189825241073,
0.987189825241073,0.987189825241073,0.987189825241073,0.987189825241073,
0.987189825241073,0.987189825241073,0.987189825241073),(0.987189825241073,
0.987189825241073,0.987189825241073,0.987189825241073,0.987189825241073,
0.987189825241073,0.987189825241073,0.987189825241073,0.987189825241073,
0.987189825241073,0.987189825241073,0.987189825241073),(1.,1.,1.,1.,1.,
1.,1.,1.,1.,1.,1.,1.)))
REPRESENTATION_ITEM('')
SURFACE()
);
#586=(
BOUNDED_SURFACE()
B_SPLINE_SURFACE(3,3,((#36875,#36876,#36877,#36878,#36879,#36880,#36881,
#36882,#36883,#36884,#36885,#36886),(#36887,#36888,#36889,#36890,#36891,
#36892,#36893,#36894,#36895,#36896,#36897,#36898),(#36899,#36900,#36901,
#36902,#36903,#36904,#36905,#36906,#36907,#36908,#36909,#36910),(#36911,
#36912,#36913,#36914,#36915,#36916,#36917,#36918,#36919,#36920,#36921,#36922)),
 .UNSPECIFIED.,.F.,.F.,.F.)
B_SPLINE_SURFACE_WITH_KNOTS((4,4),(4,2,2,2,2,4),(0.,1.),(0.,0.0783698388401129,
0.308777379129585,0.539184919419723,0.769592459709861,1.),.UNSPECIFIED.)
GEOMETRIC_REPRESENTATION_ITEM()
RATIONAL_B_SPLINE_SURFACE(((1.,1.,1.,1.,1.,1.,1.,1.,1.,1.,1.,1.),(0.833333333333333,
0.833333333333333,0.833333333333333,0.833333333333333,0.833333333333333,
0.833333333333333,0.833333333333333,0.833333333333333,0.833333333333333,
0.833333333333333,0.833333333333333,0.833333333333333),(0.833333333333333,
0.833333333333333,0.833333333333333,0.833333333333333,0.833333333333333,
0.833333333333333,0.833333333333333,0.833333333333333,0.833333333333333,
0.833333333333333,0.833333333333333,0.833333333333333),(1.,1.,1.,1.,1.,
1.,1.,1.,1.,1.,1.,1.)))
REPRESENTATION_ITEM('')
SURFACE()
);
#587=(
BOUNDED_SURFACE()
B_SPLINE_SURFACE(3,3,((#36939,#36940,#36941,#36942,#36943,#36944,#36945,
#36946,#36947,#36948,#36949,#36950),(#36951,#36952,#36953,#36954,#36955,
#36956,#36957,#36958,#36959,#36960,#36961,#36962),(#36963,#36964,#36965,
#36966,#36967,#36968,#36969,#36970,#36971,#36972,#36973,#36974),(#36975,
#36976,#36977,#36978,#36979,#36980,#36981,#36982,#36983,#36984,#36985,#36986)),
 .UNSPECIFIED.,.F.,.F.,.F.)
B_SPLINE_SURFACE_WITH_KNOTS((4,4),(4,2,2,2,2,4),(0.,1.),(0.,0.0783698388401129,
0.308777379129585,0.539184919419723,0.769592459709861,1.),.UNSPECIFIED.)
GEOMETRIC_REPRESENTATION_ITEM()
RATIONAL_B_SPLINE_SURFACE(((1.,1.,1.,1.,1.,1.,1.,1.,1.,1.,1.,1.),(0.987189825241073,
0.987189825241073,0.987189825241073,0.987189825241073,0.987189825241073,
0.987189825241073,0.987189825241073,0.987189825241073,0.987189825241073,
0.987189825241073,0.987189825241073,0.987189825241073),(0.987189825241073,
0.987189825241073,0.987189825241073,0.987189825241073,0.987189825241073,
0.987189825241073,0.987189825241073,0.987189825241073,0.987189825241073,
0.987189825241073,0.987189825241073,0.987189825241073),(1.,1.,1.,1.,1.,
1.,1.,1.,1.,1.,1.,1.)))
REPRESENTATION_ITEM('')
SURFACE()
);
#588=(
BOUNDED_SURFACE()
B_SPLINE_SURFACE(3,3,((#36987,#36988,#36989,#36990,#36991,#36992,#36993,
#36994,#36995,#36996,#36997,#36998),(#36999,#37000,#37001,#37002,#37003,
#37004,#37005,#37006,#37007,#37008,#37009,#37010),(#37011,#37012,#37013,
#37014,#37015,#37016,#37017,#37018,#37019,#37020,#37021,#37022),(#37023,
#37024,#37025,#37026,#37027,#37028,#37029,#37030,#37031,#37032,#37033,#37034)),
 .UNSPECIFIED.,.F.,.F.,.F.)
B_SPLINE_SURFACE_WITH_KNOTS((4,4),(4,2,2,2,2,4),(0.,1.),(0.,0.0783698388401129,
0.308777379129585,0.539184919419723,0.769592459709861,1.),.UNSPECIFIED.)
GEOMETRIC_REPRESENTATION_ITEM()
RATIONAL_B_SPLINE_SURFACE(((1.,1.,1.,1.,1.,1.,1.,1.,1.,1.,1.,1.),(0.987189825241073,
0.987189825241073,0.987189825241073,0.987189825241073,0.987189825241073,
0.987189825241073,0.987189825241073,0.987189825241073,0.987189825241073,
0.987189825241073,0.987189825241073,0.987189825241073),(0.987189825241073,
0.987189825241073,0.987189825241073,0.987189825241073,0.987189825241073,
0.987189825241073,0.987189825241073,0.987189825241073,0.987189825241073,
0.987189825241073,0.987189825241073,0.987189825241073),(1.,1.,1.,1.,1.,
1.,1.,1.,1.,1.,1.,1.)))
REPRESENTATION_ITEM('')
SURFACE()
);
#589=(
BOUNDED_SURFACE()
B_SPLINE_SURFACE(3,3,((#37035,#37036,#37037,#37038,#37039,#37040,#37041,
#37042,#37043,#37044,#37045,#37046,#37047,#37048),(#37049,#37050,#37051,
#37052,#37053,#37054,#37055,#37056,#37057,#37058,#37059,#37060,#37061,#37062),
(#37063,#37064,#37065,#37066,#37067,#37068,#37069,#37070,#37071,#37072,
#37073,#37074,#37075,#37076),(#37077,#37078,#37079,#37080,#37081,#37082,
#37083,#37084,#37085,#37086,#37087,#37088,#37089,#37090)),.UNSPECIFIED.,
 .F.,.F.,.F.)
B_SPLINE_SURFACE_WITH_KNOTS((4,4),(4,2,2,2,2,2,4),(0.,1.),(0.,0.0183879232268686,
0.0783698352504293,0.308777376437322,0.53918491762488,0.769592458812441,
1.),.UNSPECIFIED.)
GEOMETRIC_REPRESENTATION_ITEM()
RATIONAL_B_SPLINE_SURFACE(((1.,1.,1.,1.,1.,1.,1.,1.,1.,1.,1.,1.,1.,1.),
(0.833333333333332,0.833333333333332,0.833333333333332,0.833333333333332,
0.833333333333332,0.833333333333332,0.833333333333332,0.833333333333332,
0.833333333333332,0.833333333333332,0.833333333333332,0.833333333333332,
0.833333333333332,0.833333333333332),(0.833333333333332,0.833333333333332,
0.833333333333332,0.833333333333332,0.833333333333332,0.833333333333332,
0.833333333333332,0.833333333333332,0.833333333333332,0.833333333333332,
0.833333333333332,0.833333333333332,0.833333333333332,0.833333333333332),
(1.,1.,1.,1.,1.,1.,1.,1.,1.,1.,1.,1.,1.,1.)))
REPRESENTATION_ITEM('')
SURFACE()
);
#590=(
BOUNDED_SURFACE()
B_SPLINE_SURFACE(3,3,((#37109,#37110,#37111,#37112,#37113,#37114,#37115,
#37116,#37117,#37118,#37119,#37120,#37121,#37122),(#37123,#37124,#37125,
#37126,#37127,#37128,#37129,#37130,#37131,#37132,#37133,#37134,#37135,#37136),
(#37137,#37138,#37139,#37140,#37141,#37142,#37143,#37144,#37145,#37146,
#37147,#37148,#37149,#37150),(#37151,#37152,#37153,#37154,#37155,#37156,
#37157,#37158,#37159,#37160,#37161,#37162,#37163,#37164)),.UNSPECIFIED.,
 .F.,.F.,.F.)
B_SPLINE_SURFACE_WITH_KNOTS((4,4),(4,2,2,2,2,2,4),(0.,1.),(0.,0.0183879232268686,
0.0783698352504293,0.308777376437322,0.53918491762488,0.769592458812441,
1.),.UNSPECIFIED.)
GEOMETRIC_REPRESENTATION_ITEM()
RATIONAL_B_SPLINE_SURFACE(((1.,1.,1.,1.,1.,1.,1.,1.,1.,1.,1.,1.,1.,1.),
(0.987189825241073,0.987189825241073,0.987189825241073,0.987189825241073,
0.987189825241073,0.987189825241073,0.987189825241073,0.987189825241073,
0.987189825241073,0.987189825241073,0.987189825241073,0.987189825241073,
0.987189825241073,0.987189825241073),(0.987189825241073,0.987189825241073,
0.987189825241073,0.987189825241073,0.987189825241073,0.987189825241073,
0.987189825241073,0.987189825241073,0.987189825241073,0.987189825241073,
0.987189825241073,0.987189825241073,0.987189825241073,0.987189825241073),
(1.,1.,1.,1.,1.,1.,1.,1.,1.,1.,1.,1.,1.,1.)))
REPRESENTATION_ITEM('')
SURFACE()
);
#591=(
BOUNDED_SURFACE()
B_SPLINE_SURFACE(3,3,((#37165,#37166,#37167,#37168,#37169,#37170,#37171,
#37172,#37173,#37174,#37175,#37176,#37177,#37178),(#37179,#37180,#37181,
#37182,#37183,#37184,#37185,#37186,#37187,#37188,#37189,#37190,#37191,#37192),
(#37193,#37194,#37195,#37196,#37197,#37198,#37199,#37200,#37201,#37202,
#37203,#37204,#37205,#37206),(#37207,#37208,#37209,#37210,#37211,#37212,
#37213,#37214,#37215,#37216,#37217,#37218,#37219,#37220)),.UNSPECIFIED.,
 .F.,.F.,.F.)
B_SPLINE_SURFACE_WITH_KNOTS((4,4),(4,2,2,2,2,2,4),(0.,1.),(0.,0.0183879232268686,
0.0783698352504293,0.308777376437322,0.53918491762488,0.769592458812441,
1.),.UNSPECIFIED.)
GEOMETRIC_REPRESENTATION_ITEM()
RATIONAL_B_SPLINE_SURFACE(((1.,1.,1.,1.,1.,1.,1.,1.,1.,1.,1.,1.,1.,1.),
(0.987189825241073,0.987189825241073,0.987189825241073,0.987189825241073,
0.987189825241073,0.987189825241073,0.987189825241073,0.987189825241073,
0.987189825241073,0.987189825241073,0.987189825241073,0.987189825241073,
0.987189825241073,0.987189825241073),(0.987189825241073,0.987189825241073,
0.987189825241073,0.987189825241073,0.987189825241073,0.987189825241073,
0.987189825241073,0.987189825241073,0.987189825241073,0.987189825241073,
0.987189825241073,0.987189825241073,0.987189825241073,0.987189825241073),
(1.,1.,1.,1.,1.,1.,1.,1.,1.,1.,1.,1.,1.,1.)))
REPRESENTATION_ITEM('')
SURFACE()
);
#592=CONICAL_SURFACE('',#11051,7.,0.785398163397443);
#593=CONICAL_SURFACE('',#11081,6.95000000000004,0.785398163397436);
#594=CONICAL_SURFACE('',#11243,41.5,0.785398163397442);
#595=CONICAL_SURFACE('',#11292,43.5,0.78539816339745);
#596=CONICAL_SURFACE('',#11795,3.47500000000001,0.785398163397447);
#597=B_SPLINE_CURVE_WITH_KNOTS('',3,(#14255,#14256,#14257,#14258,#14259,
#14260,#14261,#14262,#14263,#14264,#14265,#14266,#14267,#14268,#14269,#14270,
#14271,#14272,#14273,#14274),.UNSPECIFIED.,.F.,.F.,(4,2,2,2,2,2,2,2,2,4),
(21.0628184025214,21.4115217399649,21.7865786122948,22.1603740098871,22.5335858127541,
22.9068981706492,23.2810500826543,23.656846922793,23.8644254006208,24.0718313053738),
 .UNSPECIFIED.);
#598=B_SPLINE_CURVE_WITH_KNOTS('',3,(#14278,#14279,#14280,#14281,#14282,
#14283,#14284,#14285,#14286,#14287,#14288,#14289,#14290,#14291,#14292,#14293,
#14294,#14295,#14296,#14297),.UNSPECIFIED.,.F.,.F.,(4,2,2,2,2,2,2,2,2,4),
(0.,0.207250737328132,0.414673918623437,0.790189612340599,1.16406160855106,
1.5370946787505,1.91002726915051,2.28354301766879,2.65831929717239,3.00676175776697),
 .UNSPECIFIED.);
#599=B_SPLINE_CURVE_WITH_KNOTS('',3,(#14301,#14302,#14303,#14304,#14305,
#14306,#14307,#14308,#14309,#14310,#14311,#14312,#14313,#14314,#14315,#14316,
#14317,#14318,#14319,#14320,#14321,#14322,#14323,#14324,#14325,#14326,#14327,
#14328,#14329,#14330,#14331,#14332,#14333,#14334,#14335,#14336),
 .UNSPECIFIED.,.F.,.F.,(4,2,2,2,2,2,2,2,2,2,2,2,2,2,2,2,2,4),(3.00676175776697,
3.03504667108494,3.41221154887637,3.78733667813517,4.16097374899924,4.53391428123984,
4.90688520324459,5.28056485337379,5.65563224159108,6.03278211267235,6.40960760837217,
6.78447515598402,7.15800677331664,7.5309813026748,7.90411426490854,8.27808194278114,
8.65356504512735,9.02205372355402),.UNSPECIFIED.);
#600=B_SPLINE_CURVE_WITH_KNOTS('',3,(#14341,#14342,#14343,#14344,#14345,
#14346,#14347,#14348,#14349,#14350,#14351,#14352,#14353,#14354,#14355,#14356,
#14357,#14358,#14359,#14360,#14361,#14362,#14363,#14364,#14365,#14366,#14367,
#14368,#14369,#14370,#14371,#14372,#14373,#14374,#14375,#14376),
 .UNSPECIFIED.,.F.,.F.,(4,2,2,2,2,2,2,2,2,2,2,2,2,2,2,2,2,4),(15.0430228225335,
15.4117873862963,15.7875516106631,16.1617992759669,16.535211600685,16.9084653739098,
17.2822766521976,17.6574248609679,18.0345324837305,18.4119647247325,18.7873129237276,
19.1612723456431,19.5345225088135,19.9077422594671,20.2816590702386,20.6570650535055,
21.034512312453,21.0628184025214),.UNSPECIFIED.);
#601=B_SPLINE_CURVE_WITH_KNOTS('',3,(#14377,#14378,#14379,#14380,#14381,
#14382,#14383,#14384,#14385,#14386,#14387,#14388,#14389,#14390,#14391,#14392,
#14393,#14394,#14395,#14396,#14397,#14398,#14399,#14400,#14401,#14402,#14403,
#14404,#14405,#14406,#14407,#14408,#14409,#14410,#14411,#14412,#14413,#14414),
 .UNSPECIFIED.,.F.,.F.,(4,2,2,2,2,2,2,2,2,2,2,2,2,2,2,2,2,2,4),(9.02205372355402,
9.03126316823583,9.40786592412534,9.78261257335366,10.1561697915982,10.5293045591898,
10.9027222320504,11.2770985056625,11.6531165926403,12.0313420273241,12.4094238490597,
12.7851606240943,13.1592568140597,13.5323951204357,13.9052507331937,14.278528480555,
14.6529947690463,15.0293157755821,15.0385183303645),.UNSPECIFIED.);
#602=B_SPLINE_CURVE_WITH_KNOTS('',3,(#14419,#14420,#14421,#14422,#14423,
#14424,#14425,#14426,#14427,#14428,#14429,#14430,#14431,#14432,#14433,#14434,
#14435,#14436,#14437,#14438,#14439,#14440,#14441,#14442,#14443,#14444,#14445,
#14446,#14447,#14448,#14449,#14450,#14451,#14452,#14453,#14454,#14455,#14456),
 .UNSPECIFIED.,.F.,.F.,(4,2,2,2,2,2,2,2,2,2,2,2,2,2,2,2,2,2,4),(9.02205372357257,
9.03126316825438,9.4078659241447,9.78261257337381,10.1561697916191,10.5293045592115,
10.9027222320728,11.2770985056855,11.653116592664,12.0314814820664,12.409990091939,
12.7862897014773,13.1609462684338,13.5346435169401,13.9080576483678,14.2818945467347,
14.6569217666056,15.0338064827939,15.0430228225335),.UNSPECIFIED.);
#603=B_SPLINE_CURVE_WITH_KNOTS('',3,(#14457,#14458,#14459,#14460,#14461,
#14462,#14463,#14464,#14465,#14466,#14467,#14468,#14469,#14470,#14471,#14472,
#14473,#14474,#14475,#14476,#14477,#14478,#14479,#14480,#14481,#14482,#14483,
#14484,#14485,#14486,#14487,#14488,#14489,#14490,#14491,#14492),
 .UNSPECIFIED.,.F.,.F.,(4,2,2,2,2,2,2,2,2,2,2,2,2,2,2,2,2,4),(15.0385183303645,
15.4067313298554,15.7819335204988,16.1556214204093,16.5284752291602,16.9011707235645,
17.2744228891668,17.6490099855933,18.0255535653001,18.4024212777122,18.7772080652366,
19.1506081528872,19.523300042637,19.8959615653583,20.2693191055988,20.6441635909667,
21.021046298862,21.0493100512724),.UNSPECIFIED.);
#604=B_SPLINE_CURVE_WITH_KNOTS('',3,(#14497,#14498,#14499,#14500,#14501,
#14502,#14503,#14504,#14505,#14506,#14507,#14508,#14509,#14510,#14511,#14512,
#14513,#14514,#14515,#14516,#14517,#14518,#14519,#14520,#14521,#14522,#14523,
#14524,#14525,#14526,#14527,#14528,#14529,#14530,#14531,#14532),
 .UNSPECIFIED.,.F.,.F.,(4,2,2,2,2,2,2,2,2,2,2,2,2,2,2,2,2,4),(3.0067617577732,
3.03504667109116,3.41221154888342,3.78733667814306,4.16097374900799,4.53391428124943,
4.90688520325496,5.28056485338495,5.65563224160295,6.03278211268495,6.40960760838549,
6.78447515599804,7.1580067733314,7.53098130269032,7.90411426492479,8.27808194279812,
8.65356504514509,9.02205372357257),.UNSPECIFIED.);
#605=B_SPLINE_CURVE_WITH_KNOTS('',3,(#14534,#14535,#14536,#14537,#14538,
#14539,#14540,#14541,#14542,#14543,#14544,#14545,#14546,#14547,#14548,#14549,
#14550,#14551,#14552,#14553),.UNSPECIFIED.,.F.,.F.,(4,2,2,2,2,2,2,2,2,4),
(21.0493100512724,21.3974918301899,21.771987726789,22.145224035449,22.5178776222712,
22.8906316137205,23.2642239035516,23.6394586611834,23.8467266621291,24.0538223481184),
 .UNSPECIFIED.);
#606=B_SPLINE_CURVE_WITH_KNOTS('',3,(#14554,#14555,#14556,#14557,#14558,
#14559,#14560,#14561,#14562,#14563,#14564,#14565,#14566,#14567,#14568,#14569,
#14570,#14571,#14572,#14573),.UNSPECIFIED.,.F.,.F.,(4,2,2,2,2,2,2,2,2,4),
(-24.0754558847043,-23.8386618118089,-23.6022771218884,-23.2241633619335,
-22.8481775712266,-22.4739359229648,-22.1006247072007,-21.7274979336969,
-21.3538666435424,-21.0666269184095),.UNSPECIFIED.);
#607=B_SPLINE_CURVE_WITH_KNOTS('',3,(#14579,#14580,#14581,#14582,#14583,
#14584,#14585,#14586,#14587,#14588,#14589,#14590,#14591,#14592,#14593,#14594,
#14595,#14596,#14597,#14598),.UNSPECIFIED.,.F.,.F.,(4,2,2,2,2,2,2,2,2,4),
(-3.0067617577744,-2.658319297179,-2.28354301767456,-1.91002726915535,-1.5370946787543,
-1.16406160855382,-0.790189612342309,-0.414673918624121,-0.207250737328291,
0.),.UNSPECIFIED.);
#608=B_SPLINE_CURVE_WITH_KNOTS('',3,(#14599,#14600,#14601,#14602,#14603,
#14604,#14605,#14606,#14607,#14608,#14609,#14610,#14611,#14612,#14613,#14614,
#14615,#14616,#14617,#14618),.UNSPECIFIED.,.F.,.F.,(4,2,2,2,2,2,2,2,2,4),
(0.,0.207250737328221,0.414673918623899,0.790189612341872,1.16406160855318,
1.53709467875346,1.91002726915431,2.28354301767339,2.65831929717779,3.0067617577732),
 .UNSPECIFIED.);
#609=B_SPLINE_CURVE_WITH_KNOTS('',3,(#14619,#14620,#14621,#14622,#14623,
#14624,#14625,#14626,#14627,#14628,#14629,#14630,#14631,#14632,#14633,#14634,
#14635,#14636,#14637,#14638,#14639,#14640,#14641,#14642,#14643,#14644,#14645,
#14646,#14647,#14648,#14649,#14650,#14651,#14652,#14653,#14654),
 .UNSPECIFIED.,.F.,.F.,(4,2,2,2,2,2,2,2,2,2,2,2,2,2,2,2,2,4),(-21.0666269184095,
-20.9790541549754,-20.6023718836333,-20.2247774596021,-19.8492645538475,
-19.4753390547256,-19.1022007374592,-18.7291148841734,-18.3554001957568,
-17.9803782798469,-17.6033568499733,-17.226173511323,-16.8510033824804,
-16.4772659751798,-16.1041741425224,-15.7310049385523,-15.3570806750968,
-15.0492520168156),.UNSPECIFIED.);
#610=B_SPLINE_CURVE_WITH_KNOTS('',3,(#14659,#14660,#14661,#14662,#14663,
#14664,#14665,#14666,#14667,#14668,#14669,#14670,#14671,#14672,#14673,#14674,
#14675,#14676,#14677,#14678,#14679,#14680,#14681,#14682,#14683,#14684,#14685,
#14686,#14687,#14688,#14689,#14690,#14691,#14692,#14693,#14694),
 .UNSPECIFIED.,.F.,.F.,(4,2,2,2,2,2,2,2,2,2,2,2,2,2,2,2,2,4),(-9.02205372357525,
-8.65356504514781,-8.27808194280083,-7.90411426492742,-7.53098130269283,
-7.15800677333379,-6.7844751560003,-6.40960760838759,-6.03278211268689,
-5.65563224160473,-5.28056485338656,-4.90688520325647,-4.53391428125088,
-4.1609737490094,-3.78733667814442,-3.41221154888473,-3.03504667109241,
-3.0067617577744),.UNSPECIFIED.);
#611=B_SPLINE_CURVE_WITH_KNOTS('',3,(#14695,#14696,#14697,#14698,#14699,
#14700,#14701,#14702,#14703,#14704,#14705,#14706,#14707,#14708,#14709,#14710,
#14711,#14712,#14713,#14714,#14715,#14716,#14717,#14718,#14719,#14720,#14721,
#14722,#14723,#14724,#14725,#14726,#14727,#14728,#14729,#14730),
 .UNSPECIFIED.,.F.,.F.,(4,2,2,2,2,2,2,2,2,2,2,2,2,2,2,2,2,4),(-15.0492520168156,
-14.9817215424698,-14.6042308135452,-14.2273450835583,-13.8523832079359,
-13.4787036832509,-13.1051113288905,-12.731947500807,-12.3585179295024,
-11.9840694865962,-11.6077801414908,-11.2293450863848,-10.8529730003901,
-10.4782699148012,-10.1045515865236,-9.73114186705801,-9.35733692632237,
-9.02845397887332),.UNSPECIFIED.);
#612=B_SPLINE_CURVE_WITH_KNOTS('',3,(#14737,#14738,#14739,#14740,#14741,
#14742,#14743,#14744,#14745,#14746,#14747,#14748,#14749,#14750,#14751,#14752,
#14753,#14754,#14755,#14756,#14757,#14758,#14759,#14760,#14761,#14762,#14763,
#14764,#14765,#14766,#14767,#14768,#14769,#14770,#14771,#14772),
 .UNSPECIFIED.,.F.,.F.,(4,2,2,2,2,2,2,2,2,2,2,2,2,2,2,2,2,4),(-21.062818402533,
-21.0345123124645,-20.6570650535164,-20.2816590702489,-19.9077422594767,
-19.5345225088225,-19.1612723456515,-18.7873129237354,-18.4119647247398,
-18.0345324837374,-17.6574248609745,-17.282276652204,-16.9084653739158,
-16.5352116006907,-16.1617992759723,-15.7875516106682,-15.411787386301,
-15.043022822538),.UNSPECIFIED.);
#613=B_SPLINE_CURVE_WITH_KNOTS('',3,(#14776,#14777,#14778,#14779,#14780,
#14781,#14782,#14783,#14784,#14785,#14786,#14787,#14788,#14789,#14790,#14791,
#14792,#14793,#14794,#14795),.UNSPECIFIED.,.F.,.F.,(4,2,2,2,2,2,2,2,2,4),
(-3.00896219087705,-2.9826900908492,-2.60537804402198,-2.22834522787004,
-1.85329206455909,-1.4795267572371,-1.10637111311519,-0.733142615483747,
-0.359104705713691,0.),.UNSPECIFIED.);
#614=B_SPLINE_CURVE_WITH_KNOTS('',3,(#14798,#14799,#14800,#14801,#14802,
#14803,#14804,#14805,#14806,#14807,#14808,#14809,#14810,#14811,#14812,#14813,
#14814,#14815,#14816,#14817),.UNSPECIFIED.,.F.,.F.,(4,2,2,2,2,2,2,2,2,4),
(-24.0718313053899,-23.8644254006373,-23.6568469228092,-23.2810500826698,
-22.906898170664,-22.5335858127682,-22.1603740099005,-21.7865786123075,
-21.4115217399771,-21.062818402533),.UNSPECIFIED.);
#615=B_SPLINE_CURVE_WITH_KNOTS('',3,(#14851,#14852,#14853,#14854,#14855,
#14856,#14857,#14858,#14859,#14860,#14861,#14862,#14863,#14864,#14865,#14866,
#14867,#14868,#14869,#14870,#14871,#14872,#14873,#14874,#14875,#14876,#14877,
#14878,#14879,#14880,#14881,#14882,#14883,#14884,#14885,#14886,#14887,#14888),
 .UNSPECIFIED.,.F.,.F.,(4,2,2,2,2,2,2,2,2,2,2,2,2,2,2,2,2,2,4),(-15.043022822538,
-15.0338064827984,-14.6569217666099,-14.2818945467388,-13.9080576483717,
-13.5346435169439,-13.1609462684376,-12.7862897014809,-12.4099900919424,
-12.0314814820696,-11.6531165926671,-11.2770985056884,-10.9027222320755,
-10.5293045592142,-10.1561697916218,-9.78261257337648,-9.40786592414737,
-9.03126316825707,-9.02205372357525),.UNSPECIFIED.);
#616=B_SPLINE_CURVE_WITH_KNOTS('',3,(#14889,#14890,#14891,#14892,#14893,
#14894,#14895,#14896,#14897,#14898,#14899,#14900,#14901,#14902,#14903,#14904,
#14905,#14906,#14907,#14908,#14909,#14910,#14911,#14912,#14913,#14914,#14915,
#14916,#14917,#14918,#14919,#14920,#14921,#14922,#14923,#14924),
 .UNSPECIFIED.,.F.,.F.,(4,2,2,2,2,2,2,2,2,2,2,2,2,2,2,2,2,4),(-9.02845397887332,
-8.98237168672322,-8.60557289800359,-8.22751630078672,-7.85170383973507,
-7.47743440461333,-7.10402641355928,-6.73080341422908,-6.35705169861502,
-5.98199451794767,-5.60499798633059,-5.22751545270559,-4.85214443892414,
-4.47818881415784,-4.10496887288142,-3.7318064281611,-3.35797659467942,
-3.00896219087705),.UNSPECIFIED.);
#617=B_SPLINE_CURVE_WITH_KNOTS('',3,(#17305,#17306,#17307,#17308,#17309,
#17310),.UNSPECIFIED.,.F.,.F.,(4,2,4),(-0.662095257781061,-0.331862946603713,
0.),.UNSPECIFIED.);
#618=B_SPLINE_CURVE_WITH_KNOTS('',3,(#17312,#17313,#17314,#17315,#17316,
#17317),.UNSPECIFIED.,.F.,.F.,(4,2,4),(-0.662021637365085,-0.331728159060927,
-1.00000001779232E-6),.UNSPECIFIED.);
#619=B_SPLINE_CURVE_WITH_KNOTS('',3,(#17321,#17322,#17323,#17324,#17325,
#17326,#17327,#17328,#17329,#17330,#17331,#17332,#17333,#17334),
 .UNSPECIFIED.,.F.,.F.,(4,2,2,2,2,2,4),(-0.662550701758967,-0.621305253814006,
-0.580038858839952,-0.497447618999927,-0.332066833308241,-0.165873822514336,
-1.00000000924361E-6),.UNSPECIFIED.);
#620=B_SPLINE_CURVE_WITH_KNOTS('',3,(#17336,#17337,#17338,#17339,#17340,
#17341),.UNSPECIFIED.,.F.,.F.,(4,2,4),(-0.663826635786988,-0.332807172053614,
-1.00000002301037E-6),.UNSPECIFIED.);
#621=B_SPLINE_CURVE_WITH_KNOTS('',3,(#17346,#17347,#17348,#17349,#17350,
#17351),.UNSPECIFIED.,.F.,.F.,(4,2,4),(-0.662095257781062,-0.33186294660371,
0.),.UNSPECIFIED.);
#622=B_SPLINE_CURVE_WITH_KNOTS('',3,(#17353,#17354,#17355,#17356,#17357,
#17358),.UNSPECIFIED.,.F.,.F.,(4,2,4),(-0.662021637522678,-0.331728159132817,
-1.00000001790335E-6),.UNSPECIFIED.);
#623=B_SPLINE_CURVE_WITH_KNOTS('',3,(#17362,#17363,#17364,#17365,#17366,
#17367,#17368,#17369,#17370,#17371,#17372,#17373,#17374,#17375),
 .UNSPECIFIED.,.F.,.F.,(4,2,2,2,2,2,4),(-0.662550616898668,-0.6212954808642,
-0.580019388663314,-0.49740872650569,-0.331989034460226,-0.165834990380567,
-1.0000000096877E-6),.UNSPECIFIED.);
#624=B_SPLINE_CURVE_WITH_KNOTS('',3,(#17377,#17378,#17379,#17380,#17381,
#17382),.UNSPECIFIED.,.F.,.F.,(4,2,4),(-0.663826635787034,-0.332807172053613,
-1.00000001879152E-6),.UNSPECIFIED.);
#625=B_SPLINE_CURVE_WITH_KNOTS('',3,(#17387,#17388,#17389,#17390,#17391,
#17392),.UNSPECIFIED.,.F.,.F.,(4,2,4),(-0.662095257781165,-0.331862946603753,
0.),.UNSPECIFIED.);
#626=B_SPLINE_CURVE_WITH_KNOTS('',3,(#17394,#17395,#17396,#17397,#17398,
#17399,#17400,#17401,#17402,#17403,#17404,#17405),.UNSPECIFIED.,.F.,.F.,
(4,2,2,2,2,4),(-0.660887316856551,-0.330884876596039,-0.165221392328677,
-0.0825519623367623,-0.0412673951611145,-9.99999991702083E-7),
 .UNSPECIFIED.);
#627=B_SPLINE_CURVE_WITH_KNOTS('',3,(#17409,#17410,#17411,#17412,#17413,
#17414,#17415,#17416,#17417,#17418,#17419,#17420,#17421,#17422),
 .UNSPECIFIED.,.F.,.F.,(4,2,2,2,2,2,4),(-0.662550616898348,-0.62129548086367,
-0.580019388662482,-0.497408726504859,-0.331989034460108,-0.165834990380633,
-1.00000000902156E-6),.UNSPECIFIED.);
#628=B_SPLINE_CURVE_WITH_KNOTS('',3,(#17424,#17425,#17426,#17427,#17428,
#17429),.UNSPECIFIED.,.F.,.F.,(4,2,4),(-0.663826635787024,-0.332807172053626,
-1.00000002301037E-6),.UNSPECIFIED.);
#629=B_SPLINE_CURVE_WITH_KNOTS('',3,(#17434,#17435,#17436,#17437,#17438,
#17439),.UNSPECIFIED.,.F.,.F.,(4,2,4),(-0.662095257781074,-0.331862946603717,
0.),.UNSPECIFIED.);
#630=B_SPLINE_CURVE_WITH_KNOTS('',3,(#17441,#17442,#17443,#17444,#17445,
#17446),.UNSPECIFIED.,.F.,.F.,(4,2,4),(-0.662021637922561,-0.331728159315548,
-1.00000001779232E-6),.UNSPECIFIED.);
#631=B_SPLINE_CURVE_WITH_KNOTS('',3,(#17450,#17451,#17452,#17453,#17454,
#17455,#17456,#17457),.UNSPECIFIED.,.F.,.F.,(4,2,2,4),(-0.663085280601993,
-0.331989035234756,-0.165834990767375,-1.00000000935463E-6),
 .UNSPECIFIED.);
#632=B_SPLINE_CURVE_WITH_KNOTS('',3,(#17459,#17460,#17461,#17462,#17463,
#17464),.UNSPECIFIED.,.F.,.F.,(4,2,4),(-0.663826635786995,-0.332807172053617,
-1.00000001901357E-6),.UNSPECIFIED.);
#633=B_SPLINE_CURVE_WITH_KNOTS('',3,(#17469,#17470,#17471,#17472,#17473,
#17474),.UNSPECIFIED.,.F.,.F.,(4,2,4),(-0.662095257781122,-0.33186294660374,
0.),.UNSPECIFIED.);
#634=B_SPLINE_CURVE_WITH_KNOTS('',3,(#17476,#17477,#17478,#17479,#17480,
#17481),.UNSPECIFIED.,.F.,.F.,(4,2,4),(-0.662021637998179,-0.331728159349608,
-1.0000000176813E-6),.UNSPECIFIED.);
#635=B_SPLINE_CURVE_WITH_KNOTS('',3,(#17485,#17486,#17487,#17488,#17489,
#17490,#17491,#17492,#17493,#17494,#17495,#17496,#17497,#17498),
 .UNSPECIFIED.,.F.,.F.,(4,2,2,2,2,2,4),(-0.662550616895752,-0.621295480861997,
-0.580019388660938,-0.497408726503312,-0.331989034459601,-0.165834990381051,
-1.00000000891054E-6),.UNSPECIFIED.);
#636=B_SPLINE_CURVE_WITH_KNOTS('',3,(#17500,#17501,#17502,#17503,#17504,
#17505),.UNSPECIFIED.,.F.,.F.,(4,2,4),(-0.663826635786914,-0.332807172053552,
-1.00000002090095E-6),.UNSPECIFIED.);
#637=B_SPLINE_CURVE_WITH_KNOTS('',3,(#17510,#17511,#17512,#17513,#17514,
#17515),.UNSPECIFIED.,.F.,.F.,(4,2,4),(-0.662095257781135,-0.331862946603749,
0.),.UNSPECIFIED.);
#638=B_SPLINE_CURVE_WITH_KNOTS('',3,(#17517,#17518,#17519,#17520,#17521,
#17522),.UNSPECIFIED.,.F.,.F.,(4,2,4),(-0.662021637997819,-0.331728159349464,
-1.0000000176813E-6),.UNSPECIFIED.);
#639=B_SPLINE_CURVE_WITH_KNOTS('',3,(#17526,#17527,#17528,#17529,#17530,
#17531,#17532,#17533,#17534,#17535,#17536,#17537,#17538,#17539),
 .UNSPECIFIED.,.F.,.F.,(4,2,2,2,2,2,4),(-0.66255061689952,-0.62129548086583,
-0.58001938866469,-0.497408726506779,-0.331989034460727,-0.165834990380612,
-1.00000000902156E-6),.UNSPECIFIED.);
#640=B_SPLINE_CURVE_WITH_KNOTS('',3,(#17541,#17542,#17543,#17544,#17545,
#17546),.UNSPECIFIED.,.F.,.F.,(4,2,4),(-0.663826635787004,-0.332807172053617,
-1.0000000216781E-6),.UNSPECIFIED.);
#641=B_SPLINE_CURVE_WITH_KNOTS('',3,(#17551,#17552,#17553,#17554,#17555,
#17556),.UNSPECIFIED.,.F.,.F.,(4,2,4),(-0.662095257781009,-0.331862946603692,
0.),.UNSPECIFIED.);
#642=B_SPLINE_CURVE_WITH_KNOTS('',3,(#17558,#17559,#17560,#17561,#17562,
#17563),.UNSPECIFIED.,.F.,.F.,(4,2,4),(-0.662021637880972,-0.331728159296021,
-1.0000000176813E-6),.UNSPECIFIED.);
#643=B_SPLINE_CURVE_WITH_KNOTS('',3,(#17567,#17568,#17569,#17570,#17571,
#17572,#17573,#17574,#17575,#17576,#17577,#17578,#17579,#17580),
 .UNSPECIFIED.,.F.,.F.,(4,2,2,2,2,2,4),(-0.66255061689857,-0.621295480864233,
-0.580019388662843,-0.497408726505221,-0.331989034460455,-0.165834990380495,
-1.00000000813338E-6),.UNSPECIFIED.);
#644=B_SPLINE_CURVE_WITH_KNOTS('',3,(#17582,#17583,#17584,#17585,#17586,
#17587),.UNSPECIFIED.,.F.,.F.,(4,2,4),(-0.66382663578703,-0.332807172053612,
-1.00000001945766E-6),.UNSPECIFIED.);
#645=B_SPLINE_CURVE_WITH_KNOTS('',3,(#17592,#17593,#17594,#17595,#17596,
#17597),.UNSPECIFIED.,.F.,.F.,(4,2,4),(-0.66209525778118,-0.331862946603774,
0.),.UNSPECIFIED.);
#646=B_SPLINE_CURVE_WITH_KNOTS('',3,(#17599,#17600,#17601,#17602,#17603,
#17604),.UNSPECIFIED.,.F.,.F.,(4,2,4),(-0.662021637714287,-0.331728159220456,
-1.00000001745926E-6),.UNSPECIFIED.);
#647=B_SPLINE_CURVE_WITH_KNOTS('',3,(#17608,#17609,#17610,#17611,#17612,
#17613,#17614,#17615,#17616,#17617,#17618,#17619,#17620,#17621),
 .UNSPECIFIED.,.F.,.F.,(4,2,2,2,2,2,4),(-0.662550616897935,-0.621295480863862,
-0.580019388662615,-0.497408726505072,-0.331989034460079,-0.16583499038102,
-1.00000000979872E-6),.UNSPECIFIED.);
#648=B_SPLINE_CURVE_WITH_KNOTS('',3,(#17623,#17624,#17625,#17626,#17627,
#17628),.UNSPECIFIED.,.F.,.F.,(4,2,4),(-0.663826635787039,-0.332807172053655,
-1.00000002345446E-6),.UNSPECIFIED.);
#649=B_SPLINE_CURVE_WITH_KNOTS('',3,(#17633,#17634,#17635,#17636,#17637,
#17638),.UNSPECIFIED.,.F.,.F.,(4,2,4),(-0.662095257781127,-0.331862946603734,
0.),.UNSPECIFIED.);
#650=B_SPLINE_CURVE_WITH_KNOTS('',3,(#17640,#17641,#17642,#17643,#17644,
#17645),.UNSPECIFIED.,.F.,.F.,(4,2,4),(-0.66202163751964,-0.331728159131613,
-1.00000001790335E-6),.UNSPECIFIED.);
#651=B_SPLINE_CURVE_WITH_KNOTS('',3,(#17649,#17650,#17651,#17652,#17653,
#17654,#17655,#17656,#17657,#17658,#17659,#17660,#17661,#17662),
 .UNSPECIFIED.,.F.,.F.,(4,2,2,2,2,2,4),(-0.662550616899407,-0.621295480865396,
-0.580019388664292,-0.497408726506504,-0.33198903446057,-0.165834990380615,
-1.00000000791134E-6),.UNSPECIFIED.);
#652=B_SPLINE_CURVE_WITH_KNOTS('',3,(#17664,#17665,#17666,#17667,#17668,
#17669),.UNSPECIFIED.,.F.,.F.,(4,2,4),(-0.66382663578689,-0.332807172053566,
-1.00000002201117E-6),.UNSPECIFIED.);
#653=B_SPLINE_CURVE_WITH_KNOTS('',3,(#17674,#17675,#17676,#17677,#17678,
#17679),.UNSPECIFIED.,.F.,.F.,(4,2,4),(-0.662095257781152,-0.331862946603746,
0.),.UNSPECIFIED.);
#654=B_SPLINE_CURVE_WITH_KNOTS('',3,(#17681,#17682,#17683,#17684,#17685,
#17686),.UNSPECIFIED.,.F.,.F.,(4,2,4),(-0.662021637368216,-0.331728159062471,
-1.00000001779232E-6),.UNSPECIFIED.);
#655=B_SPLINE_CURVE_WITH_KNOTS('',3,(#17690,#17691,#17692,#17693,#17694,
#17695,#17696,#17697,#17698,#17699,#17700,#17701,#17702,#17703),
 .UNSPECIFIED.,.F.,.F.,(4,2,2,2,2,2,4),(-0.662550616898824,-0.621295480864527,
-0.580019388663592,-0.497408726505791,-0.331989034460403,-0.165834990380775,
-1.00000000935463E-6),.UNSPECIFIED.);
#656=B_SPLINE_CURVE_WITH_KNOTS('',3,(#17705,#17706,#17707,#17708,#17709,
#17710),.UNSPECIFIED.,.F.,.F.,(4,2,4),(-0.663826635787064,-0.332807172053641,
-1.0000000216781E-6),.UNSPECIFIED.);
#657=B_SPLINE_CURVE_WITH_KNOTS('',3,(#17715,#17716,#17717,#17718,#17719,
#17720),.UNSPECIFIED.,.F.,.F.,(4,2,4),(-0.662095257781144,-0.331862946603761,
0.),.UNSPECIFIED.);
#658=B_SPLINE_CURVE_WITH_KNOTS('',3,(#17722,#17723,#17724,#17725,#17726,
#17727),.UNSPECIFIED.,.F.,.F.,(4,2,4),(-0.662021637123029,-0.331728158950561,
-1.00000001779232E-6),.UNSPECIFIED.);
#659=B_SPLINE_CURVE_WITH_KNOTS('',3,(#17731,#17732,#17733,#17734,#17735,
#17736,#17737,#17738,#17739,#17740,#17741,#17742,#17743,#17744),
 .UNSPECIFIED.,.F.,.F.,(4,2,2,2,2,2,4),(-0.662550616899271,-0.621295480864664,
-0.580019388663568,-0.497408726505942,-0.331989034460324,-0.165834990380964,
-1.00000000957667E-6),.UNSPECIFIED.);
#660=B_SPLINE_CURVE_WITH_KNOTS('',3,(#17746,#17747,#17748,#17749,#17750,
#17751),.UNSPECIFIED.,.F.,.F.,(4,2,4),(-0.663826635786987,-0.332807172053595,
-1.00000002278833E-6),.UNSPECIFIED.);
#661=B_SPLINE_CURVE_WITH_KNOTS('',3,(#17756,#17757,#17758,#17759,#17760,
#17761),.UNSPECIFIED.,.F.,.F.,(4,2,4),(-0.662095257780937,-0.331862946603657,
0.),.UNSPECIFIED.);
#662=B_SPLINE_CURVE_WITH_KNOTS('',3,(#17763,#17764,#17765,#17766,#17767,
#17768,#17769,#17770,#17771,#17772,#17773,#17774),.UNSPECIFIED.,.F.,.F.,
(4,2,2,2,2,4),(-0.660887316879566,-0.330884876607085,-0.165221392333038,
-0.0825519623381546,-0.0412673951613865,-9.99999991702083E-7),
 .UNSPECIFIED.);
#663=B_SPLINE_CURVE_WITH_KNOTS('',3,(#17778,#17779,#17780,#17781,#17782,
#17783,#17784,#17785,#17786,#17787,#17788,#17789,#17790,#17791),
 .UNSPECIFIED.,.F.,.F.,(4,2,2,2,2,2,4),(-0.662550616900091,-0.621295480865225,
-0.580019388664242,-0.497408726506713,-0.331989034460346,-0.165834990380543,
-1.00000000913258E-6),.UNSPECIFIED.);
#664=B_SPLINE_CURVE_WITH_KNOTS('',3,(#17793,#17794,#17795,#17796,#17797,
#17798),.UNSPECIFIED.,.F.,.F.,(4,2,4),(-0.663826635786934,-0.332807172053606,
-1.00000002178913E-6),.UNSPECIFIED.);
#665=B_SPLINE_CURVE_WITH_KNOTS('',3,(#17803,#17804,#17805,#17806,#17807,
#17808),.UNSPECIFIED.,.F.,.F.,(4,2,4),(-0.662095257781237,-0.331862946603812,
0.),.UNSPECIFIED.);
#666=B_SPLINE_CURVE_WITH_KNOTS('',3,(#17810,#17811,#17812,#17813,#17814,
#17815),.UNSPECIFIED.,.F.,.F.,(4,2,4),(-0.662021637516076,-0.331728159129799,
-1.00000001790335E-6),.UNSPECIFIED.);
#667=B_SPLINE_CURVE_WITH_KNOTS('',3,(#17819,#17820,#17821,#17822,#17823,
#17824,#17825,#17826),.UNSPECIFIED.,.F.,.F.,(4,2,2,4),(-0.663085280603729,
-0.331989035234337,-0.165834990767195,-1.00000000924361E-6),
 .UNSPECIFIED.);
#668=B_SPLINE_CURVE_WITH_KNOTS('',3,(#17828,#17829,#17830,#17831,#17832,
#17833),.UNSPECIFIED.,.F.,.F.,(4,2,4),(-0.663826635786952,-0.332807172053596,
-1.00000002356548E-6),.UNSPECIFIED.);
#669=B_SPLINE_CURVE_WITH_KNOTS('',3,(#17838,#17839,#17840,#17841,#17842,
#17843),.UNSPECIFIED.,.F.,.F.,(4,2,4),(-0.662095257781154,-0.331862946603771,
0.),.UNSPECIFIED.);
#670=B_SPLINE_CURVE_WITH_KNOTS('',3,(#17845,#17846,#17847,#17848,#17849,
#17850),.UNSPECIFIED.,.F.,.F.,(4,2,4),(-0.662021613149805,-0.331771295733496,
-1.0000000176813E-6),.UNSPECIFIED.);
#671=B_SPLINE_CURVE_WITH_KNOTS('',3,(#17854,#17855,#17856,#17857,#17858,
#17859,#17860,#17861,#17862,#17863,#17864,#17865,#17866,#17867),
 .UNSPECIFIED.,.F.,.F.,(4,2,2,2,2,2,4),(-0.662550616898987,-0.621295480864932,
-0.580019388664009,-0.497408726506264,-0.331989034460189,-0.165834990380972,
-1.00000000990974E-6),.UNSPECIFIED.);
#672=B_SPLINE_CURVE_WITH_KNOTS('',3,(#17869,#17870,#17871,#17872,#17873,
#17874),.UNSPECIFIED.,.F.,.F.,(4,2,4),(-0.663826635786919,-0.332807172053578,
-1.00000002312139E-6),.UNSPECIFIED.);
#673=B_SPLINE_CURVE_WITH_KNOTS('',3,(#17879,#17880,#17881,#17882,#17883,
#17884),.UNSPECIFIED.,.F.,.F.,(4,2,4),(-0.662095257781154,-0.331862946603728,
0.),.UNSPECIFIED.);
#674=B_SPLINE_CURVE_WITH_KNOTS('',3,(#17886,#17887,#17888,#17889,#17890,
#17891),.UNSPECIFIED.,.F.,.F.,(4,2,4),(-0.662021613337153,-0.331771296170992,
-1.00000001779232E-6),.UNSPECIFIED.);
#675=B_SPLINE_CURVE_WITH_KNOTS('',3,(#17895,#17896,#17897,#17898,#17899,
#17900,#17901,#17902,#17903,#17904,#17905,#17906,#17907,#17908),
 .UNSPECIFIED.,.F.,.F.,(4,2,2,2,2,2,4),(-0.662550701757792,-0.621305253813084,
-0.580038858838667,-0.497447618998446,-0.332066833308196,-0.165873822514761,
-1.00000000857747E-6),.UNSPECIFIED.);
#676=B_SPLINE_CURVE_WITH_KNOTS('',3,(#17910,#17911,#17912,#17913,#17914,
#17915),.UNSPECIFIED.,.F.,.F.,(4,2,4),(-0.66382663578696,-0.332807172053593,
-1.00000002312139E-6),.UNSPECIFIED.);
#677=B_SPLINE_CURVE_WITH_KNOTS('',3,(#17920,#17921,#17922,#17923,#17924,
#17925),.UNSPECIFIED.,.F.,.F.,(4,2,4),(-0.662095257781059,-0.331862946603702,
0.),.UNSPECIFIED.);
#678=B_SPLINE_CURVE_WITH_KNOTS('',3,(#17927,#17928,#17929,#17930,#17931,
#17932),.UNSPECIFIED.,.F.,.F.,(4,2,4),(-0.662021613440326,-0.331771295866445,
-1.00000001779232E-6),.UNSPECIFIED.);
#679=B_SPLINE_CURVE_WITH_KNOTS('',3,(#17936,#17937,#17938,#17939,#17940,
#17941,#17942,#17943,#17944,#17945,#17946,#17947,#17948,#17949),
 .UNSPECIFIED.,.F.,.F.,(4,2,2,2,2,2,4),(-0.662550701758225,-0.621305253856284,
-0.580038858924235,-0.497447619168591,-0.332066833647734,-0.165873822684014,
-1.00000000935463E-6),.UNSPECIFIED.);
#680=B_SPLINE_CURVE_WITH_KNOTS('',3,(#17951,#17952,#17953,#17954,#17955,
#17956),.UNSPECIFIED.,.F.,.F.,(4,2,4),(-0.663826635787033,-0.332807172053606,
-1.00000002256628E-6),.UNSPECIFIED.);
#681=B_SPLINE_CURVE_WITH_KNOTS('',3,(#17961,#17962,#17963,#17964,#17965,
#17966),.UNSPECIFIED.,.F.,.F.,(4,2,4),(-0.662095257781069,-0.331862946603717,
0.),.UNSPECIFIED.);
#682=B_SPLINE_CURVE_WITH_KNOTS('',3,(#17968,#17969,#17970,#17971,#17972,
#17973),.UNSPECIFIED.,.F.,.F.,(4,2,4),(-0.662021613427598,-0.331771295860329,
-1.00000001779232E-6),.UNSPECIFIED.);
#683=B_SPLINE_CURVE_WITH_KNOTS('',3,(#17977,#17978,#17979,#17980,#17981,
#17982,#17983,#17984,#17985,#17986,#17987,#17988,#17989,#17990),
 .UNSPECIFIED.,.F.,.F.,(4,2,2,2,2,2,4),(-0.662550701754713,-0.621305253810719,
-0.580038858836423,-0.497447618996478,-0.332066833307539,-0.165873822514765,
-1.00000000891054E-6),.UNSPECIFIED.);
#684=B_SPLINE_CURVE_WITH_KNOTS('',3,(#17992,#17993,#17994,#17995,#17996,
#17997),.UNSPECIFIED.,.F.,.F.,(4,2,4),(-0.663826635786997,-0.332807172053604,
-1.00000002267731E-6),.UNSPECIFIED.);
#685=B_SPLINE_CURVE_WITH_KNOTS('',3,(#18002,#18003,#18004,#18005,#18006,
#18007),.UNSPECIFIED.,.F.,.F.,(4,2,4),(-0.662095257781134,-0.331862946603725,
0.),.UNSPECIFIED.);
#686=B_SPLINE_CURVE_WITH_KNOTS('',3,(#18009,#18010,#18011,#18012,#18013,
#18014),.UNSPECIFIED.,.F.,.F.,(4,2,4),(-0.662021613339374,-0.331771295819707,
-1.00000001779232E-6),.UNSPECIFIED.);
#687=B_SPLINE_CURVE_WITH_KNOTS('',3,(#18018,#18019,#18020,#18021,#18022,
#18023,#18024,#18025,#18026,#18027,#18028,#18029,#18030,#18031),
 .UNSPECIFIED.,.F.,.F.,(4,2,2,2,2,2,4),(-0.662550701759283,-0.62130525381475,
-0.580038858840059,-0.49744761899971,-0.332066833308656,-0.165873822514787,
-1.00000000924361E-6),.UNSPECIFIED.);
#688=B_SPLINE_CURVE_WITH_KNOTS('',3,(#18033,#18034,#18035,#18036,#18037,
#18038),.UNSPECIFIED.,.F.,.F.,(4,2,4),(-0.663826635787049,-0.332807172053624,
-1.00000002012379E-6),.UNSPECIFIED.);
#689=B_SPLINE_CURVE_WITH_KNOTS('',3,(#18043,#18044,#18045,#18046,#18047,
#18048),.UNSPECIFIED.,.F.,.F.,(4,2,4),(-0.662095257776738,-0.331862946601972,
0.),.UNSPECIFIED.);
#690=B_SPLINE_CURVE_WITH_KNOTS('',3,(#18050,#18051,#18052,#18053,#18054,
#18055),.UNSPECIFIED.,.F.,.F.,(4,2,4),(-0.662021613160614,-0.331771295738581,
-1.00000001823641E-6),.UNSPECIFIED.);
#691=B_SPLINE_CURVE_WITH_KNOTS('',3,(#18059,#18060,#18061,#18062,#18063,
#18064,#18065,#18066,#18067,#18068,#18069,#18070,#18071,#18072),
 .UNSPECIFIED.,.F.,.F.,(4,2,2,2,2,2,4),(-0.662550701758829,-0.621305253813552,
-0.580038858838592,-0.497447618998373,-0.332066833308538,-0.165873822514955,
-1.00000000724521E-6),.UNSPECIFIED.);
#692=B_SPLINE_CURVE_WITH_KNOTS('',3,(#18074,#18075,#18076,#18077,#18078,
#18079),.UNSPECIFIED.,.F.,.F.,(4,2,4),(-0.663826635786964,-0.332807172053598,
-1.00000002323242E-6),.UNSPECIFIED.);
#693=B_SPLINE_CURVE_WITH_KNOTS('',3,(#18084,#18085,#18086,#18087,#18088,
#18089),.UNSPECIFIED.,.F.,.F.,(4,2,4),(-0.662095257781233,-0.331862946603775,
0.),.UNSPECIFIED.);
#694=B_SPLINE_CURVE_WITH_KNOTS('',3,(#18091,#18092,#18093,#18094,#18095,
#18096),.UNSPECIFIED.,.F.,.F.,(4,2,4),(-0.662021612957221,-0.331771295645616,
-1.00000001779232E-6),.UNSPECIFIED.);
#695=B_SPLINE_CURVE_WITH_KNOTS('',3,(#18100,#18101,#18102,#18103,#18104,
#18105,#18106,#18107,#18108,#18109,#18110,#18111,#18112,#18113),
 .UNSPECIFIED.,.F.,.F.,(4,2,2,2,2,2,4),(-0.662550701757299,-0.621305253812781,
-0.580038858838426,-0.497447618998266,-0.332066833308142,-0.165873822514797,
-1.00000000835543E-6),.UNSPECIFIED.);
#696=B_SPLINE_CURVE_WITH_KNOTS('',3,(#18115,#18116,#18117,#18118,#18119,
#18120),.UNSPECIFIED.,.F.,.F.,(4,2,4),(-0.663826635786982,-0.332807172053603,
-1.00000002223322E-6),.UNSPECIFIED.);
#697=B_SPLINE_CURVE_WITH_KNOTS('',3,(#18125,#18126,#18127,#18128,#18129,
#18130),.UNSPECIFIED.,.F.,.F.,(4,2,4),(-0.662095257781211,-0.331862946603789,
0.),.UNSPECIFIED.);
#698=B_SPLINE_CURVE_WITH_KNOTS('',3,(#18132,#18133,#18134,#18135,#18136,
#18137),.UNSPECIFIED.,.F.,.F.,(4,2,4),(-0.662021612815302,-0.331771295581121,
-1.00000001779232E-6),.UNSPECIFIED.);
#699=B_SPLINE_CURVE_WITH_KNOTS('',3,(#18141,#18142,#18143,#18144,#18145,
#18146,#18147,#18148,#18149,#18150,#18151,#18152,#18153,#18154),
 .UNSPECIFIED.,.F.,.F.,(4,2,2,2,2,2,4),(-0.662550701758534,-0.621305253813699,
-0.580038858839343,-0.497447618999118,-0.33206683330838,-0.165873822514653,
-1.00000000935463E-6),.UNSPECIFIED.);
#700=B_SPLINE_CURVE_WITH_KNOTS('',3,(#18156,#18157,#18158,#18159,#18160,
#18161),.UNSPECIFIED.,.F.,.F.,(4,2,4),(-0.663826635786954,-0.332807172053568,
-1.00000001945766E-6),.UNSPECIFIED.);
#701=B_SPLINE_CURVE_WITH_KNOTS('',3,(#18166,#18167,#18168,#18169,#18170,
#18171),.UNSPECIFIED.,.F.,.F.,(4,2,4),(-0.662095257781192,-0.331862946603769,
0.),.UNSPECIFIED.);
#702=B_SPLINE_CURVE_WITH_KNOTS('',3,(#18173,#18174,#18175,#18176,#18177,
#18178),.UNSPECIFIED.,.F.,.F.,(4,2,4),(-0.662021612558326,-0.331771295463796,
-1.00000001779232E-6),.UNSPECIFIED.);
#703=B_SPLINE_CURVE_WITH_KNOTS('',3,(#18182,#18183,#18184,#18185,#18186,
#18187,#18188,#18189,#18190,#18191,#18192,#18193,#18194,#18195),
 .UNSPECIFIED.,.F.,.F.,(4,2,2,2,2,2,4),(-0.662550701759507,-0.621305253814335,
-0.580038858839854,-0.497447618999759,-0.332066833308242,-0.165873822514247,
-1.00000001002076E-6),.UNSPECIFIED.);
#704=B_SPLINE_CURVE_WITH_KNOTS('',3,(#18197,#18198,#18199,#18200,#18201,
#18202),.UNSPECIFIED.,.F.,.F.,(4,2,4),(-0.663826635787048,-0.332807172053641,
-1.00000002123402E-6),.UNSPECIFIED.);
#705=B_SPLINE_CURVE_WITH_KNOTS('',3,(#18207,#18208,#18209,#18210,#18211,
#18212),.UNSPECIFIED.,.F.,.F.,(4,2,4),(-0.662095257781137,-0.331862946603746,
0.),.UNSPECIFIED.);
#706=B_SPLINE_CURVE_WITH_KNOTS('',3,(#18214,#18215,#18216,#18217,#18218,
#18219),.UNSPECIFIED.,.F.,.F.,(4,2,4),(-0.662021612804876,-0.331771295576207,
-1.0000000176813E-6),.UNSPECIFIED.);
#707=B_SPLINE_CURVE_WITH_KNOTS('',3,(#18223,#18224,#18225,#18226,#18227,
#18228,#18229,#18230,#18231,#18232,#18233,#18234,#18235,#18236),
 .UNSPECIFIED.,.F.,.F.,(4,2,2,2,2,2,4),(-0.662550701759088,-0.621305253814185,
-0.580038858840118,-0.497447619000064,-0.332066833308297,-0.165873822514322,
-1.000000006246E-6),.UNSPECIFIED.);
#708=B_SPLINE_CURVE_WITH_KNOTS('',3,(#18238,#18239,#18240,#18241,#18242,
#18243),.UNSPECIFIED.,.F.,.F.,(4,2,4),(-0.663826635786971,-0.332807172053609,
-1.00000002334344E-6),.UNSPECIFIED.);
#709=B_SPLINE_CURVE_WITH_KNOTS('',3,(#18248,#18249,#18250,#18251,#18252,
#18253),.UNSPECIFIED.,.F.,.F.,(4,2,4),(-0.662095257781061,-0.331862946603719,
0.),.UNSPECIFIED.);
#710=B_SPLINE_CURVE_WITH_KNOTS('',3,(#18255,#18256,#18257,#18258,#18259,
#18260),.UNSPECIFIED.,.F.,.F.,(4,2,4),(-0.662021612957974,-0.33177129564596,
-1.00000001779232E-6),.UNSPECIFIED.);
#711=B_SPLINE_CURVE_WITH_KNOTS('',3,(#18264,#18265,#18266,#18267,#18268,
#18269,#18270,#18271,#18272,#18273,#18274,#18275,#18276,#18277),
 .UNSPECIFIED.,.F.,.F.,(4,2,2,2,2,2,4),(-0.66255070175906,-0.621305253814359,
-0.580038858840127,-0.49744761899987,-0.332066833308326,-0.165873822514433,
-1.0000000086885E-6),.UNSPECIFIED.);
#712=B_SPLINE_CURVE_WITH_KNOTS('',3,(#18279,#18280,#18281,#18282,#18283,
#18284),.UNSPECIFIED.,.F.,.F.,(4,2,4),(-0.663826635786987,-0.332807172053615,
-1.00000002101197E-6),.UNSPECIFIED.);
#713=B_SPLINE_CURVE_WITH_KNOTS('',3,(#18289,#18290,#18291,#18292,#18293,
#18294),.UNSPECIFIED.,.F.,.F.,(4,2,4),(-0.662095257781128,-0.331862946603748,
0.),.UNSPECIFIED.);
#714=B_SPLINE_CURVE_WITH_KNOTS('',3,(#18296,#18297,#18298,#18299,#18300,
#18301,#18302,#18303,#18304,#18305,#18306,#18307),.UNSPECIFIED.,.F.,.F.,
(4,2,2,2,2,4),(-0.660887065044359,-0.330927753205643,-0.165242782459234,
-0.0825626423163793,-0.0412727318856715,-9.99999991702083E-7),
 .UNSPECIFIED.);
#715=B_SPLINE_CURVE_WITH_KNOTS('',3,(#18311,#18312,#18313,#18314,#18315,
#18316,#18317,#18318,#18319,#18320,#18321,#18322,#18323,#18324),
 .UNSPECIFIED.,.F.,.F.,(4,2,2,2,2,2,4),(-0.662550701758423,-0.621305253813834,
-0.580038858839635,-0.49744761899939,-0.332066833308269,-0.165873822514469,
-1.00000000746725E-6),.UNSPECIFIED.);
#716=B_SPLINE_CURVE_WITH_KNOTS('',3,(#18326,#18327,#18328,#18329,#18330,
#18331),.UNSPECIFIED.,.F.,.F.,(4,2,4),(-0.663826635787052,-0.332807172053646,
-1.00000002023481E-6),.UNSPECIFIED.);
#717=B_SPLINE_CURVE_WITH_KNOTS('',3,(#18336,#18337,#18338,#18339,#18340,
#18341),.UNSPECIFIED.,.F.,.F.,(4,2,4),(-0.662095257781141,-0.331862946603758,
0.),.UNSPECIFIED.);
#718=B_SPLINE_CURVE_WITH_KNOTS('',3,(#18343,#18344,#18345,#18346,#18347,
#18348,#18349,#18350,#18351,#18352,#18353,#18354),.UNSPECIFIED.,.F.,.F.,
(4,2,2,2,2,4),(-0.660887065033929,-0.330927753200197,-0.165242782456535,
-0.0825626423149307,-0.0412727318851053,-9.99999991591061E-7),
 .UNSPECIFIED.);
#719=B_SPLINE_CURVE_WITH_KNOTS('',3,(#18358,#18359,#18360,#18361,#18362,
#18363,#18364,#18365),.UNSPECIFIED.,.F.,.F.,(4,2,2,4),(-0.663084973284213,
-0.332066834082123,-0.165873822900741,-1.00000000902156E-6),
 .UNSPECIFIED.);
#720=B_SPLINE_CURVE_WITH_KNOTS('',3,(#18367,#18368,#18369,#18370,#18371,
#18372),.UNSPECIFIED.,.F.,.F.,(4,2,4),(-0.663826635787002,-0.332807172053626,
-1.0000000206789E-6),.UNSPECIFIED.);
#721=B_SPLINE_CURVE_WITH_KNOTS('',3,(#18377,#18378,#18379,#18380,#18381,
#18382),.UNSPECIFIED.,.F.,.F.,(4,2,4),(-0.662095257781032,-0.331862946603718,
0.),.UNSPECIFIED.);
#722=B_SPLINE_CURVE_WITH_KNOTS('',3,(#18384,#18385,#18386,#18387,#18388,
#18389),.UNSPECIFIED.,.F.,.F.,(4,2,4),(-0.662021613431922,-0.331771295862448,
-1.00000001779232E-6),.UNSPECIFIED.);
#723=B_SPLINE_CURVE_WITH_KNOTS('',3,(#18393,#18394,#18395,#18396,#18397,
#18398,#18399,#18400),.UNSPECIFIED.,.F.,.F.,(4,2,2,4),(-0.663084973280964,
-0.332066834082069,-0.165873822901686,-1.00000000935463E-6),
 .UNSPECIFIED.);
#724=B_SPLINE_CURVE_WITH_KNOTS('',3,(#18402,#18403,#18404,#18405,#18406,
#18407),.UNSPECIFIED.,.F.,.F.,(4,2,4),(-0.663826635787037,-0.33280717205365,
-1.00000002334344E-6),.UNSPECIFIED.);
#725=B_SPLINE_CURVE_WITH_KNOTS('',3,(#18412,#18413,#18414,#18415,#18416,
#18417),.UNSPECIFIED.,.F.,.F.,(4,2,4),(-0.662095257781131,-0.331862946603741,
0.),.UNSPECIFIED.);
#726=B_SPLINE_CURVE_WITH_KNOTS('',3,(#18419,#18420,#18421,#18422,#18423,
#18424),.UNSPECIFIED.,.F.,.F.,(4,2,4),(-0.662021613430381,-0.331771295861564,
-1.00000001779232E-6),.UNSPECIFIED.);
#727=B_SPLINE_CURVE_WITH_KNOTS('',3,(#18428,#18429,#18430,#18431,#18432,
#18433,#18434,#18435,#18436,#18437,#18438,#18439,#18440,#18441),
 .UNSPECIFIED.,.F.,.F.,(4,2,2,2,2,2,4),(-0.662550701756468,-0.62130525381211,
-0.580038858837624,-0.497447618997602,-0.332066833307905,-0.165873822514476,
-1.00000000846645E-6),.UNSPECIFIED.);
#728=B_SPLINE_CURVE_WITH_KNOTS('',3,(#18443,#18444,#18445,#18446,#18447,
#18448),.UNSPECIFIED.,.F.,.F.,(4,2,4),(-0.663826635787072,-0.332807172053659,
-1.00000002223322E-6),.UNSPECIFIED.);
#729=B_SPLINE_CURVE_WITH_KNOTS('',3,(#18453,#18454,#18455,#18456,#18457,
#18458),.UNSPECIFIED.,.F.,.F.,(4,2,4),(-0.662095257781099,-0.331862946603744,
0.),.UNSPECIFIED.);
#730=B_SPLINE_CURVE_WITH_KNOTS('',3,(#18460,#18461,#18462,#18463,#18464,
#18465),.UNSPECIFIED.,.F.,.F.,(4,2,4),(-0.662021613329726,-0.331771295815806,
-1.00000001779232E-6),.UNSPECIFIED.);
#731=B_SPLINE_CURVE_WITH_KNOTS('',3,(#18469,#18470,#18471,#18472,#18473,
#18474,#18475,#18476,#18477,#18478,#18479,#18480,#18481,#18482),
 .UNSPECIFIED.,.F.,.F.,(4,2,2,2,2,2,4),(-0.662550701757085,-0.621305253812491,
-0.580038858837846,-0.497447618997816,-0.332066833308107,-0.165873822514721,
-1.00000000857747E-6),.UNSPECIFIED.);
#732=B_SPLINE_CURVE_WITH_KNOTS('',3,(#18484,#18485,#18486,#18487,#18488,
#18489),.UNSPECIFIED.,.F.,.F.,(4,2,4),(-0.663826635787016,-0.332807172053633,
-1.00000002301037E-6),.UNSPECIFIED.);
#733=B_SPLINE_CURVE_WITH_KNOTS('',3,(#18494,#18495,#18496,#18497,#18498,
#18499),.UNSPECIFIED.,.F.,.F.,(4,2,4),(-0.662095257776784,-0.331862946602006,
0.),.UNSPECIFIED.);
#734=B_SPLINE_CURVE_WITH_KNOTS('',3,(#18501,#18502,#18503,#18504,#18505,
#18506),.UNSPECIFIED.,.F.,.F.,(4,2,4),(-0.662021613154439,-0.331771295735777,
-1.00000001712619E-6),.UNSPECIFIED.);
#735=B_SPLINE_CURVE_WITH_KNOTS('',3,(#18510,#18511,#18512,#18513,#18514,
#18515,#18516,#18517,#18518,#18519,#18520,#18521,#18522,#18523),
 .UNSPECIFIED.,.F.,.F.,(4,2,2,2,2,2,4),(-0.662550701757146,-0.621305253812992,
-0.580038858838693,-0.497447618998531,-0.332066833308134,-0.165873822514585,
-1.00000000902156E-6),.UNSPECIFIED.);
#736=B_SPLINE_CURVE_WITH_KNOTS('',3,(#18525,#18526,#18527,#18528,#18529,
#18530),.UNSPECIFIED.,.F.,.F.,(4,2,4),(-0.663826635786971,-0.332807172053601,
-1.00000002234424E-6),.UNSPECIFIED.);
#737=B_SPLINE_CURVE_WITH_KNOTS('',3,(#18535,#18536,#18537,#18538,#18539,
#18540),.UNSPECIFIED.,.F.,.F.,(4,2,4),(-0.662095257781007,-0.331862946603684,
0.),.UNSPECIFIED.);
#738=B_SPLINE_CURVE_WITH_KNOTS('',3,(#18542,#18543,#18544,#18545,#18546,
#18547),.UNSPECIFIED.,.F.,.F.,(4,2,4),(-0.662021612957012,-0.331771295645723,
-1.00000001779232E-6),.UNSPECIFIED.);
#739=B_SPLINE_CURVE_WITH_KNOTS('',3,(#18551,#18552,#18553,#18554,#18555,
#18556,#18557,#18558,#18559,#18560,#18561,#18562,#18563,#18564),
 .UNSPECIFIED.,.F.,.F.,(4,2,2,2,2,2,4),(-0.66255070175672,-0.621305253812282,
-0.58003885883802,-0.497447618998075,-0.332066833307935,-0.165873822514331,
-1.00000000913258E-6),.UNSPECIFIED.);
#740=B_SPLINE_CURVE_WITH_KNOTS('',3,(#18566,#18567,#18568,#18569,#18570,
#18571),.UNSPECIFIED.,.F.,.F.,(4,2,4),(-0.663826635786866,-0.332807172053519,
-1.00000002145606E-6),.UNSPECIFIED.);
#741=B_SPLINE_CURVE_WITH_KNOTS('',3,(#18576,#18577,#18578,#18579,#18580,
#18581),.UNSPECIFIED.,.F.,.F.,(4,2,4),(-0.662095306120118,-0.331830781965298,
0.),.UNSPECIFIED.);
#742=B_SPLINE_CURVE_WITH_KNOTS('',3,(#18583,#18584,#18585,#18586,#18587,
#18588),.UNSPECIFIED.,.F.,.F.,(4,2,4),(-0.662021612806063,-0.331771295576848,
-1.00000001779232E-6),.UNSPECIFIED.);
#743=B_SPLINE_CURVE_WITH_KNOTS('',3,(#18592,#18593,#18594,#18595,#18596,
#18597,#18598,#18599,#18600,#18601,#18602,#18603,#18604,#18605),
 .UNSPECIFIED.,.F.,.F.,(4,2,2,2,2,2,4),(-0.662550701758247,-0.621305253813676,
-0.580038858839485,-0.497447618999181,-0.332066833308307,-0.165873822514554,
-1.00000000902156E-6),.UNSPECIFIED.);
#744=B_SPLINE_CURVE_WITH_KNOTS('',3,(#18607,#18608,#18609,#18610,#18611,
#18612),.UNSPECIFIED.,.F.,.F.,(4,2,4),(-0.663826635786942,-0.332807172053572,
-1.00000002056788E-6),.UNSPECIFIED.);
#745=B_SPLINE_CURVE_WITH_KNOTS('',3,(#18617,#18618,#18619,#18620,#18621,
#18622),.UNSPECIFIED.,.F.,.F.,(4,2,4),(-0.66209530612013,-0.331830781965309,
0.),.UNSPECIFIED.);
#746=B_SPLINE_CURVE_WITH_KNOTS('',3,(#18624,#18625,#18626,#18627,#18628,
#18629,#18630,#18631,#18632,#18633,#18634,#18635),.UNSPECIFIED.,.F.,.F.,
(4,2,2,2,2,4),(-0.66088706502341,-0.330927753195277,-0.165242782452955,
-0.0825626423128806,-0.0412727318841083,-9.99999991702083E-7),
 .UNSPECIFIED.);
#747=B_SPLINE_CURVE_WITH_KNOTS('',3,(#18639,#18640,#18641,#18642,#18643,
#18644,#18645,#18646,#18647,#18648,#18649,#18650,#18651,#18652),
 .UNSPECIFIED.,.F.,.F.,(4,2,2,2,2,2,4),(-0.662550701758955,-0.621305253813872,
-0.580038858839428,-0.497447618999422,-0.332066833308222,-0.165873822514119,
-1.00000001013179E-6),.UNSPECIFIED.);
#748=B_SPLINE_CURVE_WITH_KNOTS('',3,(#18654,#18655,#18656,#18657,#18658,
#18659),.UNSPECIFIED.,.F.,.F.,(4,2,4),(-0.66382655429936,-0.332732370051042,
-1.00000002123402E-6),.UNSPECIFIED.);
#749=B_SPLINE_CURVE_WITH_KNOTS('',3,(#18664,#18665,#18666,#18667,#18668,
#18669),.UNSPECIFIED.,.F.,.F.,(4,2,4),(-0.662095306120191,-0.33183078196534,
0.),.UNSPECIFIED.);
#750=B_SPLINE_CURVE_WITH_KNOTS('',3,(#18671,#18672,#18673,#18674,#18675,
#18676,#18677,#18678,#18679,#18680,#18681,#18682),.UNSPECIFIED.,.F.,.F.,
(4,2,2,2,2,4),(-0.66088706502611,-0.330927753196476,-0.165242782453738,
-0.0825626423132116,-0.0412727318842448,-9.99999991702083E-7),
 .UNSPECIFIED.);
#751=B_SPLINE_CURVE_WITH_KNOTS('',3,(#18686,#18687,#18688,#18689,#18690,
#18691,#18692,#18693),.UNSPECIFIED.,.F.,.F.,(4,2,2,4),(-0.663084973282026,
-0.332066834082184,-0.165873822900691,-1.00000000946565E-6),
 .UNSPECIFIED.);
#752=B_SPLINE_CURVE_WITH_KNOTS('',3,(#18695,#18696,#18697,#18698,#18699,
#18700),.UNSPECIFIED.,.F.,.F.,(4,2,4),(-0.663826554299285,-0.332732370051009,
-1.0000000216781E-6),.UNSPECIFIED.);
#753=B_SPLINE_CURVE_WITH_KNOTS('',3,(#18705,#18706,#18707,#18708,#18709,
#18710),.UNSPECIFIED.,.F.,.F.,(4,2,4),(-0.662095306120128,-0.331830781965308,
0.),.UNSPECIFIED.);
#754=B_SPLINE_CURVE_WITH_KNOTS('',3,(#18712,#18713,#18714,#18715,#18716,
#18717),.UNSPECIFIED.,.F.,.F.,(4,2,4),(-0.662021612958496,-0.331771295646342,
-1.00000001779232E-6),.UNSPECIFIED.);
#755=B_SPLINE_CURVE_WITH_KNOTS('',3,(#18721,#18722,#18723,#18724,#18725,
#18726,#18727,#18728),.UNSPECIFIED.,.F.,.F.,(4,2,2,4),(-0.663084973281183,
-0.332066834082057,-0.165873822900902,-1.00000000935463E-6),
 .UNSPECIFIED.);
#756=B_SPLINE_CURVE_WITH_KNOTS('',3,(#18730,#18731,#18732,#18733,#18734,
#18735),.UNSPECIFIED.,.F.,.F.,(4,2,4),(-0.663826554299325,-0.332732370051047,
-1.00000002256628E-6),.UNSPECIFIED.);
#757=B_SPLINE_CURVE_WITH_KNOTS('',3,(#18740,#18741,#18742,#18743,#18744,
#18745),.UNSPECIFIED.,.F.,.F.,(4,2,4),(-0.662095306120064,-0.331830781965281,
0.),.UNSPECIFIED.);
#758=B_SPLINE_CURVE_WITH_KNOTS('',3,(#18747,#18748,#18749,#18750,#18751,
#18752),.UNSPECIFIED.,.F.,.F.,(4,2,4),(-0.662021613146791,-0.331771295731921,
-1.00000001679312E-6),.UNSPECIFIED.);
#759=B_SPLINE_CURVE_WITH_KNOTS('',3,(#18756,#18757,#18758,#18759,#18760,
#18761,#18762,#18763,#18764,#18765,#18766,#18767,#18768,#18769),
 .UNSPECIFIED.,.F.,.F.,(4,2,2,2,2,2,4),(-0.662550701759488,-0.621305253814721,
-0.580038858840412,-0.497447619000151,-0.332066833308525,-0.165873822514555,
-1.00000000902156E-6),.UNSPECIFIED.);
#760=B_SPLINE_CURVE_WITH_KNOTS('',3,(#18771,#18772,#18773,#18774,#18775,
#18776),.UNSPECIFIED.,.F.,.F.,(4,2,4),(-0.663826554299435,-0.332732370051088,
-1.00000001990175E-6),.UNSPECIFIED.);
#761=B_SPLINE_CURVE_WITH_KNOTS('',3,(#18781,#18782,#18783,#18784,#18785,
#18786),.UNSPECIFIED.,.F.,.F.,(4,2,4),(-0.662095306120062,-0.331830781965283,
0.),.UNSPECIFIED.);
#762=B_SPLINE_CURVE_WITH_KNOTS('',3,(#18788,#18789,#18790,#18791,#18792,
#18793),.UNSPECIFIED.,.F.,.F.,(4,2,4),(-0.662021613347664,-0.331771296175878,
-1.00000001779232E-6),.UNSPECIFIED.);
#763=B_SPLINE_CURVE_WITH_KNOTS('',3,(#18797,#18798,#18799,#18800,#18801,
#18802,#18803,#18804,#18805,#18806,#18807,#18808,#18809,#18810),
 .UNSPECIFIED.,.F.,.F.,(4,2,2,2,2,2,4),(-0.662550701760095,-0.621305253815354,
-0.580038858840818,-0.497447619000533,-0.332066833308807,-0.165873822514148,
-1.00000001002076E-6),.UNSPECIFIED.);
#764=B_SPLINE_CURVE_WITH_KNOTS('',3,(#18812,#18813,#18814,#18815,#18816,
#18817),.UNSPECIFIED.,.F.,.F.,(4,2,4),(-0.663826554299384,-0.332732370051052,
-1.00000002145606E-6),.UNSPECIFIED.);
#765=B_SPLINE_CURVE_WITH_KNOTS('',3,(#18822,#18823,#18824,#18825,#18826,
#18827),.UNSPECIFIED.,.F.,.F.,(4,2,4),(-0.662095306120294,-0.33183078196538,
0.),.UNSPECIFIED.);
#766=B_SPLINE_CURVE_WITH_KNOTS('',3,(#18829,#18830,#18831,#18832,#18833,
#18834),.UNSPECIFIED.,.F.,.F.,(4,2,4),(-0.662021613433192,-0.331771295862689,
-1.00000001779232E-6),.UNSPECIFIED.);
#767=B_SPLINE_CURVE_WITH_KNOTS('',3,(#18838,#18839,#18840,#18841,#18842,
#18843,#18844,#18845,#18846,#18847,#18848,#18849,#18850,#18851),
 .UNSPECIFIED.,.F.,.F.,(4,2,2,2,2,2,4),(-0.662550701758329,-0.621305253855782,
-0.580038858923311,-0.497447619167824,-0.332066833647579,-0.1658738226846,
-1.00000000935463E-6),.UNSPECIFIED.);
#768=B_SPLINE_CURVE_WITH_KNOTS('',3,(#18853,#18854,#18855,#18856,#18857,
#18858),.UNSPECIFIED.,.F.,.F.,(4,2,4),(-0.663826554299397,-0.33273237005105,
-1.00000002078993E-6),.UNSPECIFIED.);
#769=B_SPLINE_CURVE_WITH_KNOTS('',3,(#18863,#18864,#18865,#18866,#18867,
#18868),.UNSPECIFIED.,.F.,.F.,(4,2,4),(-0.662095306120216,-0.331830781965384,
0.),.UNSPECIFIED.);
#770=B_SPLINE_CURVE_WITH_KNOTS('',3,(#18870,#18871,#18872,#18873,#18874,
#18875),.UNSPECIFIED.,.F.,.F.,(4,2,4),(-0.662021613436443,-0.3317712958642,
-1.0000000176813E-6),.UNSPECIFIED.);
#771=B_SPLINE_CURVE_WITH_KNOTS('',3,(#18879,#18880,#18881,#18882,#18883,
#18884,#18885,#18886,#18887,#18888,#18889,#18890,#18891,#18892),
 .UNSPECIFIED.,.F.,.F.,(4,2,2,2,2,2,4),(-0.662550701759013,-0.621305253814237,
-0.580038858839444,-0.497447618999241,-0.332066833308602,-0.165873822514864,
-1.00000000702316E-6),.UNSPECIFIED.);
#772=B_SPLINE_CURVE_WITH_KNOTS('',3,(#18894,#18895,#18896,#18897,#18898,
#18899),.UNSPECIFIED.,.F.,.F.,(4,2,4),(-0.663826554299459,-0.3327323700511,
-1.00000002112299E-6),.UNSPECIFIED.);
#773=B_SPLINE_CURVE_WITH_KNOTS('',3,(#18904,#18905,#18906,#18907,#18908,
#18909),.UNSPECIFIED.,.F.,.F.,(4,2,4),(-0.662095306120087,-0.331830781965296,
0.),.UNSPECIFIED.);
#774=B_SPLINE_CURVE_WITH_KNOTS('',3,(#18911,#18912,#18913,#18914,#18915,
#18916),.UNSPECIFIED.,.F.,.F.,(4,2,4),(-0.662021613343284,-0.33177129582197,
-1.00000001790335E-6),.UNSPECIFIED.);
#775=B_SPLINE_CURVE_WITH_KNOTS('',3,(#18920,#18921,#18922,#18923,#18924,
#18925,#18926,#18927,#18928,#18929,#18930,#18931,#18932,#18933),
 .UNSPECIFIED.,.F.,.F.,(4,2,2,2,2,2,4),(-0.662550701758145,-0.621305253812989,
-0.580038858838031,-0.497447618997672,-0.33206683330843,-0.165873822514873,
-1.0000000086885E-6),.UNSPECIFIED.);
#776=B_SPLINE_CURVE_WITH_KNOTS('',3,(#18935,#18936,#18937,#18938,#18939,
#18940),.UNSPECIFIED.,.F.,.F.,(4,2,4),(-0.663826554299388,-0.332732370051057,
-1.00000002101197E-6),.UNSPECIFIED.);
#777=B_SPLINE_CURVE_WITH_KNOTS('',3,(#18945,#18946,#18947,#18948,#18949,
#18950),.UNSPECIFIED.,.F.,.F.,(4,2,4),(-0.662095306120114,-0.331830781965322,
0.),.UNSPECIFIED.);
#778=B_SPLINE_CURVE_WITH_KNOTS('',3,(#18952,#18953,#18954,#18955,#18956,
#18957),.UNSPECIFIED.,.F.,.F.,(4,2,4),(-0.662021613164074,-0.331771295740365,
-1.00000001790335E-6),.UNSPECIFIED.);
#779=B_SPLINE_CURVE_WITH_KNOTS('',3,(#18961,#18962,#18963,#18964,#18965,
#18966,#18967,#18968,#18969,#18970,#18971,#18972,#18973,#18974),
 .UNSPECIFIED.,.F.,.F.,(4,2,2,2,2,2,4),(-0.662550701755705,-0.62130525381069,
-0.580038858835955,-0.497447618995727,-0.332066833307856,-0.165873822515044,
-1.00000000857747E-6),.UNSPECIFIED.);
#780=B_SPLINE_CURVE_WITH_KNOTS('',3,(#18976,#18977,#18978,#18979,#18980,
#18981),.UNSPECIFIED.,.F.,.F.,(4,2,4),(-0.663826554299419,-0.332732370051075,
-1.00000002234424E-6),.UNSPECIFIED.);
#781=B_SPLINE_CURVE_WITH_KNOTS('',3,(#18986,#18987,#18988,#18989,#18990,
#18991),.UNSPECIFIED.,.F.,.F.,(4,2,4),(-0.662095306120204,-0.331830781965362,
0.),.UNSPECIFIED.);
#782=B_SPLINE_CURVE_WITH_KNOTS('',3,(#18993,#18994,#18995,#18996,#18997,
#18998),.UNSPECIFIED.,.F.,.F.,(4,2,4),(-0.662021612967814,-0.33177129565058,
-1.00000001779232E-6),.UNSPECIFIED.);
#783=B_SPLINE_CURVE_WITH_KNOTS('',3,(#19002,#19003,#19004,#19005,#19006,
#19007,#19008,#19009,#19010,#19011,#19012,#19013,#19014,#19015),
 .UNSPECIFIED.,.F.,.F.,(4,2,2,2,2,2,4),(-0.662550701757928,-0.621305253812802,
-0.58003885883804,-0.497447618997713,-0.332066833308205,-0.165873822515039,
-1.00000000768929E-6),.UNSPECIFIED.);
#784=B_SPLINE_CURVE_WITH_KNOTS('',3,(#19017,#19018,#19019,#19020,#19021,
#19022),.UNSPECIFIED.,.F.,.F.,(4,2,4),(-0.663826554299339,-0.332732370051032,
-1.00000002134504E-6),.UNSPECIFIED.);
#785=B_SPLINE_CURVE_WITH_KNOTS('',3,(#19027,#19028,#19029,#19030,#19031,
#19032),.UNSPECIFIED.,.F.,.F.,(4,2,4),(-0.662095257781194,-0.331862946603777,
0.),.UNSPECIFIED.);
#786=B_SPLINE_CURVE_WITH_KNOTS('',3,(#19034,#19035,#19036,#19037,#19038,
#19039),.UNSPECIFIED.,.F.,.F.,(4,2,4),(-0.662021612558349,-0.331771295463814,
-1.00000001779232E-6),.UNSPECIFIED.);
#787=B_SPLINE_CURVE_WITH_KNOTS('',3,(#19043,#19044,#19045,#19046,#19047,
#19048,#19049,#19050),.UNSPECIFIED.,.F.,.F.,(4,2,2,4),(-0.663084973281713,
-0.332066834082423,-0.165873822900929,-1.00000000924361E-6),
 .UNSPECIFIED.);
#788=B_SPLINE_CURVE_WITH_KNOTS('',3,(#19052,#19053,#19054,#19055,#19056,
#19057),.UNSPECIFIED.,.F.,.F.,(4,2,4),(-0.663826554299392,-0.332732370051039,
-1.00000002034584E-6),.UNSPECIFIED.);
#789=B_SPLINE_CURVE_WITH_KNOTS('',3,(#19062,#19063,#19064,#19065,#19066,
#19067),.UNSPECIFIED.,.F.,.F.,(4,2,4),(-0.662095306115713,-0.331830781963555,
0.),.UNSPECIFIED.);
#790=B_SPLINE_CURVE_WITH_KNOTS('',3,(#19069,#19070,#19071,#19072,#19073,
#19074,#19075,#19076,#19077,#19078,#19079,#19080),.UNSPECIFIED.,.F.,.F.,
(4,2,2,2,2,4),(-0.660887065032632,-0.330927753199737,-0.165242782455574,
-0.0825626423141882,-0.0412727318846662,-9.99999991702083E-7),
 .UNSPECIFIED.);
#791=B_SPLINE_CURVE_WITH_KNOTS('',3,(#19084,#19085,#19086,#19087,#19088,
#19089,#19090,#19091,#19092,#19093,#19094,#19095,#19096,#19097),
 .UNSPECIFIED.,.F.,.F.,(4,2,2,2,2,2,4),(-0.662550701759551,-0.621305253814749,
-0.58003885884035,-0.497447619000075,-0.332066833308522,-0.1658738225146,
-1.00000000924361E-6),.UNSPECIFIED.);
#792=B_SPLINE_CURVE_WITH_KNOTS('',3,(#19099,#19100,#19101,#19102,#19103,
#19104),.UNSPECIFIED.,.F.,.F.,(4,2,4),(-0.663826554299404,-0.332732370051068,
-1.00000002223322E-6),.UNSPECIFIED.);
#793=B_SPLINE_CURVE_WITH_KNOTS('',3,(#19109,#19110,#19111,#19112,#19113,
#19114,#19115,#19116,#19117,#19118,#19119,#19120),.UNSPECIFIED.,.F.,.F.,
(4,2,2,2,2,4),(-0.260520203475784,-0.209083280006074,-0.154198547441575,
-0.0839662032252584,-0.0407463936727428,0.),.UNSPECIFIED.);
#794=B_SPLINE_CURVE_WITH_KNOTS('',3,(#19122,#19123,#19124,#19125,#19126,
#19127,#19128),.UNSPECIFIED.,.F.,.F.,(4,3,4),(0.,0.000879527967505091,0.00156997524832468),
 .UNSPECIFIED.);
#795=B_SPLINE_CURVE_WITH_KNOTS('',3,(#19132,#19133,#19134,#19135,#19136,
#19137,#19138),.UNSPECIFIED.,.F.,.F.,(4,3,4),(9.85133562538035E-18,0.000871555184780974,
0.00160565474757454),.UNSPECIFIED.);
#796=B_SPLINE_CURVE_WITH_KNOTS('',3,(#19140,#19141,#19142,#19143,#19144,
#19145,#19146,#19147,#19148,#19149),.UNSPECIFIED.,.F.,.F.,(4,2,2,2,4),(-0.260724731519921,
-0.199727802453949,-0.13039083565756,-0.0610645770444107,0.),
 .UNSPECIFIED.);
#797=B_SPLINE_CURVE_WITH_KNOTS('',3,(#19151,#19152,#19153,#19154,#19155,
#19156,#19157),.UNSPECIFIED.,.F.,.F.,(4,3,4),(0.,0.000879527967506278,0.00156997524832335),
 .UNSPECIFIED.);
#798=B_SPLINE_CURVE_WITH_KNOTS('',3,(#19161,#19162,#19163,#19164,#19165,
#19166,#19167),.UNSPECIFIED.,.F.,.F.,(4,3,4),(2.22159771539451E-16,0.000871555185133579,
0.0016056547475732),.UNSPECIFIED.);
#799=B_SPLINE_CURVE_WITH_KNOTS('',3,(#19169,#19170,#19171,#19172,#19173,
#19174,#19175,#19176,#19177,#19178),.UNSPECIFIED.,.F.,.F.,(4,2,2,2,4),(-0.260724731516474,
-0.199727802451461,-0.130390835656149,-0.0610645770440664,0.),
 .UNSPECIFIED.);
#800=B_SPLINE_CURVE_WITH_KNOTS('',3,(#19180,#19181,#19182,#19183,#19184,
#19185,#19186),.UNSPECIFIED.,.F.,.F.,(4,3,4),(0.,0.000879527967497252,0.00156997524832199),
 .UNSPECIFIED.);
#801=B_SPLINE_CURVE_WITH_KNOTS('',3,(#19190,#19191,#19192,#19193,#19194,
#19195,#19196),.UNSPECIFIED.,.F.,.F.,(4,3,4),(3.46944695195361E-18,0.000871555184780109,
0.00160565474757182),.UNSPECIFIED.);
#802=B_SPLINE_CURVE_WITH_KNOTS('',3,(#19198,#19199,#19200,#19201,#19202,
#19203,#19204,#19205,#19206,#19207),.UNSPECIFIED.,.F.,.F.,(4,2,2,2,4),(-0.260724731519922,
-0.199727802453945,-0.130390835657557,-0.0610645770444094,0.),
 .UNSPECIFIED.);
#803=B_SPLINE_CURVE_WITH_KNOTS('',3,(#19209,#19210,#19211,#19212,#19213,
#19214,#19215),.UNSPECIFIED.,.F.,.F.,(4,3,4),(0.,0.000879527967508083,0.00156997524832066),
 .UNSPECIFIED.);
#804=B_SPLINE_CURVE_WITH_KNOTS('',3,(#19219,#19220,#19221,#19222,#19223,
#19224,#19225),.UNSPECIFIED.,.F.,.F.,(4,3,4),(9.34177181294034E-18,0.000871555184785609,
0.00160565474757049),.UNSPECIFIED.);
#805=B_SPLINE_CURVE_WITH_KNOTS('',3,(#19227,#19228,#19229,#19230,#19231,
#19232,#19233,#19234,#19235,#19236),.UNSPECIFIED.,.F.,.F.,(4,2,2,2,4),(-0.260724731519973,
-0.199727802453985,-0.130390835657586,-0.0610645770444184,0.),
 .UNSPECIFIED.);
#806=B_SPLINE_CURVE_WITH_KNOTS('',3,(#19238,#19239,#19240,#19241,#19242,
#19243,#19244),.UNSPECIFIED.,.F.,.F.,(4,3,4),(0.,0.000879527967501964,0.00156997524831932),
 .UNSPECIFIED.);
#807=B_SPLINE_CURVE_WITH_KNOTS('',3,(#19248,#19249,#19250,#19251,#19252,
#19253,#19254),.UNSPECIFIED.,.F.,.F.,(4,3,4),(1.73472347597681E-18,0.00087155518477886,
0.00160565474756914),.UNSPECIFIED.);
#808=B_SPLINE_CURVE_WITH_KNOTS('',3,(#19256,#19257,#19258,#19259,#19260,
#19261,#19262,#19263,#19264,#19265),.UNSPECIFIED.,.F.,.F.,(4,2,2,2,4),(-0.260724731519937,
-0.199727802453964,-0.130390835657569,-0.0610645770444118,0.),
 .UNSPECIFIED.);
#809=B_SPLINE_CURVE_WITH_KNOTS('',3,(#19267,#19268,#19269,#19270,#19271,
#19272,#19273),.UNSPECIFIED.,.F.,.F.,(4,3,4),(0.,0.000879527967645649,0.00156997524831794),
 .UNSPECIFIED.);
#810=B_SPLINE_CURVE_WITH_KNOTS('',3,(#19277,#19278,#19279,#19280,#19281,
#19282,#19283),.UNSPECIFIED.,.F.,.F.,(4,3,4),(2.01474521574067E-16,0.000871555185129347,
0.00160565474756778),.UNSPECIFIED.);
#811=B_SPLINE_CURVE_WITH_KNOTS('',3,(#19285,#19286,#19287,#19288,#19289,
#19290,#19291,#19292,#19293,#19294),.UNSPECIFIED.,.F.,.F.,(4,2,2,2,4),(-0.260724731516495,
-0.199727802451476,-0.130390835656153,-0.0610645770440646,0.),
 .UNSPECIFIED.);
#812=B_SPLINE_CURVE_WITH_KNOTS('',3,(#19296,#19297,#19298,#19299,#19300,
#19301,#19302),.UNSPECIFIED.,.F.,.F.,(4,3,4),(0.,0.000879527967509314,0.00156997524831662),
 .UNSPECIFIED.);
#813=B_SPLINE_CURVE_WITH_KNOTS('',3,(#19306,#19307,#19308,#19309,#19310,
#19311,#19312),.UNSPECIFIED.,.F.,.F.,(4,3,4),(1.56125112837913E-17,0.000871555184791312,
0.00160565474756646),.UNSPECIFIED.);
#814=B_SPLINE_CURVE_WITH_KNOTS('',3,(#19314,#19315,#19316,#19317,#19318,
#19319,#19320,#19321,#19322,#19323),.UNSPECIFIED.,.F.,.F.,(4,2,2,2,4),(-0.260724731519916,
-0.199727802453943,-0.130390835657558,-0.0610645770444119,0.),
 .UNSPECIFIED.);
#815=B_SPLINE_CURVE_WITH_KNOTS('',3,(#19325,#19326,#19327,#19328,#19329,
#19330,#19331),.UNSPECIFIED.,.F.,.F.,(4,3,4),(0.,0.000879527967500359,0.00156997524831529),
 .UNSPECIFIED.);
#816=B_SPLINE_CURVE_WITH_KNOTS('',3,(#19335,#19336,#19337,#19338,#19339,
#19340,#19341),.UNSPECIFIED.,.F.,.F.,(4,3,4),(1.4304896245382E-17,0.000871555184787351,
0.0016056547475651),.UNSPECIFIED.);
#817=B_SPLINE_CURVE_WITH_KNOTS('',3,(#19343,#19344,#19345,#19346,#19347,
#19348,#19349,#19350,#19351,#19352),.UNSPECIFIED.,.F.,.F.,(4,2,2,2,4),(-0.260724731519916,
-0.199727802453942,-0.130390835657559,-0.0610645770444123,0.),
 .UNSPECIFIED.);
#818=B_SPLINE_CURVE_WITH_KNOTS('',3,(#19354,#19355,#19356,#19357,#19358,
#19359,#19360),.UNSPECIFIED.,.F.,.F.,(4,3,4),(0.,0.000879527967502405,0.00156997524831393),
 .UNSPECIFIED.);
#819=B_SPLINE_CURVE_WITH_KNOTS('',3,(#19364,#19365,#19366,#19367,#19368,
#19369,#19370),.UNSPECIFIED.,.F.,.F.,(4,3,4),(1.04083408558608E-17,0.000871555184779143,
0.00160565474756374),.UNSPECIFIED.);
#820=B_SPLINE_CURVE_WITH_KNOTS('',3,(#19372,#19373,#19374,#19375,#19376,
#19377,#19378,#19379,#19380,#19381),.UNSPECIFIED.,.F.,.F.,(4,2,2,2,4),(-0.260724731519971,
-0.199727802453984,-0.130390835657585,-0.061064577044418,0.),
 .UNSPECIFIED.);
#821=B_SPLINE_CURVE_WITH_KNOTS('',3,(#19383,#19384,#19385,#19386,#19387,
#19388,#19389),.UNSPECIFIED.,.F.,.F.,(4,3,4),(0.,0.000879527967498967,0.00156997524831261),
 .UNSPECIFIED.);
#822=B_SPLINE_CURVE_WITH_KNOTS('',3,(#19393,#19394,#19395,#19396,#19397,
#19398,#19399),.UNSPECIFIED.,.F.,.F.,(4,3,4),(3.5762240613455E-18,0.00087155518478463,
0.00160565474756239),.UNSPECIFIED.);
#823=B_SPLINE_CURVE_WITH_KNOTS('',3,(#19401,#19402,#19403,#19404,#19405,
#19406,#19407,#19408,#19409,#19410),.UNSPECIFIED.,.F.,.F.,(4,2,2,2,4),(-0.260724731519967,
-0.199727802453978,-0.130390835657575,-0.0610645770444141,0.),
 .UNSPECIFIED.);
#824=B_SPLINE_CURVE_WITH_KNOTS('',3,(#19412,#19413,#19414,#19415,#19416,
#19417,#19418),.UNSPECIFIED.,.F.,.F.,(4,3,4),(0.,0.000879527967511419,0.00156997524831123),
 .UNSPECIFIED.);
#825=B_SPLINE_CURVE_WITH_KNOTS('',3,(#19422,#19423,#19424,#19425,#19426,
#19427,#19428),.UNSPECIFIED.,.F.,.F.,(4,3,4),(7.81246474747696E-18,0.000871555184784776,
0.00160565474756103),.UNSPECIFIED.);
#826=B_SPLINE_CURVE_WITH_KNOTS('',3,(#19430,#19431,#19432,#19433,#19434,
#19435,#19436,#19437,#19438,#19439),.UNSPECIFIED.,.F.,.F.,(4,2,2,2,4),(-0.260724731519981,
-0.199727802453996,-0.130390835657592,-0.0610645770444198,0.),
 .UNSPECIFIED.);
#827=B_SPLINE_CURVE_WITH_KNOTS('',3,(#19441,#19442,#19443,#19444,#19445,
#19446,#19447),.UNSPECIFIED.,.F.,.F.,(4,3,4),(1.9930455364338E-17,0.00087952796764905,
0.00156997524830989),.UNSPECIFIED.);
#828=B_SPLINE_CURVE_WITH_KNOTS('',3,(#19451,#19452,#19453,#19454,#19455,
#19456,#19457),.UNSPECIFIED.,.F.,.F.,(4,3,4),(1.97026712507607E-17,0.000871555184781697,
0.00160565474757729),.UNSPECIFIED.);
#829=B_SPLINE_CURVE_WITH_KNOTS('',3,(#19459,#19460,#19461,#19462,#19463,
#19464,#19465,#19466,#19467,#19468),.UNSPECIFIED.,.F.,.F.,(4,2,2,2,4),(-0.260724731519855,
-0.199727802453898,-0.130390835657533,-0.0610645770444068,0.),
 .UNSPECIFIED.);
#830=B_SPLINE_CURVE_WITH_KNOTS('',3,(#19470,#19471,#19472,#19473,#19474,
#19475,#19476),.UNSPECIFIED.,.F.,.F.,(4,3,4),(0.,0.000879527967652466,0.00156997524832605),
 .UNSPECIFIED.);
#831=B_SPLINE_CURVE_WITH_KNOTS('',3,(#19480,#19481,#19482,#19483,#19484,
#19485,#19486),.UNSPECIFIED.,.F.,.F.,(4,3,4),(3.46944695195361E-18,0.000871555184779645,
0.00160565474757727),.UNSPECIFIED.);
#832=B_SPLINE_CURVE_WITH_KNOTS('',3,(#19488,#19489,#19490,#19491,#19492,
#19493,#19494,#19495,#19496,#19497),.UNSPECIFIED.,.F.,.F.,(4,2,2,2,4),(-0.260724731519956,
-0.199727802453977,-0.130390835657575,-0.0610645770444154,0.),
 .UNSPECIFIED.);
#833=B_SPLINE_CURVE_WITH_KNOTS('',3,(#19499,#19500,#19501,#19502,#19503,
#19504,#19505),.UNSPECIFIED.,.F.,.F.,(4,3,4),(0.,0.000879527967652087,0.00156997524832604),
 .UNSPECIFIED.);
#834=B_SPLINE_CURVE_WITH_KNOTS('',3,(#19509,#19510,#19511,#19512,#19513,
#19514,#19515),.UNSPECIFIED.,.F.,.F.,(4,3,4),(3.46944695195361E-18,0.000871555184781849,
0.00160565474757726),.UNSPECIFIED.);
#835=B_SPLINE_CURVE_WITH_KNOTS('',3,(#19517,#19518,#19519,#19520,#19521,
#19522,#19523,#19524,#19525,#19526),.UNSPECIFIED.,.F.,.F.,(4,2,2,2,4),(-0.260724731519955,
-0.199727802453976,-0.130390835657579,-0.0610645770444187,0.),
 .UNSPECIFIED.);
#836=B_SPLINE_CURVE_WITH_KNOTS('',3,(#19528,#19529,#19530,#19531,#19532,
#19533,#19534),.UNSPECIFIED.,.F.,.F.,(4,3,4),(0.,0.000879527967511223,0.00156997524832604),
 .UNSPECIFIED.);
#837=B_SPLINE_CURVE_WITH_KNOTS('',3,(#19538,#19539,#19540,#19541,#19542,
#19543,#19544),.UNSPECIFIED.,.F.,.F.,(4,3,4),(2.32821605822755E-16,0.000871555185125512,
0.00160565474757726),.UNSPECIFIED.);
#838=B_SPLINE_CURVE_WITH_KNOTS('',3,(#19546,#19547,#19548,#19549,#19550,
#19551,#19552,#19553,#19554,#19555),.UNSPECIFIED.,.F.,.F.,(4,2,2,2,4),(-0.260724731516488,
-0.199727802451468,-0.130390835656146,-0.0610645770440642,0.),
 .UNSPECIFIED.);
#839=B_SPLINE_CURVE_WITH_KNOTS('',3,(#19557,#19558,#19559,#19560,#19561,
#19562,#19563),.UNSPECIFIED.,.F.,.F.,(4,3,4),(0.,0.000879527967497746,0.00156997524832604),
 .UNSPECIFIED.);
#840=B_SPLINE_CURVE_WITH_KNOTS('',3,(#19567,#19568,#19569,#19570,#19571,
#19572,#19573),.UNSPECIFIED.,.F.,.F.,(4,3,4),(3.46944695195361E-18,0.000871555184784586,
0.00160565474757726),.UNSPECIFIED.);
#841=B_SPLINE_CURVE_WITH_KNOTS('',3,(#19575,#19576,#19577,#19578,#19579,
#19580,#19581,#19582,#19583,#19584),.UNSPECIFIED.,.F.,.F.,(4,2,2,2,4),(-0.2607247315199,
-0.199727802453934,-0.130390835657557,-0.0610645770444129,0.),
 .UNSPECIFIED.);
#842=B_SPLINE_CURVE_WITH_KNOTS('',3,(#19586,#19587,#19588,#19589,#19590,
#19591,#19592),.UNSPECIFIED.,.F.,.F.,(4,3,4),(0.,0.000879527967505927,0.00156997524832604),
 .UNSPECIFIED.);
#843=B_SPLINE_CURVE_WITH_KNOTS('',3,(#19596,#19597,#19598,#19599,#19600,
#19601,#19602),.UNSPECIFIED.,.F.,.F.,(4,3,4),(0.,0.000871555184783887,0.00160565474757725),
 .UNSPECIFIED.);
#844=B_SPLINE_CURVE_WITH_KNOTS('',3,(#19604,#19605,#19606,#19607,#19608,
#19609,#19610,#19611,#19612,#19613),.UNSPECIFIED.,.F.,.F.,(4,2,2,2,4),(-0.26072473151999,
-0.199727802454001,-0.13039083565759,-0.0610645770444177,0.),
 .UNSPECIFIED.);
#845=B_SPLINE_CURVE_WITH_KNOTS('',3,(#19615,#19616,#19617,#19618,#19619,
#19620,#19621),.UNSPECIFIED.,.F.,.F.,(4,3,4),(0.,0.000879527967504626,0.00156997524832606),
 .UNSPECIFIED.);
#846=B_SPLINE_CURVE_WITH_KNOTS('',3,(#19625,#19626,#19627,#19628,#19629,
#19630,#19631),.UNSPECIFIED.,.F.,.F.,(4,3,4),(4.9065389333868E-18,0.000871555184783266,
0.00160565474757725),.UNSPECIFIED.);
#847=B_SPLINE_CURVE_WITH_KNOTS('',3,(#19633,#19634,#19635,#19636,#19637,
#19638,#19639,#19640,#19641,#19642),.UNSPECIFIED.,.F.,.F.,(4,2,2,2,4),(-0.260724731522011,
-0.199727808951148,-0.130390835646158,-0.0610645826755033,0.),
 .UNSPECIFIED.);
#848=B_SPLINE_CURVE_WITH_KNOTS('',3,(#19644,#19645,#19646,#19647,#19648,
#19649,#19650),.UNSPECIFIED.,.F.,.F.,(4,3,4),(0.,0.000879527967507628,0.00156997524832605),
 .UNSPECIFIED.);
#849=B_SPLINE_CURVE_WITH_KNOTS('',3,(#19654,#19655,#19656,#19657,#19658,
#19659,#19660),.UNSPECIFIED.,.F.,.F.,(4,3,4),(2.09578719802802E-16,0.000871555185122462,
0.00160565474757726),.UNSPECIFIED.);
#850=B_SPLINE_CURVE_WITH_KNOTS('',3,(#19662,#19663,#19664,#19665,#19666,
#19667,#19668,#19669,#19670,#19671),.UNSPECIFIED.,.F.,.F.,(4,2,2,2,4),(-0.260724731516458,
-0.199727802451451,-0.130390835656143,-0.0610645770440656,0.),
 .UNSPECIFIED.);
#851=B_SPLINE_CURVE_WITH_KNOTS('',3,(#19673,#19674,#19675,#19676,#19677,
#19678,#19679),.UNSPECIFIED.,.F.,.F.,(4,3,4),(0.,0.000879527967500393,0.00156997524832608),
 .UNSPECIFIED.);
#852=B_SPLINE_CURVE_WITH_KNOTS('',3,(#19683,#19684,#19685,#19686,#19687,
#19688,#19689),.UNSPECIFIED.,.F.,.F.,(4,3,4),(9.34177181294034E-18,0.000871555184782784,
0.00160565474757725),.UNSPECIFIED.);
#853=B_SPLINE_CURVE_WITH_KNOTS('',3,(#19691,#19692,#19693,#19694,#19695,
#19696,#19697,#19698,#19699,#19700),.UNSPECIFIED.,.F.,.F.,(4,2,2,2,4),(-0.260724731519931,
-0.199727802453962,-0.130390835657569,-0.0610645770444118,0.),
 .UNSPECIFIED.);
#854=B_SPLINE_CURVE_WITH_KNOTS('',3,(#19702,#19703,#19704,#19705,#19706,
#19707,#19708),.UNSPECIFIED.,.F.,.F.,(4,3,4),(0.,0.000879527967502687,0.00156997524832604),
 .UNSPECIFIED.);
#855=B_SPLINE_CURVE_WITH_KNOTS('',3,(#19712,#19713,#19714,#19715,#19716,
#19717,#19718),.UNSPECIFIED.,.F.,.F.,(4,3,4),(3.87895961444886E-18,0.000871555184780596,
0.00160565474757726),.UNSPECIFIED.);
#856=B_SPLINE_CURVE_WITH_KNOTS('',3,(#19720,#19721,#19722,#19723,#19724,
#19725,#19726,#19727,#19728,#19729),.UNSPECIFIED.,.F.,.F.,(4,2,2,2,4),(-0.260724731519954,
-0.199727802453973,-0.130390835657584,-0.0610645770444205,0.),
 .UNSPECIFIED.);
#857=B_SPLINE_CURVE_WITH_KNOTS('',3,(#19731,#19732,#19733,#19734,#19735,
#19736,#19737),.UNSPECIFIED.,.F.,.F.,(4,3,4),(0.,0.000879527967508752,0.00156997524832606),
 .UNSPECIFIED.);
#858=B_SPLINE_CURVE_WITH_KNOTS('',3,(#19741,#19742,#19743,#19744,#19745,
#19746,#19747),.UNSPECIFIED.,.F.,.F.,(4,3,4),(7.81246474747696E-18,0.000871555184790998,
0.00160565474757727),.UNSPECIFIED.);
#859=B_SPLINE_CURVE_WITH_KNOTS('',3,(#19749,#19750,#19751,#19752,#19753,
#19754),.UNSPECIFIED.,.F.,.F.,(4,2,4),(0.,0.0407463936727646,0.0482791015350969),
 .UNSPECIFIED.);
#860=B_SPLINE_CURVE_WITH_KNOTS('',3,(#19759,#19760,#19761,#19762,#19763,
#19764,#19765,#19766,#19767,#19768),.UNSPECIFIED.,.F.,.F.,(4,2,2,2,4),(0.0482791015350969,
0.0839662032253167,0.15419854744165,0.209083280006158,0.260520203475897),
 .UNSPECIFIED.);
#861=B_SPLINE_CURVE_WITH_KNOTS('',3,(#19770,#19771,#19772,#19773,#19774,
#19775,#19776),.UNSPECIFIED.,.F.,.F.,(4,3,4),(0.,0.000879527967511759,0.00156997524832607),
 .UNSPECIFIED.);
#862=B_SPLINE_CURVE_WITH_KNOTS('',3,(#19780,#19781,#19782,#19783,#19784,
#19785,#19786),.UNSPECIFIED.,.F.,.F.,(4,3,4),(3.46944695195361E-18,0.000871555184791261,
0.00160565474757729),.UNSPECIFIED.);
#863=B_SPLINE_CURVE_WITH_KNOTS('',3,(#19788,#19789,#19790,#19791,#19792,
#19793,#19794,#19795,#19796,#19797),.UNSPECIFIED.,.F.,.F.,(4,2,2,2,4),(-0.260724731519979,
-0.199727802453994,-0.130390835657588,-0.061064577044418,0.),
 .UNSPECIFIED.);
#864=B_SPLINE_CURVE_WITH_KNOTS('',3,(#19799,#19800,#19801,#19802,#19803,
#19804,#19805),.UNSPECIFIED.,.F.,.F.,(4,3,4),(0.,0.000879527967511587,0.00156997524832605),
 .UNSPECIFIED.);
#865=B_SPLINE_CURVE_WITH_KNOTS('',3,(#19809,#19810,#19811,#19812,#19813,
#19814,#19815),.UNSPECIFIED.,.F.,.F.,(4,3,4),(2.14776701328641E-16,0.000871555185130942,
0.00160565474757727),.UNSPECIFIED.);
#866=B_SPLINE_CURVE_WITH_KNOTS('',3,(#19817,#19818,#19819,#19820,#19821,
#19822,#19823,#19824,#19825,#19826),.UNSPECIFIED.,.F.,.F.,(4,2,2,2,4),(-0.260724731516507,
-0.19972780245148,-0.130390835656155,-0.0610645770440656,0.),
 .UNSPECIFIED.);
#867=B_SPLINE_CURVE_WITH_KNOTS('',3,(#19828,#19829,#19830,#19831,#19832,
#19833,#19834),.UNSPECIFIED.,.F.,.F.,(4,3,4),(0.,0.000879527967649747,0.00156997524832607),
 .UNSPECIFIED.);
#868=B_SPLINE_CURVE_WITH_KNOTS('',3,(#19838,#19839,#19840,#19841,#19842,
#19843,#19844),.UNSPECIFIED.,.F.,.F.,(4,3,4),(1.98214456752023E-16,0.000871555185118887,
0.00160565474757726),.UNSPECIFIED.);
#869=B_SPLINE_CURVE_WITH_KNOTS('',3,(#19846,#19847,#19848,#19849,#19850,
#19851,#19852,#19853,#19854,#19855),.UNSPECIFIED.,.F.,.F.,(4,2,2,2,4),(-0.260724731516436,
-0.199727802451429,-0.130390835656129,-0.0610645770440628,0.),
 .UNSPECIFIED.);
#870=B_SPLINE_CURVE_WITH_KNOTS('',3,(#19857,#19858,#19859,#19860,#19861,
#19862,#19863),.UNSPECIFIED.,.F.,.F.,(4,3,4),(0.,0.000879527967649307,0.00156997524832607),
 .UNSPECIFIED.);
#871=B_SPLINE_CURVE_WITH_KNOTS('',3,(#19867,#19868,#19869,#19870,#19871,
#19872,#19873),.UNSPECIFIED.,.F.,.F.,(4,3,4),(2.04579727988785E-16,0.00087155518513034,
0.00160565474757726),.UNSPECIFIED.);
#872=B_SPLINE_CURVE_WITH_KNOTS('',3,(#19875,#19876,#19877,#19878,#19879,
#19880,#19881,#19882,#19883,#19884),.UNSPECIFIED.,.F.,.F.,(4,2,2,2,4),(-0.260724731516512,
-0.199727802451486,-0.130390835656163,-0.0610645770440718,0.),
 .UNSPECIFIED.);
#873=B_SPLINE_CURVE_WITH_KNOTS('',3,(#19886,#19887,#19888,#19889,#19890,
#19891,#19892),.UNSPECIFIED.,.F.,.F.,(4,3,4),(0.,0.000879527967646912,0.00156997524832608),
 .UNSPECIFIED.);
#874=B_SPLINE_CURVE_WITH_KNOTS('',3,(#19896,#19897,#19898,#19899,#19900,
#19901,#19902),.UNSPECIFIED.,.F.,.F.,(4,3,4),(1.95654969040488E-16,0.000871555185114593,
0.00160565474757726),.UNSPECIFIED.);
#875=B_SPLINE_CURVE_WITH_KNOTS('',3,(#19904,#19905,#19906,#19907,#19908,
#19909,#19910,#19911,#19912,#19913),.UNSPECIFIED.,.F.,.F.,(4,2,2,2,4),(-0.260724731516399,
-0.199727802451402,-0.130390835656104,-0.0610645770440508,0.),
 .UNSPECIFIED.);
#876=B_SPLINE_CURVE_WITH_KNOTS('',3,(#19915,#19916,#19917,#19918,#19919,
#19920,#19921),.UNSPECIFIED.,.F.,.F.,(4,3,4),(0.,0.000879527967647974,0.00156997524832605),
 .UNSPECIFIED.);
#877=B_SPLINE_CURVE_WITH_KNOTS('',3,(#19925,#19926,#19927,#19928,#19929,
#19930,#19931),.UNSPECIFIED.,.F.,.F.,(4,3,4),(1.30968750346023E-17,0.000871555184789597,
0.00160565474757726),.UNSPECIFIED.);
#878=B_SPLINE_CURVE_WITH_KNOTS('',3,(#19933,#19934,#19935,#19936,#19937,
#19938,#19939,#19940,#19941,#19942),.UNSPECIFIED.,.F.,.F.,(4,2,2,2,4),(-0.260724731519943,
-0.199727802453962,-0.130390835657567,-0.0610645770444133,0.),
 .UNSPECIFIED.);
#879=B_SPLINE_CURVE_WITH_KNOTS('',3,(#19944,#19945,#19946,#19947,#19948,
#19949,#19950),.UNSPECIFIED.,.F.,.F.,(4,3,4),(0.,0.000879527967504028,0.00156997524832602),
 .UNSPECIFIED.);
#880=B_SPLINE_CURVE_WITH_KNOTS('',3,(#19954,#19955,#19956,#19957,#19958,
#19959,#19960),.UNSPECIFIED.,.F.,.F.,(4,3,4),(1.73472347597681E-18,0.000871555184776652,
0.00160565474757725),.UNSPECIFIED.);
#881=B_SPLINE_CURVE_WITH_KNOTS('',3,(#19962,#19963,#19964,#19965,#19966,
#19967,#19968,#19969,#19970,#19971),.UNSPECIFIED.,.F.,.F.,(4,2,2,2,4),(-0.260724731519973,
-0.199727802453988,-0.130390835657582,-0.0610645770444168,0.),
 .UNSPECIFIED.);
#882=B_SPLINE_CURVE_WITH_KNOTS('',3,(#19973,#19974,#19975,#19976,#19977,
#19978,#19979),.UNSPECIFIED.,.F.,.F.,(4,3,4),(0.,0.0008795279676465,0.00156997524832604),
 .UNSPECIFIED.);
#883=B_SPLINE_CURVE_WITH_KNOTS('',3,(#19983,#19984,#19985,#19986,#19987,
#19988,#19989),.UNSPECIFIED.,.F.,.F.,(4,3,4),(2.57885184514585E-17,0.000871555184785543,
0.00160565474757727),.UNSPECIFIED.);
#884=B_SPLINE_CURVE_WITH_KNOTS('',3,(#19991,#19992,#19993,#19994,#19995,
#19996,#19997,#19998,#19999,#20000),.UNSPECIFIED.,.F.,.F.,(4,2,2,2,4),(-0.260724731519904,
-0.199727802453939,-0.130390835657553,-0.0610645770444076,0.),
 .UNSPECIFIED.);
#885=B_SPLINE_CURVE_WITH_KNOTS('',3,(#20002,#20003,#20004,#20005,#20006,
#20007,#20008),.UNSPECIFIED.,.F.,.F.,(4,3,4),(0.,0.000879527967654812,0.00156997524832605),
 .UNSPECIFIED.);
#886=B_SPLINE_CURVE_WITH_KNOTS('',3,(#20012,#20013,#20014,#20015,#20016,
#20017,#20018),.UNSPECIFIED.,.F.,.F.,(4,3,4),(1.73472347597681E-18,0.000871555184781887,
0.00160565474757726),.UNSPECIFIED.);
#887=B_SPLINE_CURVE_WITH_KNOTS('',3,(#20020,#20021,#20022,#20023,#20024,
#20025,#20026,#20027,#20028,#20029),.UNSPECIFIED.,.F.,.F.,(4,2,2,2,4),(-0.260724731519953,
-0.19972780245398,-0.130390835657581,-0.0610645770444158,0.),
 .UNSPECIFIED.);
#888=B_SPLINE_CURVE_WITH_KNOTS('',3,(#20031,#20032,#20033,#20034,#20035,
#20036,#20037),.UNSPECIFIED.,.F.,.F.,(4,3,4),(0.,0.000879527967510002,0.00156997524832605),
 .UNSPECIFIED.);
#889=B_SPLINE_CURVE_WITH_KNOTS('',3,(#20041,#20042,#20043,#20044,#20045,
#20046,#20047),.UNSPECIFIED.,.F.,.F.,(4,3,4),(1.01522088571945E-17,0.00087155518478881,
0.00160565474757727),.UNSPECIFIED.);
#890=B_SPLINE_CURVE_WITH_KNOTS('',3,(#20049,#20050,#20051,#20052,#20053,
#20054,#20055,#20056,#20057,#20058),.UNSPECIFIED.,.F.,.F.,(4,2,2,2,4),(-0.260724731519909,
-0.199727802453946,-0.130390835657565,-0.0610645770444126,0.),
 .UNSPECIFIED.);
#891=B_SPLINE_CURVE_WITH_KNOTS('',3,(#20060,#20061,#20062,#20063,#20064,
#20065,#20066),.UNSPECIFIED.,.F.,.F.,(4,3,4),(0.,0.000879527967647106,0.00156997524832605),
 .UNSPECIFIED.);
#892=B_SPLINE_CURVE_WITH_KNOTS('',3,(#20070,#20071,#20072,#20073,#20074,
#20075,#20076),.UNSPECIFIED.,.F.,.F.,(4,3,4),(9.9846720473553E-18,0.000871555184783746,
0.00160565474757726),.UNSPECIFIED.);
#893=B_SPLINE_CURVE_WITH_KNOTS('',3,(#20078,#20079,#20080,#20081,#20082,
#20083,#20084,#20085,#20086,#20087),.UNSPECIFIED.,.F.,.F.,(4,2,2,2,4),(-0.26072473151994,
-0.199727802453954,-0.130390835657562,-0.0610645770444132,0.),
 .UNSPECIFIED.);
#894=B_SPLINE_CURVE_WITH_KNOTS('',3,(#20089,#20090,#20091,#20092,#20093,
#20094,#20095),.UNSPECIFIED.,.F.,.F.,(4,3,4),(0.,0.000879527967650889,0.00156997524832608),
 .UNSPECIFIED.);
#895=B_SPLINE_CURVE_WITH_KNOTS('',3,(#20099,#20100,#20101,#20102,#20103,
#20104,#20105),.UNSPECIFIED.,.F.,.F.,(4,3,4),(3.46944695195361E-18,0.000871555184784394,
0.00160565474757728),.UNSPECIFIED.);
#896=B_SPLINE_CURVE_WITH_KNOTS('',3,(#20107,#20108,#20109,#20110,#20111,
#20112,#20113,#20114,#20115,#20116),.UNSPECIFIED.,.F.,.F.,(4,2,2,2,4),(-0.260724731519926,
-0.19972780245395,-0.130390835657561,-0.061064577044412,0.),
 .UNSPECIFIED.);
#897=B_SPLINE_CURVE_WITH_KNOTS('',3,(#20118,#20119,#20120,#20121,#20122,
#20123,#20124),.UNSPECIFIED.,.F.,.F.,(4,3,4),(0.,0.000879527967499868,0.00156997524832605),
 .UNSPECIFIED.);
#898=B_SPLINE_CURVE_WITH_KNOTS('',3,(#20128,#20129,#20130,#20131,#20132,
#20133,#20134),.UNSPECIFIED.,.F.,.F.,(4,3,4),(1.73472347597681E-18,0.000871555184787591,
0.00160565474757725),.UNSPECIFIED.);
#899=B_SPLINE_CURVE_WITH_KNOTS('',3,(#20136,#20137,#20138,#20139,#20140,
#20141,#20142,#20143,#20144,#20145),.UNSPECIFIED.,.F.,.F.,(4,2,2,2,4),(-0.260724731519915,
-0.199727802453947,-0.130390835657561,-0.0610645770444091,0.),
 .UNSPECIFIED.);
#900=B_SPLINE_CURVE_WITH_KNOTS('',3,(#20147,#20148,#20149,#20150,#20151,
#20152,#20153),.UNSPECIFIED.,.F.,.F.,(4,3,4),(0.,0.000879527967506563,0.00156997524832605),
 .UNSPECIFIED.);
#901=B_SPLINE_CURVE_WITH_KNOTS('',3,(#20157,#20158,#20159,#20160,#20161,
#20162,#20163),.UNSPECIFIED.,.F.,.F.,(4,3,4),(2.09154710985512E-16,0.000871555185128014,
0.00160565474757726),.UNSPECIFIED.);
#902=B_SPLINE_CURVE_WITH_KNOTS('',3,(#20165,#20166,#20167,#20168,#20169,
#20170,#20171,#20172,#20173,#20174),.UNSPECIFIED.,.F.,.F.,(4,2,2,2,4),(-0.260724731516491,
-0.199727802451466,-0.130390835656145,-0.0610645770440631,0.),
 .UNSPECIFIED.);
#903=B_SPLINE_CURVE_WITH_KNOTS('',3,(#20176,#20177,#20178,#20179,#20180,
#20181,#20182),.UNSPECIFIED.,.F.,.F.,(4,3,4),(0.,0.000879527967651056,0.00156997524832606),
 .UNSPECIFIED.);
#904=B_SPLINE_CURVE_WITH_KNOTS('',3,(#20186,#20187,#20188,#20189,#20190,
#20191,#20192),.UNSPECIFIED.,.F.,.F.,(4,3,4),(0.,0.000871555184787238,0.00160565474757725),
 .UNSPECIFIED.);
#905=B_SPLINE_CURVE_WITH_KNOTS('',3,(#20194,#20195,#20196,#20197,#20198,
#20199,#20200,#20201,#20202,#20203),.UNSPECIFIED.,.F.,.F.,(4,2,2,2,4),(-0.260724731519923,
-0.199727802453942,-0.130390835657558,-0.0610645770444118,0.),
 .UNSPECIFIED.);
#906=B_SPLINE_CURVE_WITH_KNOTS('',3,(#20205,#20206,#20207,#20208,#20209,
#20210,#20211),.UNSPECIFIED.,.F.,.F.,(4,3,4),(0.,0.00087952796764459,0.00156997524832608),
 .UNSPECIFIED.);
#907=B_SPLINE_CURVE_WITH_KNOTS('',3,(#20215,#20216,#20217,#20218,#20219,
#20220,#20221),.UNSPECIFIED.,.F.,.F.,(4,3,4),(8.49837472194074E-18,0.000871555184788193,
0.00160565474757728),.UNSPECIFIED.);
#908=B_SPLINE_CURVE_WITH_KNOTS('',3,(#20223,#20224,#20225,#20226,#20227,
#20228,#20229,#20230,#20231,#20232),.UNSPECIFIED.,.F.,.F.,(4,2,2,2,4),(-0.260724731519922,
-0.199727802453952,-0.130390835657565,-0.0610645770444117,0.),
 .UNSPECIFIED.);
#909=B_SPLINE_CURVE_WITH_KNOTS('',3,(#20234,#20235,#20236,#20237,#20238,
#20239,#20240),.UNSPECIFIED.,.F.,.F.,(4,3,4),(0.,0.000879527967508577,0.00156997524832604),
 .UNSPECIFIED.);
#910=B_SPLINE_CURVE_WITH_KNOTS('',3,(#20244,#20245,#20246,#20247,#20248,
#20249,#20250),.UNSPECIFIED.,.F.,.F.,(4,3,4),(2.05935861929181E-16,0.000871555185115414,
0.00160565474757727),.UNSPECIFIED.);
#911=B_SPLINE_CURVE_WITH_KNOTS('',3,(#20252,#20253,#20254,#20255,#20256,
#20257,#20258,#20259,#20260,#20261),.UNSPECIFIED.,.F.,.F.,(4,2,2,2,4),(-0.260724731516467,
-0.199727802451455,-0.130390835656149,-0.0610645770440673,0.),
 .UNSPECIFIED.);
#912=B_SPLINE_CURVE_WITH_KNOTS('',3,(#20263,#20264,#20265,#20266,#20267,
#20268,#20269),.UNSPECIFIED.,.F.,.F.,(4,3,4),(0.,0.000879527967500517,0.00156997524832606),
 .UNSPECIFIED.);
#913=B_SPLINE_CURVE_WITH_KNOTS('',3,(#20273,#20274,#20275,#20276,#20277,
#20278,#20279),.UNSPECIFIED.,.F.,.F.,(4,3,4),(4.9065389333868E-18,0.000871555184783715,
0.00160565474757726),.UNSPECIFIED.);
#914=B_SPLINE_CURVE_WITH_KNOTS('',3,(#20281,#20282,#20283,#20284,#20285,
#20286,#20287,#20288,#20289,#20290),.UNSPECIFIED.,.F.,.F.,(4,2,2,2,4),(-0.260724731521994,
-0.199727808951145,-0.130390835646155,-0.0610645826755003,0.),
 .UNSPECIFIED.);
#915=B_SPLINE_CURVE_WITH_KNOTS('',3,(#20292,#20293,#20294,#20295,#20296,
#20297,#20298),.UNSPECIFIED.,.F.,.F.,(4,3,4),(0.,0.000879527967502014,0.00156997524832605),
 .UNSPECIFIED.);
#916=B_SPLINE_CURVE_WITH_KNOTS('',3,(#20302,#20303,#20304,#20305,#20306,
#20307,#20308),.UNSPECIFIED.,.F.,.F.,(4,3,4),(0.,0.000871555184778678,0.00160565474757727),
 .UNSPECIFIED.);
#917=B_SPLINE_CURVE_WITH_KNOTS('',3,(#20310,#20311,#20312,#20313,#20314,
#20315,#20316,#20317,#20318,#20319),.UNSPECIFIED.,.F.,.F.,(4,2,2,2,4),(-0.260724731519916,
-0.199727802453945,-0.130390835657561,-0.0610645770444109,0.),
 .UNSPECIFIED.);
#918=B_SPLINE_CURVE_WITH_KNOTS('',3,(#20321,#20322,#20323,#20324,#20325,
#20326,#20327),.UNSPECIFIED.,.F.,.F.,(4,3,4),(0.,0.000879527967649045,0.00156997524832605),
 .UNSPECIFIED.);
#919=B_SPLINE_CURVE_WITH_KNOTS('',3,(#20331,#20332,#20333,#20334,#20335,
#20336,#20337),.UNSPECIFIED.,.F.,.F.,(4,3,4),(7.94950163848063E-18,0.000871555184775057,
0.00160565474757727),.UNSPECIFIED.);
#920=B_SPLINE_CURVE_WITH_KNOTS('',3,(#20339,#20340,#20341,#20342,#20343,
#20344,#20345,#20346,#20347,#20348),.UNSPECIFIED.,.F.,.F.,(4,2,2,2,4),(-0.260724731519915,
-0.199727802453944,-0.13039083565756,-0.0610645770444119,0.),
 .UNSPECIFIED.);
#921=B_SPLINE_CURVE_WITH_KNOTS('',3,(#20350,#20351,#20352,#20353,#20354,
#20355,#20356),.UNSPECIFIED.,.F.,.F.,(4,3,4),(0.,0.000879527967640991,0.00156997524832605),
 .UNSPECIFIED.);
#922=B_SPLINE_CURVE_WITH_KNOTS('',3,(#20360,#20361,#20362,#20363,#20364,
#20365,#20366),.UNSPECIFIED.,.F.,.F.,(4,3,4),(0.,0.000871555184782733,0.00160565474757727),
 .UNSPECIFIED.);
#923=B_SPLINE_CURVE_WITH_KNOTS('',3,(#20368,#20369,#20370,#20371,#20372,
#20373,#20374,#20375,#20376,#20377),.UNSPECIFIED.,.F.,.F.,(4,2,2,2,4),(-0.260724731519912,
-0.199727802453946,-0.130390835657566,-0.0610645770444142,0.),
 .UNSPECIFIED.);
#924=B_SPLINE_CURVE_WITH_KNOTS('',3,(#20379,#20380,#20381,#20382,#20383,
#20384,#20385),.UNSPECIFIED.,.F.,.F.,(4,3,4),(0.,0.00087952796764763,0.00156997524832606),
 .UNSPECIFIED.);
#925=B_SPLINE_CURVE_WITH_KNOTS('',3,(#20388,#20389,#20390,#20391,#20392,
#20393,#20394),.UNSPECIFIED.,.F.,.F.,(4,3,4),(7.81246474747696E-18,0.000871555184773631,
0.00160565474757588),.UNSPECIFIED.);
#926=B_SPLINE_CURVE_WITH_KNOTS('',3,(#20407,#20408,#20409,#20410,#20411,
#20412,#20413,#20414,#20415,#20416,#20417,#20418),.UNSPECIFIED.,.F.,.F.,
(4,2,2,2,2,4),(0.,0.0407569430586041,0.0839882141528699,0.154219975171057,
0.209093406724745,0.260520353691867),.UNSPECIFIED.);
#927=B_SPLINE_CURVE_WITH_KNOTS('',3,(#20420,#20421,#20422,#20423,#20424,
#20425,#20426),.UNSPECIFIED.,.F.,.F.,(4,3,4),(1.78811203067275E-18,0.000871811004260026,
0.00160579165132935),.UNSPECIFIED.);
#928=B_SPLINE_CURVE_WITH_KNOTS('',3,(#20430,#20431,#20432,#20433,#20434,
#20435,#20436),.UNSPECIFIED.,.F.,.F.,(4,3,4),(3.69724068824877E-17,0.000879500804028015,
0.00156989029765835),.UNSPECIFIED.);
#929=B_SPLINE_CURVE_WITH_KNOTS('',3,(#20438,#20439,#20440,#20441,#20442,
#20443,#20444,#20445,#20446,#20447),.UNSPECIFIED.,.F.,.F.,(4,2,2,2,4),(-0.260724943430805,
-0.199726494015773,-0.130391022448095,-0.0610665706517605,0.),
 .UNSPECIFIED.);
#930=B_SPLINE_CURVE_WITH_KNOTS('',3,(#20449,#20450,#20451,#20452,#20453,
#20454,#20455),.UNSPECIFIED.,.F.,.F.,(4,3,4),(7.94950163848063E-18,0.000871811004271929,
0.00160579165132327),.UNSPECIFIED.);
#931=B_SPLINE_CURVE_WITH_KNOTS('',3,(#20459,#20460,#20461,#20462,#20463,
#20464,#20465),.UNSPECIFIED.,.F.,.F.,(4,3,4),(2.7097246932071E-17,0.000879500804038936,
0.00156989029765586),.UNSPECIFIED.);
#932=B_SPLINE_CURVE_WITH_KNOTS('',3,(#20467,#20468,#20469,#20470,#20471,
#20472,#20473,#20474,#20475,#20476),.UNSPECIFIED.,.F.,.F.,(4,2,2,2,4),(-0.260724943430658,
-0.199726493772702,-0.130391022195998,-0.0610665704089927,0.),
 .UNSPECIFIED.);
#933=B_SPLINE_CURVE_WITH_KNOTS('',3,(#20478,#20479,#20480,#20481,#20482,
#20483,#20484),.UNSPECIFIED.,.F.,.F.,(4,3,4),(2.91013228173329E-14,0.000871811007982037,
0.00160579165130272),.UNSPECIFIED.);
#934=B_SPLINE_CURVE_WITH_KNOTS('',3,(#20488,#20489,#20490,#20491,#20492,
#20493,#20494),.UNSPECIFIED.,.F.,.F.,(4,3,4),(2.11749985874298E-17,0.000879500804027354,
0.00156989029765845),.UNSPECIFIED.);
#935=B_SPLINE_CURVE_WITH_KNOTS('',3,(#20496,#20497,#20498,#20499,#20500,
#20501,#20502,#20503,#20504,#20505),.UNSPECIFIED.,.F.,.F.,(4,2,2,2,4),(-0.260724943430588,
-0.199726493772793,-0.130391022195965,-0.0610665704088414,0.),
 .UNSPECIFIED.);
#936=B_SPLINE_CURVE_WITH_KNOTS('',3,(#20507,#20508,#20509,#20510,#20511,
#20512,#20513),.UNSPECIFIED.,.F.,.F.,(4,3,4),(2.91023102291187E-14,0.000871811007963625,
0.00160579165130527),.UNSPECIFIED.);
#937=B_SPLINE_CURVE_WITH_KNOTS('',3,(#20517,#20518,#20519,#20520,#20521,
#20522,#20523),.UNSPECIFIED.,.F.,.F.,(4,3,4),(2.32737576866932E-17,0.000879500804022207,
0.00156989029766219),.UNSPECIFIED.);
#938=B_SPLINE_CURVE_WITH_KNOTS('',3,(#20525,#20526,#20527,#20528,#20529,
#20530,#20531,#20532,#20533,#20534),.UNSPECIFIED.,.F.,.F.,(4,2,2,2,4),(-0.260724943430767,
-0.199726493772903,-0.130391022196058,-0.0610665704089389,0.),
 .UNSPECIFIED.);
#939=B_SPLINE_CURVE_WITH_KNOTS('',3,(#20536,#20537,#20538,#20539,#20540,
#20541,#20542),.UNSPECIFIED.,.F.,.F.,(4,3,4),(2.90971702336027E-14,0.000871811007985608,
0.00160579165129744),.UNSPECIFIED.);
#940=B_SPLINE_CURVE_WITH_KNOTS('',3,(#20546,#20547,#20548,#20549,#20550,
#20551,#20552),.UNSPECIFIED.,.F.,.F.,(4,3,4),(3.49106365300398E-17,0.000879500804038357,
0.00156989029766081),.UNSPECIFIED.);
#941=B_SPLINE_CURVE_WITH_KNOTS('',3,(#20554,#20555,#20556,#20557,#20558,
#20559,#20560,#20561,#20562,#20563),.UNSPECIFIED.,.F.,.F.,(4,2,2,2,4),(-0.260724943430475,
-0.199726493772615,-0.130391022195898,-0.061066570408873,0.),
 .UNSPECIFIED.);
#942=B_SPLINE_CURVE_WITH_KNOTS('',3,(#20565,#20566,#20567,#20568,#20569,
#20570,#20571),.UNSPECIFIED.,.F.,.F.,(4,3,4),(2.91265948333354E-14,0.000871811007982302,
0.00160579165130123),.UNSPECIFIED.);
#943=B_SPLINE_CURVE_WITH_KNOTS('',3,(#20575,#20576,#20577,#20578,#20579,
#20580,#20581),.UNSPECIFIED.,.F.,.F.,(4,3,4),(4.06458703981066E-17,0.00087950080403512,
0.00156989029766391),.UNSPECIFIED.);
#944=B_SPLINE_CURVE_WITH_KNOTS('',3,(#20583,#20584,#20585,#20586,#20587,
#20588,#20589,#20590,#20591,#20592),.UNSPECIFIED.,.F.,.F.,(4,2,2,2,4),(-0.26072494343065,
-0.199726493772769,-0.130391022195999,-0.0610665704089316,0.),
 .UNSPECIFIED.);
#945=B_SPLINE_CURVE_WITH_KNOTS('',3,(#20594,#20595,#20596,#20597,#20598,
#20599,#20600),.UNSPECIFIED.,.F.,.F.,(4,3,4),(2.91191625685097E-14,0.000871811007980137,
0.00160579165129441),.UNSPECIFIED.);
#946=B_SPLINE_CURVE_WITH_KNOTS('',3,(#20604,#20605,#20606,#20607,#20608,
#20609,#20610),.UNSPECIFIED.,.F.,.F.,(4,3,4),(2.73734747335474E-17,0.000879500804032835,
0.00156989029766265),.UNSPECIFIED.);
#947=B_SPLINE_CURVE_WITH_KNOTS('',3,(#20612,#20613,#20614,#20615,#20616,
#20617,#20618,#20619,#20620,#20621),.UNSPECIFIED.,.F.,.F.,(4,2,2,2,4),(-0.260724943430845,
-0.199726493772884,-0.130391022196103,-0.061066570409027,0.),
 .UNSPECIFIED.);
#948=B_SPLINE_CURVE_WITH_KNOTS('',3,(#20623,#20624,#20625,#20626,#20627,
#20628,#20629),.UNSPECIFIED.,.F.,.F.,(4,3,4),(2.90751839301751E-14,0.000871811007988348,
0.00160579165129659),.UNSPECIFIED.);
#949=B_SPLINE_CURVE_WITH_KNOTS('',3,(#20633,#20634,#20635,#20636,#20637,
#20638,#20639),.UNSPECIFIED.,.F.,.F.,(4,3,4),(5.18389248106846E-17,0.000879500804056453,
0.00156989029764657),.UNSPECIFIED.);
#950=B_SPLINE_CURVE_WITH_KNOTS('',3,(#20641,#20642,#20643,#20644,#20645,
#20646,#20647,#20648,#20649,#20650),.UNSPECIFIED.,.F.,.F.,(4,2,2,2,4),(-0.260724943430446,
-0.199726493772451,-0.130391022195854,-0.0610665704089763,0.),
 .UNSPECIFIED.);
#951=B_SPLINE_CURVE_WITH_KNOTS('',3,(#20652,#20653,#20654,#20655,#20656,
#20657,#20658),.UNSPECIFIED.,.F.,.F.,(4,3,4),(2.91340106381937E-14,0.00087181100798855,
0.00160579165130922),.UNSPECIFIED.);
#952=B_SPLINE_CURVE_WITH_KNOTS('',3,(#20662,#20663,#20664,#20665,#20666,
#20667,#20668),.UNSPECIFIED.,.F.,.F.,(4,3,4),(5.56194657756796E-17,0.000879500804048824,
0.00156989029765731),.UNSPECIFIED.);
#953=B_SPLINE_CURVE_WITH_KNOTS('',3,(#20670,#20671,#20672,#20673,#20674,
#20675,#20676,#20677,#20678,#20679),.UNSPECIFIED.,.F.,.F.,(4,2,2,2,4),(-0.260724943430608,
-0.199726493772825,-0.130391022195954,-0.0610665704087948,0.),
 .UNSPECIFIED.);
#954=B_SPLINE_CURVE_WITH_KNOTS('',3,(#20681,#20682,#20683,#20684,#20685,
#20686,#20687),.UNSPECIFIED.,.F.,.F.,(4,3,4),(2.90925827778347E-14,0.000871811007964718,
0.00160579165129899),.UNSPECIFIED.);
#955=B_SPLINE_CURVE_WITH_KNOTS('',3,(#20691,#20692,#20693,#20694,#20695,
#20696,#20697),.UNSPECIFIED.,.F.,.F.,(4,3,4),(4.35066434406066E-17,0.000879500804046061,
0.00156989029765632),.UNSPECIFIED.);
#956=B_SPLINE_CURVE_WITH_KNOTS('',3,(#20699,#20700,#20701,#20702,#20703,
#20704,#20705,#20706,#20707,#20708),.UNSPECIFIED.,.F.,.F.,(4,2,2,2,4),(-0.260724943430643,
-0.199726494015738,-0.130391022447992,-0.0610665706515827,0.),
 .UNSPECIFIED.);
#957=B_SPLINE_CURVE_WITH_KNOTS('',3,(#20710,#20711,#20712,#20713,#20714,
#20715,#20716),.UNSPECIFIED.,.F.,.F.,(4,3,4),(3.46944695195361E-18,0.000871811004271182,
0.00160579165132782),.UNSPECIFIED.);
#958=B_SPLINE_CURVE_WITH_KNOTS('',3,(#20720,#20721,#20722,#20723,#20724,
#20725,#20726),.UNSPECIFIED.,.F.,.F.,(4,3,4),(1.27770362542414E-17,0.000879500804024833,
0.00156989029765982),.UNSPECIFIED.);
#959=B_SPLINE_CURVE_WITH_KNOTS('',3,(#20728,#20729,#20730,#20731,#20732,
#20733,#20734,#20735,#20736,#20737),.UNSPECIFIED.,.F.,.F.,(4,2,2,2,4),(-0.260724943430692,
-0.199726493772888,-0.130391022196012,-0.0610665704088243,0.),
 .UNSPECIFIED.);
#960=B_SPLINE_CURVE_WITH_KNOTS('',3,(#20739,#20740,#20741,#20742,#20743,
#20744,#20745),.UNSPECIFIED.,.F.,.F.,(4,3,4),(2.91292484701896E-14,0.000871811007984886,
0.00160579165129793),.UNSPECIFIED.);
#961=B_SPLINE_CURVE_WITH_KNOTS('',3,(#20749,#20750,#20751,#20752,#20753,
#20754,#20755),.UNSPECIFIED.,.F.,.F.,(4,3,4),(1.25393031850254E-17,0.00087950080402042,
0.00156989029765787),.UNSPECIFIED.);
#962=B_SPLINE_CURVE_WITH_KNOTS('',3,(#20757,#20758,#20759,#20760,#20761,
#20762,#20763,#20764,#20765,#20766),.UNSPECIFIED.,.F.,.F.,(4,2,2,2,4),(-0.26072494343069,
-0.199726493772886,-0.130391022196038,-0.0610665704088844,0.),
 .UNSPECIFIED.);
#963=B_SPLINE_CURVE_WITH_KNOTS('',3,(#20768,#20769,#20770,#20771,#20772,
#20773,#20774),.UNSPECIFIED.,.F.,.F.,(4,3,4),(2.90945543471338E-14,0.000871811007981126,
0.00160579165129904),.UNSPECIFIED.);
#964=B_SPLINE_CURVE_WITH_KNOTS('',3,(#20778,#20779,#20780,#20781,#20782,
#20783,#20784),.UNSPECIFIED.,.F.,.F.,(4,3,4),(3.46944695195361E-18,0.000879500804016519,
0.00156989029766726),.UNSPECIFIED.);
#965=B_SPLINE_CURVE_WITH_KNOTS('',3,(#20786,#20787,#20788,#20789,#20790,
#20791,#20792,#20793,#20794,#20795),.UNSPECIFIED.,.F.,.F.,(4,2,2,2,4),(-0.260724943430721,
-0.199726493772798,-0.130391022196058,-0.0610665704090037,0.),
 .UNSPECIFIED.);
#966=B_SPLINE_CURVE_WITH_KNOTS('',3,(#20797,#20798,#20799,#20800,#20801,
#20802,#20803),.UNSPECIFIED.,.F.,.F.,(4,3,4),(2.91013228173329E-14,0.000871811007991177,
0.0016057916512899),.UNSPECIFIED.);
#967=B_SPLINE_CURVE_WITH_KNOTS('',3,(#20807,#20808,#20809,#20810,#20811,
#20812,#20813),.UNSPECIFIED.,.F.,.F.,(4,3,4),(2.11749985874298E-17,0.000879500804033151,
0.00156989029764894),.UNSPECIFIED.);
#968=B_SPLINE_CURVE_WITH_KNOTS('',3,(#20815,#20816,#20817,#20818,#20819,
#20820,#20821,#20822,#20823,#20824),.UNSPECIFIED.,.F.,.F.,(4,2,2,2,4),(-0.26072494343059,
-0.199726494015698,-0.130391022447996,-0.0610665706516228,0.),
 .UNSPECIFIED.);
#969=B_SPLINE_CURVE_WITH_KNOTS('',3,(#20826,#20827,#20828,#20829,#20830,
#20831,#20832),.UNSPECIFIED.,.F.,.F.,(4,3,4),(1.73472347597681E-18,0.000871811004245289,
0.00160579165133993),.UNSPECIFIED.);
#970=B_SPLINE_CURVE_WITH_KNOTS('',3,(#20836,#20837,#20838,#20839,#20840,
#20841,#20842),.UNSPECIFIED.,.F.,.F.,(4,3,4),(1.29814818157976E-17,0.000879500804017423,
0.00156989029766904),.UNSPECIFIED.);
#971=B_SPLINE_CURVE_WITH_KNOTS('',3,(#20844,#20845,#20846,#20847,#20848,
#20849,#20850,#20851,#20852,#20853),.UNSPECIFIED.,.F.,.F.,(4,2,2,2,4),(-0.260724943430682,
-0.199726493772798,-0.130391022196032,-0.0610665704089836,0.),
 .UNSPECIFIED.);
#972=B_SPLINE_CURVE_WITH_KNOTS('',3,(#20855,#20856,#20857,#20858,#20859,
#20860,#20861),.UNSPECIFIED.,.F.,.F.,(4,3,4),(2.91001867197953E-14,0.000871811007999078,
0.00160579165129162),.UNSPECIFIED.);
#973=B_SPLINE_CURVE_WITH_KNOTS('',3,(#20865,#20866,#20867,#20868,#20869,
#20870,#20871),.UNSPECIFIED.,.F.,.F.,(4,3,4),(3.00963274664804E-17,0.000879500804029671,
0.00156989029766195),.UNSPECIFIED.);
#974=B_SPLINE_CURVE_WITH_KNOTS('',3,(#20873,#20874,#20875,#20876,#20877,
#20878,#20879,#20880,#20881,#20882),.UNSPECIFIED.,.F.,.F.,(4,2,2,2,4),(-0.260724943430772,
-0.199726493772819,-0.130391022196083,-0.0610665704090635,0.),
 .UNSPECIFIED.);
#975=B_SPLINE_CURVE_WITH_KNOTS('',3,(#20884,#20885,#20886,#20887,#20888,
#20889,#20890),.UNSPECIFIED.,.F.,.F.,(4,3,4),(2.90982160104274E-14,0.000871811007979976,
0.00160579165129827),.UNSPECIFIED.);
#976=B_SPLINE_CURVE_WITH_KNOTS('',3,(#20894,#20895,#20896,#20897,#20898,
#20899,#20900),.UNSPECIFIED.,.F.,.F.,(4,3,4),(1.30968750346023E-17,0.000879500804031867,
0.00156989029765141),.UNSPECIFIED.);
#977=B_SPLINE_CURVE_WITH_KNOTS('',3,(#20902,#20903,#20904,#20905,#20906,
#20907,#20908,#20909,#20910,#20911),.UNSPECIFIED.,.F.,.F.,(4,2,2,2,4),(-0.260724943430687,
-0.199726493772781,-0.130391022196041,-0.0610665704090031,0.),
 .UNSPECIFIED.);
#978=B_SPLINE_CURVE_WITH_KNOTS('',3,(#20913,#20914,#20915,#20916,#20917,
#20918,#20919),.UNSPECIFIED.,.F.,.F.,(4,3,4),(2.91087637723392E-14,0.000871811007963812,
0.00160579165130534),.UNSPECIFIED.);
#979=B_SPLINE_CURVE_WITH_KNOTS('',3,(#20923,#20924,#20925,#20926,#20927,
#20928,#20929),.UNSPECIFIED.,.F.,.F.,(4,3,4),(1.74337551706054E-17,0.000879500804024546,
0.00156989029766136),.UNSPECIFIED.);
#980=B_SPLINE_CURVE_WITH_KNOTS('',3,(#20931,#20932,#20933,#20934,#20935,
#20936,#20937,#20938,#20939,#20940),.UNSPECIFIED.,.F.,.F.,(4,2,2,2,4),(-0.260724943430695,
-0.199726493772679,-0.130391022195957,-0.0610665704089199,0.),
 .UNSPECIFIED.);
#981=B_SPLINE_CURVE_WITH_KNOTS('',3,(#20942,#20943,#20944,#20945,#20946,
#20947,#20948),.UNSPECIFIED.,.F.,.F.,(4,3,4),(2.91042167107766E-14,0.000871811007980219,
0.00160579165129469),.UNSPECIFIED.);
#982=B_SPLINE_CURVE_WITH_KNOTS('',3,(#20952,#20953,#20954,#20955,#20956,
#20957,#20958),.UNSPECIFIED.,.F.,.F.,(4,3,4),(2.4532694666934E-17,0.000879500804036203,
0.00156989029764486),.UNSPECIFIED.);
#983=B_SPLINE_CURVE_WITH_KNOTS('',3,(#20960,#20961,#20962,#20963,#20964,
#20965,#20966,#20967,#20968,#20969),.UNSPECIFIED.,.F.,.F.,(4,2,2,2,4),(-0.260724943430608,
-0.199726493772553,-0.130391022195942,-0.0610665704090163,0.),
 .UNSPECIFIED.);
#984=B_SPLINE_CURVE_WITH_KNOTS('',3,(#20971,#20972,#20973,#20974,#20975,
#20976,#20977),.UNSPECIFIED.,.F.,.F.,(4,3,4),(2.91014911109026E-14,0.000871811007975891,
0.00160579165131238),.UNSPECIFIED.);
#985=B_SPLINE_CURVE_WITH_KNOTS('',3,(#20981,#20982,#20983,#20984,#20985,
#20986,#20987),.UNSPECIFIED.,.F.,.F.,(4,3,4),(1.35486234660355E-17,0.000879500804022474,
0.00156989029765048),.UNSPECIFIED.);
#986=B_SPLINE_CURVE_WITH_KNOTS('',3,(#20989,#20990,#20991,#20992,#20993,
#20994,#20995,#20996,#20997,#20998),.UNSPECIFIED.,.F.,.F.,(4,2,2,2,4),(-0.260724943430529,
-0.199726493772671,-0.130391022195944,-0.0610665704089295,0.),
 .UNSPECIFIED.);
#987=B_SPLINE_CURVE_WITH_KNOTS('',3,(#21000,#21001,#21002,#21003,#21004,
#21005,#21006),.UNSPECIFIED.,.F.,.F.,(4,3,4),(2.9101180116032E-14,0.000871811007967255,
0.00160579165130327),.UNSPECIFIED.);
#988=B_SPLINE_CURVE_WITH_KNOTS('',3,(#21010,#21011,#21012,#21013,#21014,
#21015,#21016),.UNSPECIFIED.,.F.,.F.,(4,3,4),(1.16368788433466E-17,0.000879500804019555,
0.00156989029765596),.UNSPECIFIED.);
#989=B_SPLINE_CURVE_WITH_KNOTS('',3,(#21018,#21019,#21020,#21021,#21022,
#21023,#21024,#21025,#21026,#21027),.UNSPECIFIED.,.F.,.F.,(4,2,2,2,4),(-0.260724943430678,
-0.199726493772776,-0.130391022196033,-0.0610665704089837,0.),
 .UNSPECIFIED.);
#990=B_SPLINE_CURVE_WITH_KNOTS('',3,(#21029,#21030,#21031,#21032,#21033,
#21034,#21035),.UNSPECIFIED.,.F.,.F.,(4,3,4),(2.91000394628375E-14,0.000871811007976233,
0.00160579165130128),.UNSPECIFIED.);
#991=B_SPLINE_CURVE_WITH_KNOTS('',3,(#21039,#21040,#21041,#21042,#21043,
#21044,#21045),.UNSPECIFIED.,.F.,.F.,(4,3,4),(1.9930455364338E-17,0.000879500804026383,
0.00156989029765913),.UNSPECIFIED.);
#992=B_SPLINE_CURVE_WITH_KNOTS('',3,(#21047,#21048,#21049,#21050,#21051,
#21052,#21053,#21054,#21055,#21056),.UNSPECIFIED.,.F.,.F.,(4,2,2,2,4),(-0.260520353691811,
-0.209093406725458,-0.154219975172592,-0.0839882141543201,-0.0483220958496221),
 .UNSPECIFIED.);
#993=B_SPLINE_CURVE_WITH_KNOTS('',3,(#21061,#21062,#21063,#21064,#21065,
#21066),.UNSPECIFIED.,.F.,.F.,(4,2,4),(-0.0483220958496221,-0.0407569430592836,
0.),.UNSPECIFIED.);
#994=B_SPLINE_CURVE_WITH_KNOTS('',3,(#21068,#21069,#21070,#21071,#21072,
#21073,#21074),.UNSPECIFIED.,.F.,.F.,(4,3,4),(2.90906258208131E-14,0.000871811007977714,
0.00160579165130056),.UNSPECIFIED.);
#995=B_SPLINE_CURVE_WITH_KNOTS('',3,(#21078,#21079,#21080,#21081,#21082,
#21083,#21084),.UNSPECIFIED.,.F.,.F.,(4,3,4),(2.22829265085925E-17,0.000879500804029387,
0.00156989029765885),.UNSPECIFIED.);
#996=B_SPLINE_CURVE_WITH_KNOTS('',3,(#21086,#21087,#21088,#21089,#21090,
#21091,#21092,#21093,#21094,#21095),.UNSPECIFIED.,.F.,.F.,(4,2,2,2,4),(-0.260724943430766,
-0.199726494015728,-0.130391022448065,-0.061066570651741,0.),
 .UNSPECIFIED.);
#997=B_SPLINE_CURVE_WITH_KNOTS('',3,(#21097,#21098,#21099,#21100,#21101,
#21102,#21103),.UNSPECIFIED.,.F.,.F.,(4,3,4),(3.5762240613455E-18,0.00087181100425516,
0.00160579165132772),.UNSPECIFIED.);
#998=B_SPLINE_CURVE_WITH_KNOTS('',3,(#21107,#21108,#21109,#21110,#21111,
#21112,#21113),.UNSPECIFIED.,.F.,.F.,(4,3,4),(1.96261557335472E-17,0.000879500804038629,
0.00156989029765915),.UNSPECIFIED.);
#999=B_SPLINE_CURVE_WITH_KNOTS('',3,(#21115,#21116,#21117,#21118,#21119,
#21120,#21121,#21122,#21123,#21124),.UNSPECIFIED.,.F.,.F.,(4,2,2,2,4),(-0.260724943430666,
-0.199726493772782,-0.130391022196017,-0.0610665704089714,0.),
 .UNSPECIFIED.);
#1000=B_SPLINE_CURVE_WITH_KNOTS('',3,(#21126,#21127,#21128,#21129,#21130,
#21131,#21132),.UNSPECIFIED.,.F.,.F.,(4,3,4),(2.91001126777664E-14,0.000871811007981504,
0.00160579165129883),.UNSPECIFIED.);
#1001=B_SPLINE_CURVE_WITH_KNOTS('',3,(#21136,#21137,#21138,#21139,#21140,
#21141,#21142),.UNSPECIFIED.,.F.,.F.,(4,3,4),(2.7318452618149E-17,0.000879500804037613,
0.00156989029765498),.UNSPECIFIED.);
#1002=B_SPLINE_CURVE_WITH_KNOTS('',3,(#21144,#21145,#21146,#21147,#21148,
#21149,#21150,#21151,#21152,#21153),.UNSPECIFIED.,.F.,.F.,(4,2,2,2,4),(-0.260724943430572,
-0.199726493772594,-0.13039102219594,-0.0610665704089772,0.),
 .UNSPECIFIED.);
#1003=B_SPLINE_CURVE_WITH_KNOTS('',3,(#21155,#21156,#21157,#21158,#21159,
#21160,#21161),.UNSPECIFIED.,.F.,.F.,(4,3,4),(2.91359063697315E-14,0.000871811007969042,
0.00160579165130329),.UNSPECIFIED.);
#1004=B_SPLINE_CURVE_WITH_KNOTS('',3,(#21165,#21166,#21167,#21168,#21169,
#21170,#21171),.UNSPECIFIED.,.F.,.F.,(4,3,4),(2.32737576866932E-17,0.000879500804023078,
0.00156989029766054),.UNSPECIFIED.);
#1005=B_SPLINE_CURVE_WITH_KNOTS('',3,(#21173,#21174,#21175,#21176,#21177,
#21178,#21179,#21180,#21181,#21182),.UNSPECIFIED.,.F.,.F.,(4,2,2,2,4),(-0.260724943430778,
-0.199726493772851,-0.130391022196053,-0.0610665704089545,0.),
 .UNSPECIFIED.);
#1006=B_SPLINE_CURVE_WITH_KNOTS('',3,(#21184,#21185,#21186,#21187,#21188,
#21189,#21190),.UNSPECIFIED.,.F.,.F.,(4,3,4),(2.91132655738402E-14,0.000871811007988041,
0.00160579165129781),.UNSPECIFIED.);
#1007=B_SPLINE_CURVE_WITH_KNOTS('',3,(#21194,#21195,#21196,#21197,#21198,
#21199,#21200),.UNSPECIFIED.,.F.,.F.,(4,3,4),(3.24073089410192E-17,0.000879500804029647,
0.00156989029765669),.UNSPECIFIED.);
#1008=B_SPLINE_CURVE_WITH_KNOTS('',3,(#21202,#21203,#21204,#21205,#21206,
#21207,#21208,#21209,#21210,#21211),.UNSPECIFIED.,.F.,.F.,(4,2,2,2,4),(-0.260724943430862,
-0.199726493772895,-0.130391022196119,-0.0610665704090545,0.),
 .UNSPECIFIED.);
#1009=B_SPLINE_CURVE_WITH_KNOTS('',3,(#21213,#21214,#21215,#21216,#21217,
#21218,#21219),.UNSPECIFIED.,.F.,.F.,(4,3,4),(2.91067438627834E-14,0.0008718110079958,
0.00160579165130139),.UNSPECIFIED.);
#1010=B_SPLINE_CURVE_WITH_KNOTS('',3,(#21223,#21224,#21225,#21226,#21227,
#21228,#21229),.UNSPECIFIED.,.F.,.F.,(4,3,4),(2.92855028701906E-17,0.000879500804033521,
0.00156989029764515),.UNSPECIFIED.);
#1011=B_SPLINE_CURVE_WITH_KNOTS('',3,(#21231,#21232,#21233,#21234,#21235,
#21236,#21237,#21238,#21239,#21240),.UNSPECIFIED.,.F.,.F.,(4,2,2,2,4),(-0.260724943430445,
-0.199726493772613,-0.130391022195896,-0.0610665704088579,0.),
 .UNSPECIFIED.);
#1012=B_SPLINE_CURVE_WITH_KNOTS('',3,(#21242,#21243,#21244,#21245,#21246,
#21247,#21248),.UNSPECIFIED.,.F.,.F.,(4,3,4),(2.91087637723392E-14,0.000871811007984256,
0.00160579165131312),.UNSPECIFIED.);
#1013=B_SPLINE_CURVE_WITH_KNOTS('',3,(#21252,#21253,#21254,#21255,#21256,
#21257,#21258),.UNSPECIFIED.,.F.,.F.,(4,3,4),(3.63878666146591E-17,0.000879500804036169,
0.00156989029767024),.UNSPECIFIED.);
#1014=B_SPLINE_CURVE_WITH_KNOTS('',3,(#21260,#21261,#21262,#21263,#21264,
#21265,#21266,#21267,#21268,#21269),.UNSPECIFIED.,.F.,.F.,(4,2,2,2,4),(-0.26072494343082,
-0.199726493772798,-0.130391022196048,-0.0610665704089677,0.),
 .UNSPECIFIED.);
#1015=B_SPLINE_CURVE_WITH_KNOTS('',3,(#21271,#21272,#21273,#21274,#21275,
#21276,#21277),.UNSPECIFIED.,.F.,.F.,(4,3,4),(2.91241109924099E-14,0.000871811007978442,
0.00160579165128969),.UNSPECIFIED.);
#1016=B_SPLINE_CURVE_WITH_KNOTS('',3,(#21281,#21282,#21283,#21284,#21285,
#21286,#21287),.UNSPECIFIED.,.F.,.F.,(4,3,4),(2.08166817117217E-17,0.000879500804019574,
0.00156989029766826),.UNSPECIFIED.);
#1017=B_SPLINE_CURVE_WITH_KNOTS('',3,(#21289,#21290,#21291,#21292,#21293,
#21294,#21295,#21296,#21297,#21298),.UNSPECIFIED.,.F.,.F.,(4,2,2,2,4),(-0.260724943430785,
-0.199726493772819,-0.130391022196044,-0.0610665704089591,0.),
 .UNSPECIFIED.);
#1018=B_SPLINE_CURVE_WITH_KNOTS('',3,(#21300,#21301,#21302,#21303,#21304,
#21305,#21306),.UNSPECIFIED.,.F.,.F.,(4,3,4),(2.91043716495764E-14,0.000871811007981064,
0.00160579165128749),.UNSPECIFIED.);
#1019=B_SPLINE_CURVE_WITH_KNOTS('',3,(#21310,#21311,#21312,#21313,#21314,
#21315,#21316),.UNSPECIFIED.,.F.,.F.,(4,3,4),(1.97026712507607E-17,0.000879500804023626,
0.00156989029766686),.UNSPECIFIED.);
#1020=B_SPLINE_CURVE_WITH_KNOTS('',3,(#21318,#21319,#21320,#21321,#21322,
#21323,#21324,#21325,#21326,#21327),.UNSPECIFIED.,.F.,.F.,(4,2,2,2,4),(-0.260724943430759,
-0.199726493772798,-0.130391022196069,-0.0610665704090458,0.),
 .UNSPECIFIED.);
#1021=B_SPLINE_CURVE_WITH_KNOTS('',3,(#21329,#21330,#21331,#21332,#21333,
#21334,#21335),.UNSPECIFIED.,.F.,.F.,(4,3,4),(2.90643704185478E-14,0.000871811007973552,
0.00160579165129078),.UNSPECIFIED.);
#1022=B_SPLINE_CURVE_WITH_KNOTS('',3,(#21339,#21340,#21341,#21342,#21343,
#21344,#21345),.UNSPECIFIED.,.F.,.F.,(4,3,4),(3.94435074910981E-17,0.000879500804033538,
0.00156989029765321),.UNSPECIFIED.);
#1023=B_SPLINE_CURVE_WITH_KNOTS('',3,(#21347,#21348,#21349,#21350,#21351,
#21352,#21353,#21354,#21355,#21356),.UNSPECIFIED.,.F.,.F.,(4,2,2,2,4),(-0.260724943430726,
-0.199726493772705,-0.130391022196008,-0.0610665704090159,0.),
 .UNSPECIFIED.);
#1024=B_SPLINE_CURVE_WITH_KNOTS('',3,(#21358,#21359,#21360,#21361,#21362,
#21363,#21364),.UNSPECIFIED.,.F.,.F.,(4,3,4),(2.90938207050466E-14,0.000871811007985816,
0.00160579165130088),.UNSPECIFIED.);
#1025=B_SPLINE_CURVE_WITH_KNOTS('',3,(#21368,#21369,#21370,#21371,#21372,
#21373,#21374),.UNSPECIFIED.,.F.,.F.,(4,3,4),(1.86885762303156E-17,0.000879500804024845,
0.00156989029765983),.UNSPECIFIED.);
#1026=B_SPLINE_CURVE_WITH_KNOTS('',3,(#21376,#21377,#21378,#21379,#21380,
#21381,#21382,#21383,#21384,#21385),.UNSPECIFIED.,.F.,.F.,(4,2,2,2,4),(-0.260724943430608,
-0.199726493772826,-0.130391022195969,-0.0610665704088119,0.),
 .UNSPECIFIED.);
#1027=B_SPLINE_CURVE_WITH_KNOTS('',3,(#21387,#21388,#21389,#21390,#21391,
#21392,#21393),.UNSPECIFIED.,.F.,.F.,(4,3,4),(2.91304865854723E-14,0.000871811007993082,
0.00160579165129793),.UNSPECIFIED.);
#1028=B_SPLINE_CURVE_WITH_KNOTS('',3,(#21397,#21398,#21399,#21400,#21401,
#21402,#21403),.UNSPECIFIED.,.F.,.F.,(4,3,4),(2.22829265085925E-17,0.000879500804025998,
0.00156989029765836),.UNSPECIFIED.);
#1029=B_SPLINE_CURVE_WITH_KNOTS('',3,(#21405,#21406,#21407,#21408,#21409,
#21410,#21411,#21412,#21413,#21414),.UNSPECIFIED.,.F.,.F.,(4,2,2,2,4),(-0.260724943430637,
-0.199726493772782,-0.130391022195983,-0.0610665704088931,0.),
 .UNSPECIFIED.);
#1030=B_SPLINE_CURVE_WITH_KNOTS('',3,(#21416,#21417,#21418,#21419,#21420,
#21421,#21422),.UNSPECIFIED.,.F.,.F.,(4,3,4),(2.91247662370936E-14,0.000871811007979228,
0.00160579165130031),.UNSPECIFIED.);
#1031=B_SPLINE_CURVE_WITH_KNOTS('',3,(#21426,#21427,#21428,#21429,#21430,
#21431,#21432),.UNSPECIFIED.,.F.,.F.,(4,3,4),(2.0888836804026E-17,0.00087950080401925,
0.00156989029766913),.UNSPECIFIED.);
#1032=B_SPLINE_CURVE_WITH_KNOTS('',3,(#21434,#21435,#21436,#21437,#21438,
#21439,#21440,#21441,#21442,#21443),.UNSPECIFIED.,.F.,.F.,(4,2,2,2,4),(-0.26072494343068,
-0.199726493772826,-0.13039102219598,-0.0610665704088353,0.),
 .UNSPECIFIED.);
#1033=B_SPLINE_CURVE_WITH_KNOTS('',3,(#21445,#21446,#21447,#21448,#21449,
#21450,#21451),.UNSPECIFIED.,.F.,.F.,(4,3,4),(2.91135465160192E-14,0.000871811007985186,
0.00160579165128965),.UNSPECIFIED.);
#1034=B_SPLINE_CURVE_WITH_KNOTS('',3,(#21455,#21456,#21457,#21458,#21459,
#21460,#21461),.UNSPECIFIED.,.F.,.F.,(4,3,4),(2.11749985874298E-17,0.000879500804028422,
0.00156989029765732),.UNSPECIFIED.);
#1035=B_SPLINE_CURVE_WITH_KNOTS('',3,(#21463,#21464,#21465,#21466,#21467,
#21468,#21469,#21470,#21471,#21472),.UNSPECIFIED.,.F.,.F.,(4,2,2,2,4),(-0.260724943430486,
-0.199726494015597,-0.130391022447942,-0.0610665706516372,0.),
 .UNSPECIFIED.);
#1036=B_SPLINE_CURVE_WITH_KNOTS('',3,(#21474,#21475,#21476,#21477,#21478,
#21479,#21480),.UNSPECIFIED.,.F.,.F.,(4,3,4),(0.,0.000871811004269854,0.00160579165133273),
 .UNSPECIFIED.);
#1037=B_SPLINE_CURVE_WITH_KNOTS('',3,(#21484,#21485,#21486,#21487,#21488,
#21489,#21490),.UNSPECIFIED.,.F.,.F.,(4,3,4),(3.0245937307082E-17,0.000879500804036986,
0.00156989029766962),.UNSPECIFIED.);
#1038=B_SPLINE_CURVE_WITH_KNOTS('',3,(#21492,#21493,#21494,#21495,#21496,
#21497,#21498,#21499,#21500,#21501),.UNSPECIFIED.,.F.,.F.,(4,2,2,2,4),(-0.260724943430712,
-0.19972649401573,-0.130391022448006,-0.061066570651615,0.),
 .UNSPECIFIED.);
#1039=B_SPLINE_CURVE_WITH_KNOTS('',3,(#21503,#21504,#21505,#21506,#21507,
#21508,#21509),.UNSPECIFIED.,.F.,.F.,(4,3,4),(9.34177181294034E-18,0.000871811004264771,
0.0016057916513195),.UNSPECIFIED.);
#1040=B_SPLINE_CURVE_WITH_KNOTS('',3,(#21513,#21514,#21515,#21516,#21517,
#21518,#21519),.UNSPECIFIED.,.F.,.F.,(4,3,4),(4.16333634234434E-17,0.000879500804025556,
0.00156989029766107),.UNSPECIFIED.);
#1041=B_SPLINE_CURVE_WITH_KNOTS('',3,(#21521,#21522,#21523,#21524,#21525,
#21526,#21527,#21528,#21529,#21530),.UNSPECIFIED.,.F.,.F.,(4,2,2,2,4),(-0.260724943430731,
-0.199726493772769,-0.130391022196028,-0.0610665704089995,0.),
 .UNSPECIFIED.);
#1042=B_SPLINE_CURVE_WITH_KNOTS('',3,(#21532,#21533,#21534,#21535,#21536,
#21537,#21538),.UNSPECIFIED.,.F.,.F.,(4,3,4),(2.9112405365365E-14,0.000871811007989186,
0.00160579165129583),.UNSPECIFIED.);
#1043=B_SPLINE_CURVE_WITH_KNOTS('',3,(#21542,#21543,#21544,#21545,#21546,
#21547,#21548),.UNSPECIFIED.,.F.,.F.,(4,3,4),(3.04442734473391E-17,0.000879500804017925,
0.00156989029765869),.UNSPECIFIED.);
#1044=B_SPLINE_CURVE_WITH_KNOTS('',3,(#21550,#21551,#21552,#21553,#21554,
#21555,#21556,#21557,#21558,#21559),.UNSPECIFIED.,.F.,.F.,(4,2,2,2,4),(-0.260724943430665,
-0.199726493772749,-0.130391022196018,-0.0610665704090143,0.),
 .UNSPECIFIED.);
#1045=B_SPLINE_CURVE_WITH_KNOTS('',3,(#21561,#21562,#21563,#21564,#21565,
#21566,#21567),.UNSPECIFIED.,.F.,.F.,(4,3,4),(2.9097154720412E-14,0.000871811007991494,
0.00160579165130179),.UNSPECIFIED.);
#1046=B_SPLINE_CURVE_WITH_KNOTS('',3,(#21571,#21572,#21573,#21574,#21575,
#21576,#21577),.UNSPECIFIED.,.F.,.F.,(4,3,4),(1.74337551706054E-17,0.000879500804021092,
0.00156989029765673),.UNSPECIFIED.);
#1047=B_SPLINE_CURVE_WITH_KNOTS('',3,(#21579,#21580,#21581,#21582,#21583,
#21584,#21585,#21586,#21587,#21588),.UNSPECIFIED.,.F.,.F.,(4,2,2,2,4),(-0.260724943430631,
-0.199726493772786,-0.130391022195963,-0.0610665704088755,0.),
 .UNSPECIFIED.);
#1048=B_SPLINE_CURVE_WITH_KNOTS('',3,(#21590,#21591,#21592,#21593,#21594,
#21595,#21596),.UNSPECIFIED.,.F.,.F.,(4,3,4),(2.90847295664599E-14,0.000871811007970203,
0.00160579165130329),.UNSPECIFIED.);
#1049=B_SPLINE_CURVE_WITH_KNOTS('',3,(#21600,#21601,#21602,#21603,#21604,
#21605,#21606),.UNSPECIFIED.,.F.,.F.,(4,3,4),(3.87895961444886E-17,0.000879500804034552,
0.00156989029765527),.UNSPECIFIED.);
#1050=B_SPLINE_CURVE_WITH_KNOTS('',3,(#21608,#21609,#21610,#21611,#21612,
#21613,#21614,#21615,#21616,#21617),.UNSPECIFIED.,.F.,.F.,(4,2,2,2,4),(-0.260724943430537,
-0.199726493772744,-0.130391022195923,-0.061066570408807,0.),
 .UNSPECIFIED.);
#1051=B_SPLINE_CURVE_WITH_KNOTS('',3,(#21619,#21620,#21621,#21622,#21623,
#21624,#21625),.UNSPECIFIED.,.F.,.F.,(4,3,4),(2.9092974958669E-14,0.000871811007970566,
0.00160579165130425),.UNSPECIFIED.);
#1052=B_SPLINE_CURVE_WITH_KNOTS('',3,(#21629,#21630,#21631,#21632,#21633,
#21634,#21635),.UNSPECIFIED.,.F.,.F.,(4,3,4),(2.57885184514585E-17,0.00087950080403597,
0.00156989029765865),.UNSPECIFIED.);
#1053=B_SPLINE_CURVE_WITH_KNOTS('',3,(#21637,#21638,#21639,#21640,#21641,
#21642,#21643,#21644,#21645,#21646),.UNSPECIFIED.,.F.,.F.,(4,2,2,2,4),(-0.260724943430618,
-0.199726493772736,-0.130391022195974,-0.0610665704089162,0.),
 .UNSPECIFIED.);
#1054=B_SPLINE_CURVE_WITH_KNOTS('',3,(#21648,#21649,#21650,#21651,#21652,
#21653,#21654),.UNSPECIFIED.,.F.,.F.,(4,3,4),(2.91294464430763E-14,0.000871811007972832,
0.00160579165129869),.UNSPECIFIED.);
#1055=B_SPLINE_CURVE_WITH_KNOTS('',3,(#21658,#21659,#21660,#21661,#21662,
#21663,#21664),.UNSPECIFIED.,.F.,.F.,(4,3,4),(2.32737576866932E-17,0.000879500804029127,
0.0015698902976571),.UNSPECIFIED.);
#1056=B_SPLINE_CURVE_WITH_KNOTS('',3,(#21666,#21667,#21668,#21669,#21670,
#21671,#21672,#21673,#21674,#21675),.UNSPECIFIED.,.F.,.F.,(4,2,2,2,4),(-0.260724943430665,
-0.199726493772715,-0.130391022195962,-0.0610665704089159,0.),
 .UNSPECIFIED.);
#1057=B_SPLINE_CURVE_WITH_KNOTS('',3,(#21677,#21678,#21679,#21680,#21681,
#21682,#21683),.UNSPECIFIED.,.F.,.F.,(4,3,4),(2.90901901300838E-14,0.000871811007981293,
0.00160579165130176),.UNSPECIFIED.);
#1058=B_SPLINE_CURVE_WITH_KNOTS('',3,(#21686,#21687,#21688,#21689,#21690,
#21691,#21692),.UNSPECIFIED.,.F.,.F.,(4,3,4),(1.75413055748779E-17,0.000879500804021358,
0.00156989029765893),.UNSPECIFIED.);
#1059=B_SPLINE_CURVE_WITH_KNOTS('',3,(#21694,#21695,#21696,#21697,#21698,
#21699),.UNSPECIFIED.,.F.,.F.,(4,2,4),(1.00000018525999E-6,0.161245973868135,
0.321302696423032),.UNSPECIFIED.);
#1060=B_SPLINE_CURVE_WITH_KNOTS('',3,(#21700,#21701,#21702,#21703,#21704,
#21705),.UNSPECIFIED.,.F.,.F.,(4,2,4),(1.00000020281465E-6,0.1667794805349,
0.332956960668741),.UNSPECIFIED.);
#1061=B_SPLINE_CURVE_WITH_KNOTS('',3,(#21707,#21708,#21709,#21710,#21711,
#21712),.UNSPECIFIED.,.F.,.F.,(4,2,4),(1.00000020232593E-6,0.166779480533119,
0.33295696066984),.UNSPECIFIED.);
#1062=B_SPLINE_CURVE_WITH_KNOTS('',3,(#21713,#21714,#21715,#21716,#21717,
#21718),.UNSPECIFIED.,.F.,.F.,(4,2,4),(1.00000018558043E-6,0.161245973866302,
0.321302696447619),.UNSPECIFIED.);
#1063=B_SPLINE_CURVE_WITH_KNOTS('',3,(#21720,#21721,#21722,#21723,#21724,
#21725),.UNSPECIFIED.,.F.,.F.,(4,2,4),(1.00000018541071E-6,0.161245467064344,
0.321302696404247),.UNSPECIFIED.);
#1064=B_SPLINE_CURVE_WITH_KNOTS('',3,(#21726,#21727,#21728,#21729,#21730,
#21731),.UNSPECIFIED.,.F.,.F.,(4,2,4),(1.00000020240854E-6,0.1667794805253,
0.332956960639582),.UNSPECIFIED.);
#1065=B_SPLINE_CURVE_WITH_KNOTS('',3,(#21733,#21734,#21735,#21736,#21737,
#21738),.UNSPECIFIED.,.F.,.F.,(4,2,4),(1.00000018516492E-6,0.161245973870214,
0.32130269640169),.UNSPECIFIED.);
#1066=B_SPLINE_CURVE_WITH_KNOTS('',3,(#21739,#21740,#21741,#21742,#21743,
#21744),.UNSPECIFIED.,.F.,.F.,(4,2,4),(1.00000020306044E-6,0.166779480520393,
0.332956960668093),.UNSPECIFIED.);
#1067=B_SPLINE_CURVE_WITH_KNOTS('',3,(#21746,#21747,#21748,#21749,#21750,
#21751),.UNSPECIFIED.,.F.,.F.,(4,2,4),(1.00000018495189E-6,0.161245467061803,
0.321302696480035),.UNSPECIFIED.);
#1068=B_SPLINE_CURVE_WITH_KNOTS('',3,(#21752,#21753,#21754,#21755,#21756,
#21757),.UNSPECIFIED.,.F.,.F.,(4,2,4),(1.00000020291508E-6,0.166779480527622,
0.332956960694064),.UNSPECIFIED.);
#1069=B_SPLINE_CURVE_WITH_KNOTS('',3,(#21759,#21760,#21761,#21762,#21763,
#21764),.UNSPECIFIED.,.F.,.F.,(4,2,4),(1.00000018524296E-6,0.161245467067315,
0.321302696528087),.UNSPECIFIED.);
#1070=B_SPLINE_CURVE_WITH_KNOTS('',3,(#21765,#21766,#21767,#21768,#21769,
#21770),.UNSPECIFIED.,.F.,.F.,(4,2,4),(1.00000020251295E-6,0.166779480532976,
0.332956960702249),.UNSPECIFIED.);
#1071=B_SPLINE_CURVE_WITH_KNOTS('',3,(#21772,#21773,#21774,#21775,#21776,
#21777),.UNSPECIFIED.,.F.,.F.,(4,2,4),(1.00000018551213E-6,0.161245467070566,
0.321302696524444),.UNSPECIFIED.);
#1072=B_SPLINE_CURVE_WITH_KNOTS('',3,(#21778,#21779,#21780,#21781,#21782,
#21783),.UNSPECIFIED.,.F.,.F.,(4,2,4),(1.00000020265717E-6,0.166779480531078,
0.332956960668084),.UNSPECIFIED.);
#1073=B_SPLINE_CURVE_WITH_KNOTS('',3,(#21785,#21786,#21787,#21788,#21789,
#21790),.UNSPECIFIED.,.F.,.F.,(4,2,4),(1.00000018518735E-6,0.161245467061048,
0.321302696421221),.UNSPECIFIED.);
#1074=B_SPLINE_CURVE_WITH_KNOTS('',3,(#21791,#21792,#21793,#21794,#21795,
#21796),.UNSPECIFIED.,.F.,.F.,(4,2,4),(1.000000202362E-6,0.166779480540548,
0.332956960686337),.UNSPECIFIED.);
#1075=B_SPLINE_CURVE_WITH_KNOTS('',3,(#21798,#21799,#21800,#21801,#21802,
#21803),.UNSPECIFIED.,.F.,.F.,(4,2,4),(1.00000018537216E-6,0.161245973869415,
0.321302696413987),.UNSPECIFIED.);
#1076=B_SPLINE_CURVE_WITH_KNOTS('',3,(#21804,#21805,#21806,#21807,#21808,
#21809),.UNSPECIFIED.,.F.,.F.,(4,2,4),(1.00000020298589E-6,0.166779480532959,
0.332956960659601),.UNSPECIFIED.);
#1077=B_SPLINE_CURVE_WITH_KNOTS('',3,(#21811,#21812,#21813,#21814,#21815,
#21816),.UNSPECIFIED.,.F.,.F.,(4,2,4),(1.00000018494672E-6,0.161245973865759,
0.321302696389016),.UNSPECIFIED.);
#1078=B_SPLINE_CURVE_WITH_KNOTS('',3,(#21817,#21818,#21819,#21820,#21821,
#21822),.UNSPECIFIED.,.F.,.F.,(4,2,4),(1.00000020269192E-6,0.166779480525868,
0.332956960672747),.UNSPECIFIED.);
#1079=B_SPLINE_CURVE_WITH_KNOTS('',3,(#21824,#21825,#21826,#21827,#21828,
#21829),.UNSPECIFIED.,.F.,.F.,(4,2,4),(1.00000018523224E-6,0.161245467065664,
0.321302696484184),.UNSPECIFIED.);
#1080=B_SPLINE_CURVE_WITH_KNOTS('',3,(#21830,#21831,#21832,#21833,#21834,
#21835),.UNSPECIFIED.,.F.,.F.,(4,2,4),(1.00000020265587E-6,0.166779480529505,
0.332956960668596),.UNSPECIFIED.);
#1081=B_SPLINE_CURVE_WITH_KNOTS('',3,(#21837,#21838,#21839,#21840,#21841,
#21842),.UNSPECIFIED.,.F.,.F.,(4,2,4),(1.00000018523152E-6,0.161245973866936,
0.321302696434055),.UNSPECIFIED.);
#1082=B_SPLINE_CURVE_WITH_KNOTS('',3,(#21843,#21844,#21845,#21846,#21847,
#21848),.UNSPECIFIED.,.F.,.F.,(4,2,4),(1.00000020282499E-6,0.16677948053055,
0.332956960655279),.UNSPECIFIED.);
#1083=B_SPLINE_CURVE_WITH_KNOTS('',3,(#21850,#21851,#21852,#21853,#21854,
#21855),.UNSPECIFIED.,.F.,.F.,(4,2,4),(1.00000018488197E-6,0.161245467060642,
0.321302696386487),.UNSPECIFIED.);
#1084=B_SPLINE_CURVE_WITH_KNOTS('',3,(#21856,#21857,#21858,#21859,#21860,
#21861),.UNSPECIFIED.,.F.,.F.,(4,2,4),(1.00000020310365E-6,0.16677948052756,
0.332956960677708),.UNSPECIFIED.);
#1085=B_SPLINE_CURVE_WITH_KNOTS('',3,(#21863,#21864,#21865,#21866,#21867,
#21868),.UNSPECIFIED.,.F.,.F.,(4,2,4),(1.00000018517987E-6,0.161245973870067,
0.321302696479206),.UNSPECIFIED.);
#1086=B_SPLINE_CURVE_WITH_KNOTS('',3,(#21869,#21870,#21871,#21872,#21873,
#21874),.UNSPECIFIED.,.F.,.F.,(4,2,4),(1.00000020285339E-6,0.166779480523092,
0.332956960656032),.UNSPECIFIED.);
#1087=B_SPLINE_CURVE_WITH_KNOTS('',3,(#21876,#21877,#21878,#21879,#21880,
#21881),.UNSPECIFIED.,.F.,.F.,(4,2,4),(1.00000018502563E-6,0.161245467059883,
0.321302696428097),.UNSPECIFIED.);
#1088=B_SPLINE_CURVE_WITH_KNOTS('',3,(#21882,#21883,#21884,#21885,#21886,
#21887),.UNSPECIFIED.,.F.,.F.,(4,2,4),(1.00000020277303E-6,0.166779480528052,
0.33295696065521),.UNSPECIFIED.);
#1089=B_SPLINE_CURVE_WITH_KNOTS('',3,(#21889,#21890,#21891,#21892,#21893,
#21894),.UNSPECIFIED.,.F.,.F.,(4,2,4),(1.00000018537403E-6,0.161245467061688,
0.321302696397048),.UNSPECIFIED.);
#1090=B_SPLINE_CURVE_WITH_KNOTS('',3,(#21895,#21896,#21897,#21898,#21899,
#21900),.UNSPECIFIED.,.F.,.F.,(4,2,4),(1.00000020322115E-6,0.166779480526764,
0.332956960619472),.UNSPECIFIED.);
#1091=B_SPLINE_CURVE_WITH_KNOTS('',3,(#21902,#21903,#21904,#21905,#21906,
#21907),.UNSPECIFIED.,.F.,.F.,(4,2,4),(1.00000018531336E-6,0.161245467045064,
0.321302696266755),.UNSPECIFIED.);
#1092=B_SPLINE_CURVE_WITH_KNOTS('',3,(#21908,#21909,#21910,#21911,#21912,
#21913),.UNSPECIFIED.,.F.,.F.,(4,2,4),(1.00000020262015E-6,0.166779480521345,
0.332956960659132),.UNSPECIFIED.);
#1093=B_SPLINE_CURVE_WITH_KNOTS('',3,(#21915,#21916,#21917,#21918,#21919,
#21920),.UNSPECIFIED.,.F.,.F.,(4,2,4),(1.00000018504582E-6,0.161245467060812,
0.321302696456924),.UNSPECIFIED.);
#1094=B_SPLINE_CURVE_WITH_KNOTS('',3,(#21921,#21922,#21923,#21924,#21925,
#21926),.UNSPECIFIED.,.F.,.F.,(4,2,4),(1.00000020282842E-6,0.166779480527225,
0.332956960704414),.UNSPECIFIED.);
#1095=B_SPLINE_CURVE_WITH_KNOTS('',3,(#21928,#21929,#21930,#21931,#21932,
#21933),.UNSPECIFIED.,.F.,.F.,(4,2,4),(1.00000018543154E-6,0.161245973871395,
0.321302696554539),.UNSPECIFIED.);
#1096=B_SPLINE_CURVE_WITH_KNOTS('',3,(#21934,#21935,#21936,#21937,#21938,
#21939),.UNSPECIFIED.,.F.,.F.,(4,2,4),(1.00000020267848E-6,0.166779480528834,
0.332956960646251),.UNSPECIFIED.);
#1097=B_SPLINE_CURVE_WITH_KNOTS('',3,(#21941,#21942,#21943,#21944,#21945,
#21946),.UNSPECIFIED.,.F.,.F.,(4,2,4),(1.00000018528204E-6,0.161245973862908,
0.321302696370201),.UNSPECIFIED.);
#1098=B_SPLINE_CURVE_WITH_KNOTS('',3,(#21947,#21948,#21949,#21950,#21951,
#21952),.UNSPECIFIED.,.F.,.F.,(4,2,4),(1.00000020243982E-6,0.166779480529185,
0.332956960704068),.UNSPECIFIED.);
#1099=B_SPLINE_CURVE_WITH_KNOTS('',3,(#21954,#21955,#21956,#21957,#21958,
#21959),.UNSPECIFIED.,.F.,.F.,(4,2,4),(1.0000001851793E-6,0.161245467065769,
0.32130269653859),.UNSPECIFIED.);
#1100=B_SPLINE_CURVE_WITH_KNOTS('',3,(#21960,#21961,#21962,#21963,#21964,
#21965),.UNSPECIFIED.,.F.,.F.,(4,2,4),(1.00000020281741E-6,0.166779480531347,
0.33295696066664),.UNSPECIFIED.);
#1101=B_SPLINE_CURVE_WITH_KNOTS('',3,(#21967,#21968,#21969,#21970,#21971,
#21972),.UNSPECIFIED.,.F.,.F.,(4,2,4),(1.00000018530067E-6,0.161245973867389,
0.321302696417749),.UNSPECIFIED.);
#1102=B_SPLINE_CURVE_WITH_KNOTS('',3,(#21973,#21974,#21975,#21976,#21977,
#21978),.UNSPECIFIED.,.F.,.F.,(4,2,4),(1.00000020264041E-6,0.166779480527634,
0.332956960670351),.UNSPECIFIED.);
#1103=B_SPLINE_CURVE_WITH_KNOTS('',3,(#21980,#21981,#21982,#21983,#21984,
#21985),.UNSPECIFIED.,.F.,.F.,(4,2,4),(1.00000018506015E-6,0.161245973866292,
0.321302696447615),.UNSPECIFIED.);
#1104=B_SPLINE_CURVE_WITH_KNOTS('',3,(#21986,#21987,#21988,#21989,#21990,
#21991),.UNSPECIFIED.,.F.,.F.,(4,2,4),(1.00000020278924E-6,0.166779480531265,
0.332956960653417),.UNSPECIFIED.);
#1105=B_SPLINE_CURVE_WITH_KNOTS('',3,(#21993,#21994,#21995,#21996,#21997,
#21998),.UNSPECIFIED.,.F.,.F.,(4,2,4),(1.00000018471263E-6,0.161245973865716,
0.321302696384943),.UNSPECIFIED.);
#1106=B_SPLINE_CURVE_WITH_KNOTS('',3,(#21999,#22000,#22001,#22002,#22003,
#22004),.UNSPECIFIED.,.F.,.F.,(4,2,4),(1.00000020287686E-6,0.166779480530013,
0.33295696070179),.UNSPECIFIED.);
#1107=B_SPLINE_CURVE_WITH_KNOTS('',3,(#22006,#22007,#22008,#22009,#22010,
#22011),.UNSPECIFIED.,.F.,.F.,(4,2,4),(1.00000018567777E-6,0.161245467067852,
0.321302696531001),.UNSPECIFIED.);
#1108=B_SPLINE_CURVE_WITH_KNOTS('',3,(#22012,#22013,#22014,#22015,#22016,
#22017),.UNSPECIFIED.,.F.,.F.,(4,2,4),(1.00000020307531E-6,0.166779480520602,
0.332956960698483),.UNSPECIFIED.);
#1109=B_SPLINE_CURVE_WITH_KNOTS('',3,(#22019,#22020,#22021,#22022,#22023,
#22024),.UNSPECIFIED.,.F.,.F.,(4,2,4),(1.00000018514608E-6,0.161245467067323,
0.321302696582733),.UNSPECIFIED.);
#1110=B_SPLINE_CURVE_WITH_KNOTS('',3,(#22025,#22026,#22027,#22028,#22029,
#22030),.UNSPECIFIED.,.F.,.F.,(4,2,4),(1.00000020271264E-6,0.166779480532087,
0.33295696071809),.UNSPECIFIED.);
#1111=B_SPLINE_CURVE_WITH_KNOTS('',3,(#22032,#22033,#22034,#22035,#22036,
#22037),.UNSPECIFIED.,.F.,.F.,(4,2,4),(1.00000018490616E-6,0.161245467070947,
0.32130269657138),.UNSPECIFIED.);
#1112=B_SPLINE_CURVE_WITH_KNOTS('',3,(#22038,#22039,#22040,#22041,#22042,
#22043),.UNSPECIFIED.,.F.,.F.,(4,2,4),(1.00000020260949E-6,0.166779480540914,
0.332956960617602),.UNSPECIFIED.);
#1113=B_SPLINE_CURVE_WITH_KNOTS('',3,(#22045,#22046,#22047,#22048,#22049,
#22050),.UNSPECIFIED.,.F.,.F.,(4,2,4),(1.00000018495762E-6,0.161245973857737,
0.321302696209486),.UNSPECIFIED.);
#1114=B_SPLINE_CURVE_WITH_KNOTS('',3,(#22051,#22052,#22053,#22054,#22055,
#22056),.UNSPECIFIED.,.F.,.F.,(4,2,4),(1.00000020240665E-6,0.166779480518083,
0.33295696063765),.UNSPECIFIED.);
#1115=B_SPLINE_CURVE_WITH_KNOTS('',3,(#22058,#22059,#22060,#22061,#22062,
#22063),.UNSPECIFIED.,.F.,.F.,(4,2,4),(1.00000018539525E-6,0.161245467056979,
0.3213026964032),.UNSPECIFIED.);
#1116=B_SPLINE_CURVE_WITH_KNOTS('',3,(#22064,#22065,#22066,#22067,#22068,
#22069),.UNSPECIFIED.,.F.,.F.,(4,2,4),(1.00000020243603E-6,0.166779480530758,
0.332956960667656),.UNSPECIFIED.);
#1117=B_SPLINE_CURVE_WITH_KNOTS('',3,(#22071,#22072,#22073,#22074,#22075,
#22076),.UNSPECIFIED.,.F.,.F.,(4,2,4),(1.00000018564707E-6,0.161245973864463,
0.321302696409748),.UNSPECIFIED.);
#1118=B_SPLINE_CURVE_WITH_KNOTS('',3,(#22077,#22078,#22079,#22080,#22081,
#22082),.UNSPECIFIED.,.F.,.F.,(4,2,4),(1.00000020289556E-6,0.166779480530644,
0.332956960665992),.UNSPECIFIED.);
#1119=B_SPLINE_CURVE_WITH_KNOTS('',3,(#22084,#22085,#22086,#22087,#22088,
#22089),.UNSPECIFIED.,.F.,.F.,(4,2,4),(1.00000018538887E-6,0.161245467065029,
0.321302696435402),.UNSPECIFIED.);
#1120=B_SPLINE_CURVE_WITH_KNOTS('',3,(#22090,#22091,#22092,#22093,#22094,
#22095),.UNSPECIFIED.,.F.,.F.,(4,2,4),(1.00000020280345E-6,0.166779480528368,
0.332956960671687),.UNSPECIFIED.);
#1121=B_SPLINE_CURVE_WITH_KNOTS('',3,(#22097,#22098,#22099,#22100,#22101,
#22102),.UNSPECIFIED.,.F.,.F.,(4,2,4),(1.00000018531322E-6,0.16124597386755,
0.32130269645182),.UNSPECIFIED.);
#1122=B_SPLINE_CURVE_WITH_KNOTS('',3,(#22103,#22104,#22105,#22106,#22107,
#22108),.UNSPECIFIED.,.F.,.F.,(4,2,4),(1.00000020245141E-6,0.166779480529231,
0.332956960669946),.UNSPECIFIED.);
#1123=B_SPLINE_CURVE_WITH_KNOTS('',3,(#22110,#22111,#22112,#22113,#22114,
#22115),.UNSPECIFIED.,.F.,.F.,(4,2,4),(1.00000018554594E-6,0.16124546706305,
0.321302696441769),.UNSPECIFIED.);
#1124=B_SPLINE_CURVE_WITH_KNOTS('',3,(#22116,#22117,#22118,#22119,#22120,
#22121),.UNSPECIFIED.,.F.,.F.,(4,2,4),(1.00000020288612E-6,0.166779480527922,
0.332956960667366),.UNSPECIFIED.);
#1125=B_SPLINE_CURVE_WITH_KNOTS('',3,(#22123,#22124,#22125,#22126,#22127,
#22128),.UNSPECIFIED.,.F.,.F.,(4,2,4),(1.00000018525775E-6,0.161245973865254,
0.32130269643526),.UNSPECIFIED.);
#1126=B_SPLINE_CURVE_WITH_KNOTS('',3,(#22129,#22130,#22131,#22132,#22133,
#22134),.UNSPECIFIED.,.F.,.F.,(4,2,4),(1.00000020267844E-6,0.166779480525132,
0.332956960648716),.UNSPECIFIED.);
#1127=B_SPLINE_CURVE_WITH_KNOTS('',3,(#22136,#22137,#22138,#22139,#22140,
#22141),.UNSPECIFIED.,.F.,.F.,(4,2,4),(1.00000018542923E-6,0.161245467060377,
0.321302696403438),.UNSPECIFIED.);
#1128=B_SPLINE_CURVE_WITH_KNOTS('',3,(#22142,#22143,#22144,#22145,#22146,
#22147),.UNSPECIFIED.,.F.,.F.,(4,2,4),(1.00000020266136E-6,0.166779480530653,
0.332956960655275),.UNSPECIFIED.);
#1129=B_SPLINE_CURVE_WITH_KNOTS('',3,(#22149,#22150,#22151,#22152,#22153,
#22154),.UNSPECIFIED.,.F.,.F.,(4,2,4),(1.00000018510516E-6,0.161245973869074,
0.321302696406845),.UNSPECIFIED.);
#1130=B_SPLINE_CURVE_WITH_KNOTS('',3,(#22155,#22156,#22157,#22158,#22159,
#22160),.UNSPECIFIED.,.F.,.F.,(4,2,4),(1.00000020266632E-6,0.166779480533638,
0.332956960627681),.UNSPECIFIED.);
#1131=B_SPLINE_CURVE_WITH_KNOTS('',3,(#22162,#22163,#22164,#22165,#22166,
#22167),.UNSPECIFIED.,.F.,.F.,(4,2,4),(1.00000018510568E-6,0.161245973864822,
0.321302696292674),.UNSPECIFIED.);
#1132=B_SPLINE_CURVE_WITH_KNOTS('',3,(#22168,#22169,#22170,#22171,#22172,
#22173),.UNSPECIFIED.,.F.,.F.,(4,2,4),(1.00000020272525E-6,0.166779480521084,
0.332956960672202),.UNSPECIFIED.);
#1133=B_SPLINE_CURVE_WITH_KNOTS('',3,(#22175,#22176,#22177,#22178,#22179,
#22180),.UNSPECIFIED.,.F.,.F.,(4,2,4),(1.00000018522469E-6,0.161245467066401,
0.321302696507321),.UNSPECIFIED.);
#1134=B_SPLINE_CURVE_WITH_KNOTS('',3,(#22181,#22182,#22183,#22184,#22185,
#22186),.UNSPECIFIED.,.F.,.F.,(4,2,4),(1.0000002026673E-6,0.166779480534649,
0.332956960655979),.UNSPECIFIED.);
#1135=B_SPLINE_CURVE_WITH_KNOTS('',3,(#22188,#22189,#22190,#22191,#22192,
#22193),.UNSPECIFIED.,.F.,.F.,(4,2,4),(1.00000018545856E-6,0.16124546705897,
0.321302696360171),.UNSPECIFIED.);
#1136=B_SPLINE_CURVE_WITH_KNOTS('',3,(#22194,#22195,#22196,#22197,#22198,
#22199),.UNSPECIFIED.,.F.,.F.,(4,2,4),(1.00000020277335E-6,0.166779480534565,
0.332956960695636),.UNSPECIFIED.);
#1137=B_SPLINE_CURVE_WITH_KNOTS('',3,(#22201,#22202,#22203,#22204,#22205,
#22206),.UNSPECIFIED.,.F.,.F.,(4,2,4),(1.00000018536716E-6,0.161245467067694,
0.321302696478807),.UNSPECIFIED.);
#1138=B_SPLINE_CURVE_WITH_KNOTS('',3,(#22207,#22208,#22209,#22210,#22211,
#22212),.UNSPECIFIED.,.F.,.F.,(4,2,4),(1.00000020264012E-6,0.166779480514383,
0.332956960670406),.UNSPECIFIED.);
#1139=B_SPLINE_CURVE_WITH_KNOTS('',3,(#22214,#22215,#22216,#22217,#22218,
#22219),.UNSPECIFIED.,.F.,.F.,(4,2,4),(1.00000018542659E-6,0.161245973863339,
0.321302696520851),.UNSPECIFIED.);
#1140=B_SPLINE_CURVE_WITH_KNOTS('',3,(#22220,#22221,#22222,#22223,#22224,
#22225),.UNSPECIFIED.,.F.,.F.,(4,2,4),(1.000000202736E-6,0.166779480527173,
0.332956960649766),.UNSPECIFIED.);
#1141=B_SPLINE_CURVE_WITH_KNOTS('',3,(#22227,#22228,#22229,#22230,#22231,
#22232),.UNSPECIFIED.,.F.,.F.,(4,2,4),(1.00000018528858E-6,0.161245467063617,
0.321302696399603),.UNSPECIFIED.);
#1142=B_SPLINE_CURVE_WITH_KNOTS('',3,(#22233,#22234,#22235,#22236,#22237,
#22238),.UNSPECIFIED.,.F.,.F.,(4,2,4),(1.00000020289104E-6,0.16677948052314,
0.332956960694236),.UNSPECIFIED.);
#1143=B_SPLINE_CURVE_WITH_KNOTS('',3,(#22240,#22241,#22242,#22243,#22244,
#22245),.UNSPECIFIED.,.F.,.F.,(4,2,4),(1.00000018486152E-6,0.161245467066123,
0.321302696553676),.UNSPECIFIED.);
#1144=B_SPLINE_CURVE_WITH_KNOTS('',3,(#22246,#22247,#22248,#22249,#22250,
#22251),.UNSPECIFIED.,.F.,.F.,(4,2,4),(1.00000020272568E-6,0.166779480527199,
0.332956960661804),.UNSPECIFIED.);
#1145=B_SPLINE_CURVE_WITH_KNOTS('',3,(#22253,#22254,#22255,#22256,#22257,
#22258),.UNSPECIFIED.,.F.,.F.,(4,2,4),(1.00000018559864E-6,0.161245973866835,
0.321302696434928),.UNSPECIFIED.);
#1146=B_SPLINE_CURVE_WITH_KNOTS('',3,(#22259,#22260,#22261,#22262,#22263,
#22264),.UNSPECIFIED.,.F.,.F.,(4,2,4),(1.00000020252041E-6,0.166779480527667,
0.332956960670414),.UNSPECIFIED.);
#1147=B_SPLINE_CURVE_WITH_KNOTS('',3,(#22266,#22267,#22268,#22269,#22270,
#22271),.UNSPECIFIED.,.F.,.F.,(4,2,4),(1.00000022065418E-6,0.167102971345719,
0.334149753299976),.UNSPECIFIED.);
#1148=B_SPLINE_CURVE_WITH_KNOTS('',3,(#22272,#22273,#22274,#22275,#22276,
#22277),.UNSPECIFIED.,.F.,.F.,(4,2,4),(1.00000012092585E-6,0.161160399905657,
0.32316760723809),.UNSPECIFIED.);
#1149=B_SPLINE_CURVE_WITH_KNOTS('',3,(#22279,#22280,#22281,#22282,#22283,
#22284),.UNSPECIFIED.,.F.,.F.,(4,2,4),(1.00000012028406E-6,0.161160399904698,
0.323167607237289),.UNSPECIFIED.);
#1150=B_SPLINE_CURVE_WITH_KNOTS('',3,(#22285,#22286,#22287,#22288,#22289,
#22290),.UNSPECIFIED.,.F.,.F.,(4,2,4),(1.00000022034966E-6,0.1671029713458,
0.334149753300162),.UNSPECIFIED.);
#1151=B_SPLINE_CURVE_WITH_KNOTS('',3,(#22292,#22293,#22294,#22295,#22296,
#22297),.UNSPECIFIED.,.F.,.F.,(4,2,4),(1.00000012065005E-6,0.161160399904619,
0.323167607236669),.UNSPECIFIED.);
#1152=B_SPLINE_CURVE_WITH_KNOTS('',3,(#22298,#22299,#22300,#22301,#22302,
#22303),.UNSPECIFIED.,.F.,.F.,(4,2,4),(1.00000022013381E-6,0.167102971345785,
0.334149753300176),.UNSPECIFIED.);
#1153=B_SPLINE_CURVE_WITH_KNOTS('',3,(#22305,#22306,#22307,#22308,#22309,
#22310),.UNSPECIFIED.,.F.,.F.,(4,2,4),(1.00000012096186E-6,0.161160399904608,
0.323167607236878),.UNSPECIFIED.);
#1154=B_SPLINE_CURVE_WITH_KNOTS('',3,(#22311,#22312,#22313,#22314,#22315,
#22316),.UNSPECIFIED.,.F.,.F.,(4,2,4),(1.00000022094295E-6,0.167102971345706,
0.334149753300038),.UNSPECIFIED.);
#1155=B_SPLINE_CURVE_WITH_KNOTS('',3,(#22318,#22319,#22320,#22321,#22322,
#22323),.UNSPECIFIED.,.F.,.F.,(4,2,4),(1.00000012019619E-6,0.161160399904656,
0.323167607236991),.UNSPECIFIED.);
#1156=B_SPLINE_CURVE_WITH_KNOTS('',3,(#22324,#22325,#22326,#22327,#22328,
#22329),.UNSPECIFIED.,.F.,.F.,(4,2,4),(1.00000022083162E-6,0.167102971345771,
0.334149753300189),.UNSPECIFIED.);
#1157=B_SPLINE_CURVE_WITH_KNOTS('',3,(#22331,#22332,#22333,#22334,#22335,
#22336),.UNSPECIFIED.,.F.,.F.,(4,2,4),(1.00000012046609E-6,0.16115988960677,
0.323167607237021),.UNSPECIFIED.);
#1158=B_SPLINE_CURVE_WITH_KNOTS('',3,(#22337,#22338,#22339,#22340,#22341,
#22342),.UNSPECIFIED.,.F.,.F.,(4,2,4),(1.00000022058697E-6,0.1671029713457,
0.334149753299905),.UNSPECIFIED.);
#1159=B_SPLINE_CURVE_WITH_KNOTS('',3,(#22344,#22345,#22346,#22347,#22348,
#22349),.UNSPECIFIED.,.F.,.F.,(4,2,4),(1.00000012068149E-6,0.161159889606763,
0.323167607237227),.UNSPECIFIED.);
#1160=B_SPLINE_CURVE_WITH_KNOTS('',3,(#22350,#22351,#22352,#22353,#22354,
#22355),.UNSPECIFIED.,.F.,.F.,(4,2,4),(1.00000022093697E-6,0.167102971345751,
0.334149753300017),.UNSPECIFIED.);
#1161=B_SPLINE_CURVE_WITH_KNOTS('',3,(#22357,#22358,#22359,#22360,#22361,
#22362),.UNSPECIFIED.,.F.,.F.,(4,2,4),(1.00000012055824E-6,0.161160399904627,
0.323167607236808),.UNSPECIFIED.);
#1162=B_SPLINE_CURVE_WITH_KNOTS('',3,(#22363,#22364,#22365,#22366,#22367,
#22368),.UNSPECIFIED.,.F.,.F.,(4,2,4),(1.00000022101565E-6,0.167102971345646,
0.334149753299828),.UNSPECIFIED.);
#1163=B_SPLINE_CURVE_WITH_KNOTS('',3,(#22370,#22371,#22372,#22373,#22374,
#22375),.UNSPECIFIED.,.F.,.F.,(4,2,4),(1.00000012064667E-6,0.16116039990467,
0.323167607237047),.UNSPECIFIED.);
#1164=B_SPLINE_CURVE_WITH_KNOTS('',3,(#22376,#22377,#22378,#22379,#22380,
#22381),.UNSPECIFIED.,.F.,.F.,(4,2,4),(1.00000022025054E-6,0.16710297134573,
0.334149753300021),.UNSPECIFIED.);
#1165=B_SPLINE_CURVE_WITH_KNOTS('',3,(#22383,#22384,#22385,#22386,#22387,
#22388),.UNSPECIFIED.,.F.,.F.,(4,2,4),(1.00000012080846E-6,0.161160399904661,
0.323167607236932),.UNSPECIFIED.);
#1166=B_SPLINE_CURVE_WITH_KNOTS('',3,(#22389,#22390,#22391,#22392,#22393,
#22394),.UNSPECIFIED.,.F.,.F.,(4,2,4),(1.00000022119352E-6,0.167102971345721,
0.334149753299959),.UNSPECIFIED.);
#1167=B_SPLINE_CURVE_WITH_KNOTS('',3,(#22396,#22397,#22398,#22399,#22400,
#22401),.UNSPECIFIED.,.F.,.F.,(4,2,4),(1.00000012038514E-6,0.161160399904662,
0.323167607237004),.UNSPECIFIED.);
#1168=B_SPLINE_CURVE_WITH_KNOTS('',3,(#22402,#22403,#22404,#22405,#22406,
#22407),.UNSPECIFIED.,.F.,.F.,(4,2,4),(1.00000022107472E-6,0.167102971345737,
0.33414975330002),.UNSPECIFIED.);
#1169=B_SPLINE_CURVE_WITH_KNOTS('',3,(#22409,#22410,#22411,#22412,#22413,
#22414),.UNSPECIFIED.,.F.,.F.,(4,2,4),(1.00000012039255E-6,0.161160399904654,
0.323167607237),.UNSPECIFIED.);
#1170=B_SPLINE_CURVE_WITH_KNOTS('',3,(#22415,#22416,#22417,#22418,#22419,
#22420),.UNSPECIFIED.,.F.,.F.,(4,2,4),(1.00000022054453E-6,0.167102971345693,
0.334149753299904),.UNSPECIFIED.);
#1171=B_SPLINE_CURVE_WITH_KNOTS('',3,(#22422,#22423,#22424,#22425,#22426,
#22427),.UNSPECIFIED.,.F.,.F.,(4,2,4),(1.00000012058307E-6,0.161159889606735,
0.323167607236912),.UNSPECIFIED.);
#1172=B_SPLINE_CURVE_WITH_KNOTS('',3,(#22428,#22429,#22430,#22431,#22432,
#22433),.UNSPECIFIED.,.F.,.F.,(4,2,4),(1.00000022069235E-6,0.167102971345655,
0.334149753299868),.UNSPECIFIED.);
#1173=B_SPLINE_CURVE_WITH_KNOTS('',3,(#22435,#22436,#22437,#22438,#22439,
#22440),.UNSPECIFIED.,.F.,.F.,(4,2,4),(1.00000012093059E-6,0.161160399904649,
0.323167607236986),.UNSPECIFIED.);
#1174=B_SPLINE_CURVE_WITH_KNOTS('',3,(#22441,#22442,#22443,#22444,#22445,
#22446),.UNSPECIFIED.,.F.,.F.,(4,2,4),(1.00000022078288E-6,0.167102971345831,
0.334149753300156),.UNSPECIFIED.);
#1175=B_SPLINE_CURVE_WITH_KNOTS('',3,(#22448,#22449,#22450,#22451,#22452,
#22453),.UNSPECIFIED.,.F.,.F.,(4,2,4),(1.00000012057364E-6,0.161160399904675,
0.323167607237077),.UNSPECIFIED.);
#1176=B_SPLINE_CURVE_WITH_KNOTS('',3,(#22454,#22455,#22456,#22457,#22458,
#22459),.UNSPECIFIED.,.F.,.F.,(4,2,4),(1.000000220711E-6,0.167102971345943,
0.334149753300391),.UNSPECIFIED.);
#1177=B_SPLINE_CURVE_WITH_KNOTS('',3,(#22461,#22462,#22463,#22464,#22465,
#22466),.UNSPECIFIED.,.F.,.F.,(4,2,4),(1.00000012058037E-6,0.161160399904651,
0.323167607236874),.UNSPECIFIED.);
#1178=B_SPLINE_CURVE_WITH_KNOTS('',3,(#22467,#22468,#22469,#22470,#22471,
#22472),.UNSPECIFIED.,.F.,.F.,(4,2,4),(1.00000022031051E-6,0.167102971345854,
0.334149753300263),.UNSPECIFIED.);
#1179=B_SPLINE_CURVE_WITH_KNOTS('',3,(#22474,#22475,#22476,#22477,#22478,
#22479),.UNSPECIFIED.,.F.,.F.,(4,2,4),(1.00000012055685E-6,0.161160399904695,
0.323167607237214),.UNSPECIFIED.);
#1180=B_SPLINE_CURVE_WITH_KNOTS('',3,(#22480,#22481,#22482,#22483,#22484,
#22485),.UNSPECIFIED.,.F.,.F.,(4,2,4),(1.00000022029865E-6,0.167102971345825,
0.334149753300157),.UNSPECIFIED.);
#1181=B_SPLINE_CURVE_WITH_KNOTS('',3,(#22487,#22488,#22489,#22490,#22491,
#22492),.UNSPECIFIED.,.F.,.F.,(4,2,4),(1.00000012053579E-6,0.161160399904707,
0.323167607237315),.UNSPECIFIED.);
#1182=B_SPLINE_CURVE_WITH_KNOTS('',3,(#22493,#22494,#22495,#22496,#22497,
#22498),.UNSPECIFIED.,.F.,.F.,(4,2,4),(1.00000022063479E-6,0.167102971345967,
0.334149753300421),.UNSPECIFIED.);
#1183=B_SPLINE_CURVE_WITH_KNOTS('',3,(#22500,#22501,#22502,#22503,#22504,
#22505),.UNSPECIFIED.,.F.,.F.,(4,2,4),(1.00000012093733E-6,0.161160399904629,
0.323167607236834),.UNSPECIFIED.);
#1184=B_SPLINE_CURVE_WITH_KNOTS('',3,(#22506,#22507,#22508,#22509,#22510,
#22511),.UNSPECIFIED.,.F.,.F.,(4,2,4),(1.0000002205328E-6,0.16710297134574,
0.334149753300078),.UNSPECIFIED.);
#1185=B_SPLINE_CURVE_WITH_KNOTS('',3,(#22513,#22514,#22515,#22516,#22517,
#22518),.UNSPECIFIED.,.F.,.F.,(4,2,4),(1.00000012048169E-6,0.161159889606741,
0.323167607237064),.UNSPECIFIED.);
#1186=B_SPLINE_CURVE_WITH_KNOTS('',3,(#22519,#22520,#22521,#22522,#22523,
#22524),.UNSPECIFIED.,.F.,.F.,(4,2,4),(1.00000022062917E-6,0.167102971345646,
0.334149753299816),.UNSPECIFIED.);
#1187=B_SPLINE_CURVE_WITH_KNOTS('',3,(#22526,#22527,#22528,#22529,#22530,
#22531),.UNSPECIFIED.,.F.,.F.,(4,2,4),(1.00000012032585E-6,0.16116039990466,
0.323167607237033),.UNSPECIFIED.);
#1188=B_SPLINE_CURVE_WITH_KNOTS('',3,(#22532,#22533,#22534,#22535,#22536,
#22537),.UNSPECIFIED.,.F.,.F.,(4,2,4),(1.00000022065021E-6,0.167102971345787,
0.334149753300079),.UNSPECIFIED.);
#1189=B_SPLINE_CURVE_WITH_KNOTS('',3,(#22539,#22540,#22541,#22542,#22543,
#22544),.UNSPECIFIED.,.F.,.F.,(4,2,4),(1.00000012068184E-6,0.16115988960672,
0.323167607236954),.UNSPECIFIED.);
#1190=B_SPLINE_CURVE_WITH_KNOTS('',3,(#22545,#22546,#22547,#22548,#22549,
#22550),.UNSPECIFIED.,.F.,.F.,(4,2,4),(1.0000002207771E-6,0.167102971345759,
0.334149753300061),.UNSPECIFIED.);
#1191=B_SPLINE_CURVE_WITH_KNOTS('',3,(#22552,#22553,#22554,#22555,#22556,
#22557),.UNSPECIFIED.,.F.,.F.,(4,2,4),(1.00000012044603E-6,0.161160399904649,
0.323167607237023),.UNSPECIFIED.);
#1192=B_SPLINE_CURVE_WITH_KNOTS('',3,(#22558,#22559,#22560,#22561,#22562,
#22563),.UNSPECIFIED.,.F.,.F.,(4,2,4),(1.00000022079248E-6,0.1671029713458,
0.33414975330013),.UNSPECIFIED.);
#1193=B_SPLINE_CURVE_WITH_KNOTS('',3,(#22565,#22566,#22567,#22568,#22569,
#22570),.UNSPECIFIED.,.F.,.F.,(4,2,4),(1.00000012037424E-6,0.161160399904647,
0.323167607237001),.UNSPECIFIED.);
#1194=B_SPLINE_CURVE_WITH_KNOTS('',3,(#22571,#22572,#22573,#22574,#22575,
#22576),.UNSPECIFIED.,.F.,.F.,(4,2,4),(1.00000022090657E-6,0.167102971345759,
0.334149753300051),.UNSPECIFIED.);
#1195=B_SPLINE_CURVE_WITH_KNOTS('',3,(#22578,#22579,#22580,#22581,#22582,
#22583),.UNSPECIFIED.,.F.,.F.,(4,2,4),(1.00000012028251E-6,0.161160399904642,
0.323167607236946),.UNSPECIFIED.);
#1196=B_SPLINE_CURVE_WITH_KNOTS('',3,(#22584,#22585,#22586,#22587,#22588,
#22589),.UNSPECIFIED.,.F.,.F.,(4,2,4),(1.00000022075346E-6,0.167102971345758,
0.334149753300091),.UNSPECIFIED.);
#1197=B_SPLINE_CURVE_WITH_KNOTS('',3,(#22591,#22592,#22593,#22594,#22595,
#22596),.UNSPECIFIED.,.F.,.F.,(4,2,4),(1.00000012045161E-6,0.161160399904678,
0.323167607237292),.UNSPECIFIED.);
#1198=B_SPLINE_CURVE_WITH_KNOTS('',3,(#22597,#22598,#22599,#22600,#22601,
#22602),.UNSPECIFIED.,.F.,.F.,(4,2,4),(1.00000022071781E-6,0.167102971346066,
0.334149753300729),.UNSPECIFIED.);
#1199=B_SPLINE_CURVE_WITH_KNOTS('',3,(#22604,#22605,#22606,#22607,#22608,
#22609),.UNSPECIFIED.,.F.,.F.,(4,2,4),(1.00000012085704E-6,0.161160399904647,
0.323167607236899),.UNSPECIFIED.);
#1200=B_SPLINE_CURVE_WITH_KNOTS('',3,(#22610,#22611,#22612,#22613,#22614,
#22615),.UNSPECIFIED.,.F.,.F.,(4,2,4),(1.00000022074304E-6,0.167102971345757,
0.334149753300087),.UNSPECIFIED.);
#1201=B_SPLINE_CURVE_WITH_KNOTS('',3,(#22617,#22618,#22619,#22620,#22621,
#22622),.UNSPECIFIED.,.F.,.F.,(4,2,4),(1.00000012006173E-6,0.161160399904691,
0.323167607237029),.UNSPECIFIED.);
#1202=B_SPLINE_CURVE_WITH_KNOTS('',3,(#22623,#22624,#22625,#22626,#22627,
#22628),.UNSPECIFIED.,.F.,.F.,(4,2,4),(1.00000022083549E-6,0.167102971345888,
0.334149753300255),.UNSPECIFIED.);
#1203=B_SPLINE_CURVE_WITH_KNOTS('',3,(#22630,#22631,#22632,#22633,#22634,
#22635),.UNSPECIFIED.,.F.,.F.,(4,2,4),(1.00000012064762E-6,0.161160399904703,
0.323167607237272),.UNSPECIFIED.);
#1204=B_SPLINE_CURVE_WITH_KNOTS('',3,(#22636,#22637,#22638,#22639,#22640,
#22641),.UNSPECIFIED.,.F.,.F.,(4,2,4),(1.00000022088092E-6,0.167102971345646,
0.33414975329985),.UNSPECIFIED.);
#1205=B_SPLINE_CURVE_WITH_KNOTS('',3,(#22643,#22644,#22645,#22646,#22647,
#22648),.UNSPECIFIED.,.F.,.F.,(4,2,4),(1.00000012096778E-6,0.161160399904595,
0.323167607236728),.UNSPECIFIED.);
#1206=B_SPLINE_CURVE_WITH_KNOTS('',3,(#22649,#22650,#22651,#22652,#22653,
#22654),.UNSPECIFIED.,.F.,.F.,(4,2,4),(1.00000022064523E-6,0.167102971345871,
0.334149753300307),.UNSPECIFIED.);
#1207=B_SPLINE_CURVE_WITH_KNOTS('',3,(#22656,#22657,#22658,#22659,#22660,
#22661),.UNSPECIFIED.,.F.,.F.,(4,2,4),(1.00000012057745E-6,0.161160399904619,
0.32316760723675),.UNSPECIFIED.);
#1208=B_SPLINE_CURVE_WITH_KNOTS('',3,(#22662,#22663,#22664,#22665,#22666,
#22667),.UNSPECIFIED.,.F.,.F.,(4,2,4),(1.00000022078269E-6,0.167102971345806,
0.334149753300164),.UNSPECIFIED.);
#1209=B_SPLINE_CURVE_WITH_KNOTS('',3,(#22669,#22670,#22671,#22672,#22673,
#22674),.UNSPECIFIED.,.F.,.F.,(4,2,4),(1.00000012048116E-6,0.16116039990468,
0.323167607237172),.UNSPECIFIED.);
#1210=B_SPLINE_CURVE_WITH_KNOTS('',3,(#22675,#22676,#22677,#22678,#22679,
#22680),.UNSPECIFIED.,.F.,.F.,(4,2,4),(1.00000022054791E-6,0.167102971345839,
0.334149753300197),.UNSPECIFIED.);
#1211=B_SPLINE_CURVE_WITH_KNOTS('',3,(#22682,#22683,#22684,#22685,#22686,
#22687),.UNSPECIFIED.,.F.,.F.,(4,2,4),(1.00000012048408E-6,0.161159889606746,
0.323167607237105),.UNSPECIFIED.);
#1212=B_SPLINE_CURVE_WITH_KNOTS('',3,(#22688,#22689,#22690,#22691,#22692,
#22693),.UNSPECIFIED.,.F.,.F.,(4,2,4),(1.00000022061624E-6,0.16710297134579,
0.3341497533002),.UNSPECIFIED.);
#1213=B_SPLINE_CURVE_WITH_KNOTS('',3,(#22695,#22696,#22697,#22698,#22699,
#22700),.UNSPECIFIED.,.F.,.F.,(4,2,4),(1.00000012060288E-6,0.161159889606819,
0.32316760723714),.UNSPECIFIED.);
#1214=B_SPLINE_CURVE_WITH_KNOTS('',3,(#22701,#22702,#22703,#22704,#22705,
#22706),.UNSPECIFIED.,.F.,.F.,(4,2,4),(1.00000022039092E-6,0.16710297134578,
0.334149753300241),.UNSPECIFIED.);
#1215=B_SPLINE_CURVE_WITH_KNOTS('',3,(#22708,#22709,#22710,#22711,#22712,
#22713),.UNSPECIFIED.,.F.,.F.,(4,2,4),(1.00000012039262E-6,0.161159889606932,
0.323167607237268),.UNSPECIFIED.);
#1216=B_SPLINE_CURVE_WITH_KNOTS('',3,(#22714,#22715,#22716,#22717,#22718,
#22719),.UNSPECIFIED.,.F.,.F.,(4,2,4),(1.00000022068054E-6,0.167102971345753,
0.334149753300243),.UNSPECIFIED.);
#1217=B_SPLINE_CURVE_WITH_KNOTS('',3,(#22721,#22722,#22723,#22724,#22725,
#22726),.UNSPECIFIED.,.F.,.F.,(4,2,4),(1.00000012008432E-6,0.161160399904884,
0.323167607237139),.UNSPECIFIED.);
#1218=B_SPLINE_CURVE_WITH_KNOTS('',3,(#22727,#22728,#22729,#22730,#22731,
#22732),.UNSPECIFIED.,.F.,.F.,(4,2,4),(1.00000022061894E-6,0.167102971345809,
0.334149753300514),.UNSPECIFIED.);
#1219=B_SPLINE_CURVE_WITH_KNOTS('',3,(#22734,#22735,#22736,#22737,#22738,
#22739),.UNSPECIFIED.,.F.,.F.,(4,2,4),(1.00000012081545E-6,0.161160399905061,
0.323167607237863),.UNSPECIFIED.);
#1220=B_SPLINE_CURVE_WITH_KNOTS('',3,(#22740,#22741,#22742,#22743,#22744,
#22745),.UNSPECIFIED.,.F.,.F.,(4,2,4),(1.00000022055009E-6,0.16710297134578,
0.334149753300514),.UNSPECIFIED.);
#1221=B_SPLINE_CURVE_WITH_KNOTS('',3,(#22747,#22748,#22749,#22750,#22751,
#22752),.UNSPECIFIED.,.F.,.F.,(4,2,4),(1.00000012031008E-6,0.161160399905076,
0.323167607237676),.UNSPECIFIED.);
#1222=B_SPLINE_CURVE_WITH_KNOTS('',3,(#22753,#22754,#22755,#22756,#22757,
#22758),.UNSPECIFIED.,.F.,.F.,(4,2,4),(1.00000022063654E-6,0.167102971345982,
0.334149753301056),.UNSPECIFIED.);
#1223=B_SPLINE_CURVE_WITH_KNOTS('',3,(#22760,#22761,#22762,#22763,#22764,
#22765),.UNSPECIFIED.,.F.,.F.,(4,2,4),(1.00000012057795E-6,0.161159889607266,
0.323167607237755),.UNSPECIFIED.);
#1224=B_SPLINE_CURVE_WITH_KNOTS('',3,(#22766,#22767,#22768,#22769,#22770,
#22771),.UNSPECIFIED.,.F.,.F.,(4,2,4),(1.00000022038566E-6,0.167102971345924,
0.334149753300952),.UNSPECIFIED.);
#1225=B_SPLINE_CURVE_WITH_KNOTS('',3,(#22773,#22774,#22775,#22776,#22777,
#22778),.UNSPECIFIED.,.F.,.F.,(4,2,4),(1.00000012035839E-6,0.161160399905228,
0.323167607237738),.UNSPECIFIED.);
#1226=B_SPLINE_CURVE_WITH_KNOTS('',3,(#22779,#22780,#22781,#22782,#22783,
#22784),.UNSPECIFIED.,.F.,.F.,(4,2,4),(1.00000022108953E-6,0.167102971345621,
0.334149753300335),.UNSPECIFIED.);
#1227=B_SPLINE_CURVE_WITH_KNOTS('',3,(#22786,#22787,#22788,#22789,#22790,
#22791),.UNSPECIFIED.,.F.,.F.,(4,2,4),(1.00000011994104E-6,0.161159889607422,
0.323167607237808),.UNSPECIFIED.);
#1228=B_SPLINE_CURVE_WITH_KNOTS('',3,(#22792,#22793,#22794,#22795,#22796,
#22797),.UNSPECIFIED.,.F.,.F.,(4,2,4),(1.00000022079877E-6,0.167102971345911,
0.334149753301048),.UNSPECIFIED.);
#1229=B_SPLINE_CURVE_WITH_KNOTS('',3,(#22799,#22800,#22801,#22802,#22803,
#22804),.UNSPECIFIED.,.F.,.F.,(4,2,4),(1.00000012034089E-6,0.161160399905409,
0.323167607237919),.UNSPECIFIED.);
#1230=B_SPLINE_CURVE_WITH_KNOTS('',3,(#22805,#22806,#22807,#22808,#22809,
#22810),.UNSPECIFIED.,.F.,.F.,(4,2,4),(1.0000002204628E-6,0.167102971345718,
0.334149753300732),.UNSPECIFIED.);
#1231=B_SPLINE_CURVE_WITH_KNOTS('',3,(#22812,#22813,#22814,#22815,#22816,
#22817),.UNSPECIFIED.,.F.,.F.,(4,2,4),(1.00000011993139E-6,0.161159889607588,
0.323167607237936),.UNSPECIFIED.);
#1232=B_SPLINE_CURVE_WITH_KNOTS('',3,(#22818,#22819,#22820,#22821,#22822,
#22823),.UNSPECIFIED.,.F.,.F.,(4,2,4),(1.00000022104047E-6,0.167102971345937,
0.334149753301223),.UNSPECIFIED.);
#1233=B_SPLINE_CURVE_WITH_KNOTS('',3,(#22825,#22826,#22827,#22828,#22829,
#22830),.UNSPECIFIED.,.F.,.F.,(4,2,4),(1.00000012050061E-6,0.161160399905562,
0.323167607237955),.UNSPECIFIED.);
#1234=B_SPLINE_CURVE_WITH_KNOTS('',3,(#22831,#22832,#22833,#22834,#22835,
#22836),.UNSPECIFIED.,.F.,.F.,(4,2,4),(1.00000022052091E-6,0.167102971345926,
0.334149753301295),.UNSPECIFIED.);
#1235=B_SPLINE_CURVE_WITH_KNOTS('',3,(#22891,#22892,#22893,#22894,#22895,
#22896,#22897,#22898,#22899,#22900,#22901,#22902,#22903,#22904,#22905,#22906,
#22907,#22908,#22909,#22910,#22911,#22912,#22913,#22914,#22915,#22916,#22917,
#22918,#22919,#22920,#22921,#22922,#22923,#22924,#22925,#22926,#22927,#22928,
#22929,#22930,#22931,#22932,#22933,#22934,#22935,#22936,#22937,#22938,#22939,
#22940,#22941,#22942),.UNSPECIFIED.,.F.,.F.,(4,3,3,3,3,3,3,3,3,3,3,3,3,
3,3,3,3,4),(0.,0.0290398589546445,0.0579843816831971,0.0868853129795454,
0.115761457357984,0.144631560789434,0.173538323016997,0.202474581669382,
0.2314954385994,0.249999999943001,0.279015696481342,0.30796588845617,0.336869516660747,
0.365745410793947,0.394622693781268,0.423510570114902,0.452445568558316,
0.460808762537663),.UNSPECIFIED.);
#1236=B_SPLINE_CURVE_WITH_KNOTS('',3,(#23074,#23075,#23076,#23077,#23078,
#23079,#23080,#23081),.UNSPECIFIED.,.F.,.F.,(4,2,2,4),(0.0783698293107414,
0.308777371982556,0.539184914655036,0.562623084473123),.UNSPECIFIED.);
#1237=B_SPLINE_CURVE_WITH_KNOTS('',3,(#23224,#23225,#23226,#23227,#23228,
#23229,#23230,#23231,#23232,#23233,#23234,#23235,#23236,#23237,#23238,#23239,
#23240,#23241,#23242,#23243,#23244,#23245,#23246,#23247,#23248,#23249,#23250,
#23251,#23252,#23253,#23254,#23255,#23256,#23257,#23258,#23259,#23260,#23261,
#23262,#23263,#23264,#23265,#23266,#23267,#23268,#23269,#23270,#23271,#23272,
#23273,#23274,#23275),.UNSPECIFIED.,.F.,.F.,(4,3,3,3,3,3,3,3,3,3,3,3,3,
3,3,3,3,4),(0.,0.0290398589545971,0.0579843816831279,0.0868853129794532,
0.115761457357872,0.144631560789305,0.173538323016845,0.202474581669205,
0.231495438599207,0.249999999943415,0.279015696481713,0.307965888456488,
0.336869516660988,0.365745410794182,0.394622693781447,0.423510570114973,
0.45244556855835,0.460808762537663),.UNSPECIFIED.);
#1238=B_SPLINE_CURVE_WITH_KNOTS('',3,(#23396,#23397,#23398,#23399,#23400,
#23401,#23402,#23403,#23404,#23405,#23406,#23407,#23408,#23409,#23410,#23411,
#23412,#23413,#23414,#23415,#23416,#23417,#23418,#23419,#23420,#23421,#23422,
#23423,#23424,#23425,#23426,#23427,#23428,#23429,#23430,#23431,#23432,#23433,
#23434,#23435,#23436,#23437,#23438,#23439,#23440,#23441,#23442,#23443,#23444,
#23445,#23446,#23447),.UNSPECIFIED.,.F.,.F.,(4,3,3,3,3,3,3,3,3,3,3,3,3,
3,3,3,3,4),(0.,0.029039858954596,0.0579843816831248,0.0868853129794533,
0.115761457357877,0.144631560789305,0.173538323016854,0.202474581669227,
0.231495438599218,0.249999999943415,0.279015696481708,0.307965888456495,
0.336869516661002,0.365745410794122,0.394622693781374,0.423510570114958,
0.452445568558351,0.460808762537663),.UNSPECIFIED.);
#1239=B_SPLINE_CURVE_WITH_KNOTS('',3,(#23693,#23694,#23695,#23696,#23697,
#23698,#23699,#23700,#23701,#23702,#23703,#23704,#23705,#23706,#23707,#23708,
#23709,#23710,#23711,#23712,#23713,#23714,#23715,#23716,#23717,#23718,#23719,
#23720,#23721,#23722,#23723,#23724,#23725,#23726,#23727,#23728,#23729,#23730,
#23731,#23732,#23733,#23734,#23735,#23736,#23737,#23738,#23739,#23740,#23741,
#23742,#23743,#23744),.UNSPECIFIED.,.F.,.F.,(4,3,3,3,3,3,3,3,3,3,3,3,3,
3,3,3,3,4),(0.,0.0290398589546279,0.0579843816831548,0.086885312979481,
0.115761457357894,0.14463156078933,0.173538323016879,0.202474581669232,
0.231495438599223,0.249999999943415,0.279015696481706,0.307965888456492,
0.336869516661009,0.365745410794138,0.394622693781402,0.423510570114935,
0.452445568558275,0.460808762537663),.UNSPECIFIED.);
#1240=B_SPLINE_CURVE_WITH_KNOTS('',3,(#23865,#23866,#23867,#23868,#23869,
#23870,#23871,#23872,#23873,#23874,#23875,#23876,#23877,#23878,#23879,#23880,
#23881,#23882,#23883,#23884,#23885,#23886,#23887,#23888,#23889,#23890,#23891,
#23892,#23893,#23894,#23895,#23896,#23897,#23898,#23899,#23900,#23901,#23902,
#23903,#23904,#23905,#23906,#23907,#23908,#23909,#23910,#23911,#23912,#23913,
#23914,#23915,#23916),.UNSPECIFIED.,.F.,.F.,(4,3,3,3,3,3,3,3,3,3,3,3,3,
3,3,3,3,4),(0.,0.0290398589546199,0.0579843816831478,0.0868853129794725,
0.11576145735789,0.144631560789328,0.17353832301687,0.202474581669228,0.231495438599226,
0.249999999943415,0.279015696481709,0.307965888456473,0.336869516660979,
0.365745410794135,0.394622693781407,0.423510570114972,0.452445568558348,
0.460808762537948),.UNSPECIFIED.);
#1241=B_SPLINE_CURVE_WITH_KNOTS('',3,(#24037,#24038,#24039,#24040,#24041,
#24042,#24043,#24044,#24045,#24046,#24047,#24048,#24049,#24050,#24051,#24052,
#24053,#24054,#24055,#24056,#24057,#24058,#24059,#24060,#24061,#24062,#24063,
#24064,#24065,#24066,#24067,#24068,#24069,#24070,#24071,#24072,#24073,#24074,
#24075,#24076,#24077,#24078,#24079,#24080,#24081,#24082,#24083,#24084,#24085,
#24086,#24087,#24088),.UNSPECIFIED.,.F.,.F.,(4,3,3,3,3,3,3,3,3,3,3,3,3,
3,3,3,3,4),(0.,0.0290398589546317,0.0579843816831625,0.0868853129794868,
0.115761457357901,0.144631560789317,0.173538323016866,0.202474581669238,
0.231495438599229,0.249999999943415,0.279015696481706,0.307965888456485,
0.336869516660966,0.365745410794117,0.394622693781377,0.423510570114936,
0.452445568558318,0.460808762537663),.UNSPECIFIED.);
#1242=B_SPLINE_CURVE_WITH_KNOTS('',3,(#24209,#24210,#24211,#24212,#24213,
#24214,#24215,#24216,#24217,#24218,#24219,#24220,#24221,#24222,#24223,#24224,
#24225,#24226,#24227,#24228,#24229,#24230,#24231,#24232,#24233,#24234,#24235,
#24236,#24237,#24238,#24239,#24240,#24241,#24242,#24243,#24244,#24245,#24246,
#24247,#24248,#24249,#24250,#24251,#24252,#24253,#24254,#24255,#24256,#24257,
#24258,#24259,#24260),.UNSPECIFIED.,.F.,.F.,(4,3,3,3,3,3,3,3,3,3,3,3,3,
3,3,3,3,4),(0.,0.0290398589545938,0.0579843816831263,0.0868853129794523,
0.115761457357861,0.144631560789281,0.173538323016826,0.202474581669178,
0.231495438599186,0.249999999943415,0.279015696481703,0.307965888456488,
0.336869516660999,0.365745410794192,0.394622693781458,0.423510570115037,
0.452445568558385,0.460808762537663),.UNSPECIFIED.);
#1243=B_SPLINE_CURVE_WITH_KNOTS('',3,(#24381,#24382,#24383,#24384,#24385,
#24386,#24387,#24388,#24389,#24390,#24391,#24392,#24393,#24394,#24395,#24396,
#24397,#24398,#24399,#24400,#24401,#24402,#24403,#24404,#24405,#24406,#24407,
#24408,#24409,#24410,#24411,#24412,#24413,#24414,#24415,#24416,#24417,#24418,
#24419,#24420,#24421,#24422,#24423,#24424,#24425,#24426,#24427,#24428,#24429,
#24430,#24431,#24432),.UNSPECIFIED.,.F.,.F.,(4,3,3,3,3,3,3,3,3,3,3,3,3,
3,3,3,3,4),(0.,0.029039858954607,0.057984381683134,0.0868853129794584,0.115761457357883,
0.144631560789343,0.173538323016891,0.202474581669253,0.23149543859925,
0.249999999943415,0.279015696481708,0.307965888456493,0.336869516661006,
0.365745410794227,0.39462269378149,0.423510570115083,0.452445568558457,
0.460808762537663),.UNSPECIFIED.);
#1244=B_SPLINE_CURVE_WITH_KNOTS('',3,(#24553,#24554,#24555,#24556,#24557,
#24558,#24559,#24560,#24561,#24562,#24563,#24564,#24565,#24566,#24567,#24568,
#24569,#24570,#24571,#24572,#24573,#24574,#24575,#24576,#24577,#24578,#24579,
#24580,#24581,#24582,#24583,#24584,#24585,#24586,#24587,#24588,#24589,#24590,
#24591,#24592,#24593,#24594,#24595,#24596,#24597,#24598,#24599,#24600,#24601,
#24602,#24603,#24604),.UNSPECIFIED.,.F.,.F.,(4,3,3,3,3,3,3,3,3,3,3,3,3,
3,3,3,3,4),(0.,0.029039858954619,0.0579843816831522,0.0868853129794786,
0.115761457357895,0.144631560789334,0.17353832301688,0.202474581669239,
0.23149543859923,0.249999999943415,0.279015696481715,0.307965888456487,
0.336869516660996,0.365745410794131,0.394622693781399,0.423510570114902,
0.452445568558267,0.460808762537948),.UNSPECIFIED.);
#1245=B_SPLINE_CURVE_WITH_KNOTS('',3,(#24725,#24726,#24727,#24728,#24729,
#24730,#24731,#24732,#24733,#24734,#24735,#24736,#24737,#24738,#24739,#24740,
#24741,#24742,#24743,#24744,#24745,#24746,#24747,#24748,#24749,#24750,#24751,
#24752,#24753,#24754,#24755,#24756,#24757,#24758,#24759,#24760,#24761,#24762,
#24763,#24764,#24765,#24766,#24767,#24768,#24769,#24770,#24771,#24772,#24773,
#24774,#24775,#24776),.UNSPECIFIED.,.F.,.F.,(4,3,3,3,3,3,3,3,3,3,3,3,3,
3,3,3,3,4),(0.,0.0290398589546166,0.0579843816831443,0.0868853129794682,
0.115761457357876,0.144631560789308,0.173538323016849,0.202474581669216,
0.231495438599206,0.249999999943415,0.279015696481708,0.307965888456497,
0.336869516660995,0.365745410794177,0.394622693781448,0.423510570114999,
0.452445568558359,0.460808762537663),.UNSPECIFIED.);
#1246=B_SPLINE_CURVE_WITH_KNOTS('',3,(#24897,#24898,#24899,#24900,#24901,
#24902,#24903,#24904,#24905,#24906,#24907,#24908,#24909,#24910,#24911,#24912,
#24913,#24914,#24915,#24916,#24917,#24918,#24919,#24920,#24921,#24922,#24923,
#24924,#24925,#24926,#24927,#24928,#24929,#24930,#24931,#24932,#24933,#24934,
#24935,#24936,#24937,#24938,#24939,#24940,#24941,#24942,#24943,#24944,#24945,
#24946,#24947,#24948),.UNSPECIFIED.,.F.,.F.,(4,3,3,3,3,3,3,3,3,3,3,3,3,
3,3,3,3,4),(0.,0.0290398589545852,0.0579843816831127,0.0868853129794385,
0.115761457357852,0.144631560789294,0.173538323016838,0.202474581669212,
0.231495438599219,0.249999999943415,0.279015696481717,0.307965888456499,
0.336869516661014,0.365745410794191,0.394622693781443,0.423510570114999,
0.452445568558387,0.460808762537663),.UNSPECIFIED.);
#1247=B_SPLINE_CURVE_WITH_KNOTS('',3,(#25194,#25195,#25196,#25197,#25198,
#25199,#25200,#25201,#25202,#25203,#25204,#25205,#25206,#25207,#25208,#25209,
#25210,#25211,#25212,#25213,#25214,#25215,#25216,#25217,#25218,#25219,#25220,
#25221,#25222,#25223,#25224,#25225,#25226,#25227,#25228,#25229,#25230,#25231,
#25232,#25233,#25234,#25235,#25236,#25237,#25238,#25239,#25240,#25241,#25242,
#25243,#25244,#25245),.UNSPECIFIED.,.F.,.F.,(4,3,3,3,3,3,3,3,3,3,3,3,3,
3,3,3,3,4),(0.,0.0290398589546215,0.0579843816831506,0.0868853129794766,
0.115761457357889,0.144631560789315,0.173538323016858,0.202474581669225,
0.23149543859923,0.249999999943415,0.279015696481707,0.307965888456492,
0.336869516660998,0.365745410794129,0.394622693781395,0.423510570114959,
0.452445568558335,0.460808762537663),.UNSPECIFIED.);
#1248=B_SPLINE_CURVE_WITH_KNOTS('',3,(#25366,#25367,#25368,#25369,#25370,
#25371,#25372,#25373,#25374,#25375,#25376,#25377,#25378,#25379,#25380,#25381,
#25382,#25383,#25384,#25385,#25386,#25387,#25388,#25389,#25390,#25391,#25392,
#25393,#25394,#25395,#25396,#25397,#25398,#25399,#25400,#25401,#25402,#25403,
#25404,#25405,#25406,#25407,#25408,#25409,#25410,#25411,#25412,#25413,#25414,
#25415,#25416,#25417),.UNSPECIFIED.,.F.,.F.,(4,3,3,3,3,3,3,3,3,3,3,3,3,
3,3,3,3,4),(0.,0.0290398589546135,0.0579843816831423,0.0868853129794702,
0.115761457357887,0.144631560789319,0.17353832301686,0.202474581669214,
0.231495438599214,0.249999999943415,0.27901569648171,0.307965888456478,
0.33686951666102,0.365745410794196,0.394622693781435,0.42351057011498,0.452445568558357,
0.460808762537663),.UNSPECIFIED.);
#1249=B_SPLINE_CURVE_WITH_KNOTS('',3,(#25663,#25664,#25665,#25666,#25667,
#25668,#25669,#25670,#25671,#25672,#25673,#25674,#25675,#25676,#25677,#25678,
#25679,#25680,#25681,#25682,#25683,#25684,#25685,#25686,#25687,#25688,#25689,
#25690,#25691,#25692,#25693,#25694,#25695,#25696,#25697,#25698,#25699,#25700,
#25701,#25702,#25703,#25704,#25705,#25706,#25707,#25708,#25709,#25710,#25711,
#25712,#25713,#25714),.UNSPECIFIED.,.F.,.F.,(4,3,3,3,3,3,3,3,3,3,3,3,3,
3,3,3,3,4),(0.,0.029039858954608,0.0579843816831391,0.0868853129794618,
0.11576145735788,0.144631560789298,0.173538323016834,0.202474581669206,
0.231495438599219,0.249999999943415,0.279015696481705,0.307965888456485,
0.336869516660995,0.365745410794133,0.394622693781401,0.423510570114937,
0.452445568558294,0.460808762537949),.UNSPECIFIED.);
#1250=B_SPLINE_CURVE_WITH_KNOTS('',3,(#25835,#25836,#25837,#25838,#25839,
#25840,#25841,#25842,#25843,#25844,#25845,#25846,#25847,#25848,#25849,#25850,
#25851,#25852,#25853,#25854,#25855,#25856,#25857,#25858,#25859,#25860,#25861,
#25862,#25863,#25864,#25865,#25866,#25867,#25868,#25869,#25870,#25871,#25872,
#25873,#25874,#25875,#25876,#25877,#25878,#25879,#25880,#25881,#25882,#25883,
#25884,#25885,#25886),.UNSPECIFIED.,.F.,.F.,(4,3,3,3,3,3,3,3,3,3,3,3,3,
3,3,3,3,4),(0.,0.0290398589545822,0.0579843816831122,0.0868853129794408,
0.115761457357852,0.144631560789278,0.17353832301682,0.202474581669178,
0.231495438599178,0.249999999943415,0.279015696481709,0.307965888456482,
0.336869516660988,0.365745410794173,0.394622693781441,0.423510570115002,
0.45244556855839,0.460808762537663),.UNSPECIFIED.);
#1251=B_SPLINE_CURVE_WITH_KNOTS('',3,(#26007,#26008,#26009,#26010,#26011,
#26012,#26013,#26014,#26015,#26016,#26017,#26018,#26019,#26020,#26021,#26022,
#26023,#26024,#26025,#26026,#26027,#26028,#26029,#26030,#26031,#26032,#26033,
#26034,#26035,#26036,#26037,#26038,#26039,#26040,#26041,#26042,#26043,#26044,
#26045,#26046,#26047,#26048,#26049,#26050,#26051,#26052,#26053,#26054,#26055,
#26056,#26057,#26058),.UNSPECIFIED.,.F.,.F.,(4,3,3,3,3,3,3,3,3,3,3,3,3,
3,3,3,3,4),(0.,0.0290398589545848,0.057984381683115,0.0868853129794429,
0.115761457357857,0.144631560789289,0.173538323016833,0.202474581669208,
0.231495438599203,0.249999999943415,0.279015696481713,0.307965888456485,
0.33686951666099,0.365745410794146,0.394622693781407,0.423510570114923,
0.452445568558284,0.460808762537663),.UNSPECIFIED.);
#1252=B_SPLINE_CURVE_WITH_KNOTS('',3,(#26179,#26180,#26181,#26182,#26183,
#26184,#26185,#26186,#26187,#26188,#26189,#26190,#26191,#26192,#26193,#26194,
#26195,#26196,#26197,#26198,#26199,#26200,#26201,#26202,#26203,#26204,#26205,
#26206,#26207,#26208,#26209,#26210,#26211,#26212,#26213,#26214,#26215,#26216,
#26217,#26218,#26219,#26220,#26221,#26222,#26223,#26224,#26225,#26226,#26227,
#26228,#26229,#26230),.UNSPECIFIED.,.F.,.F.,(4,3,3,3,3,3,3,3,3,3,3,3,3,
3,3,3,3,4),(0.,0.0290398589546297,0.0579843816831633,0.0868853129794911,
0.115761457357903,0.144631560789311,0.173538323016857,0.202474581669236,
0.231495438599235,0.249999999943415,0.279015696481717,0.307965888456498,
0.33686951666101,0.3657454107942,0.394622693781471,0.423510570115025,0.452445568558387,
0.460808762537948),.UNSPECIFIED.);
#1253=B_SPLINE_CURVE_WITH_KNOTS('',3,(#26351,#26352,#26353,#26354,#26355,
#26356,#26357,#26358,#26359,#26360,#26361,#26362,#26363,#26364,#26365,#26366,
#26367,#26368,#26369,#26370,#26371,#26372,#26373,#26374,#26375,#26376,#26377,
#26378,#26379,#26380,#26381,#26382,#26383,#26384,#26385,#26386,#26387,#26388,
#26389,#26390,#26391,#26392,#26393,#26394,#26395,#26396,#26397,#26398,#26399,
#26400,#26401,#26402),.UNSPECIFIED.,.F.,.F.,(4,3,3,3,3,3,3,3,3,3,3,3,3,
3,3,3,3,4),(0.,0.0290398589546329,0.0579843816831612,0.0868853129794864,
0.115761457357903,0.144631560789325,0.173538323016875,0.202474581669236,
0.231495438599232,0.249999999943415,0.279015696481708,0.307965888456492,
0.336869516660998,0.365745410794162,0.394622693781427,0.423510570114935,
0.452445568558293,0.460808762537663),.UNSPECIFIED.);
#1254=B_SPLINE_CURVE_WITH_KNOTS('',3,(#26523,#26524,#26525,#26526,#26527,
#26528,#26529,#26530,#26531,#26532,#26533,#26534,#26535,#26536,#26537,#26538,
#26539,#26540,#26541,#26542,#26543,#26544,#26545,#26546,#26547,#26548,#26549,
#26550,#26551,#26552,#26553,#26554,#26555,#26556,#26557,#26558,#26559,#26560,
#26561,#26562,#26563,#26564,#26565,#26566,#26567,#26568,#26569,#26570,#26571,
#26572,#26573,#26574),.UNSPECIFIED.,.F.,.F.,(4,3,3,3,3,3,3,3,3,3,3,3,3,
3,3,3,3,4),(0.,0.0290398589545988,0.0579843816831278,0.0868853129794553,
0.115761457357868,0.144631560789295,0.173538323016838,0.202474581669197,
0.231495438599194,0.249999999943415,0.279015696481713,0.307965888456485,
0.336869516660974,0.365745410794115,0.394622693781377,0.423510570114947,
0.452445568558327,0.460808762537662),.UNSPECIFIED.);
#1255=B_SPLINE_CURVE_WITH_KNOTS('',3,(#26695,#26696,#26697,#26698,#26699,
#26700,#26701,#26702,#26703,#26704,#26705,#26706,#26707,#26708,#26709,#26710,
#26711,#26712,#26713,#26714,#26715,#26716,#26717,#26718,#26719,#26720,#26721,
#26722,#26723,#26724,#26725,#26726,#26727,#26728,#26729,#26730,#26731,#26732,
#26733,#26734,#26735,#26736,#26737,#26738,#26739,#26740,#26741,#26742,#26743,
#26744,#26745,#26746),.UNSPECIFIED.,.F.,.F.,(4,3,3,3,3,3,3,3,3,3,3,3,3,
3,3,3,3,4),(0.,0.0290398589546069,0.0579843816831384,0.0868853129794673,
0.115761457357882,0.144631560789308,0.173538323016854,0.202474581669225,
0.231495438599218,0.249999999943415,0.279015696481714,0.30796588845649,
0.336869516661014,0.365745410794146,0.394622693781409,0.423510570114946,
0.45244556855833,0.460808762537664),.UNSPECIFIED.);
#1256=B_SPLINE_CURVE_WITH_KNOTS('',3,(#26867,#26868,#26869,#26870,#26871,
#26872,#26873,#26874,#26875,#26876,#26877,#26878,#26879,#26880,#26881,#26882,
#26883,#26884,#26885,#26886,#26887,#26888,#26889,#26890,#26891,#26892,#26893,
#26894,#26895,#26896,#26897,#26898,#26899,#26900,#26901,#26902,#26903,#26904,
#26905,#26906,#26907,#26908,#26909,#26910,#26911,#26912,#26913,#26914,#26915,
#26916,#26917,#26918),.UNSPECIFIED.,.F.,.F.,(4,3,3,3,3,3,3,3,3,3,3,3,3,
3,3,3,3,4),(0.,0.0290398589546067,0.0579843816831386,0.0868853129794601,
0.115761457357869,0.144631560789311,0.173538323016853,0.202474581669217,
0.231495438599211,0.249999999943415,0.279015696481709,0.307965888456493,
0.336869516660981,0.365745410794142,0.394622693781412,0.423510570114967,
0.452445568558324,0.460808762537663),.UNSPECIFIED.);
#1257=B_SPLINE_CURVE_WITH_KNOTS('',3,(#27039,#27040,#27041,#27042,#27043,
#27044,#27045,#27046,#27047,#27048,#27049,#27050,#27051,#27052,#27053,#27054,
#27055,#27056,#27057,#27058,#27059,#27060,#27061,#27062,#27063,#27064,#27065,
#27066,#27067,#27068,#27069,#27070,#27071,#27072,#27073,#27074,#27075,#27076,
#27077,#27078,#27079,#27080,#27081,#27082,#27083,#27084,#27085,#27086,#27087,
#27088,#27089,#27090),.UNSPECIFIED.,.F.,.F.,(4,3,3,3,3,3,3,3,3,3,3,3,3,
3,3,3,3,4),(0.,0.0290398589546235,0.0579843816831504,0.0868853129794786,
0.115761457357899,0.144631560789329,0.173538323016875,0.202474581669235,
0.231495438599228,0.249999999943415,0.279015696481717,0.307965888456488,
0.336869516661017,0.365745410794157,0.394622693781428,0.423510570114982,
0.452445568558358,0.460808762537662),.UNSPECIFIED.);
#1258=B_SPLINE_CURVE_WITH_KNOTS('',3,(#27461,#27462,#27463,#27464,#27465,
#27466,#27467,#27468,#27469,#27470,#27471,#27472,#27473,#27474,#27475,#27476,
#27477,#27478,#27479,#27480,#27481,#27482,#27483,#27484,#27485,#27486,#27487,
#27488,#27489,#27490,#27491,#27492,#27493,#27494,#27495,#27496,#27497,#27498,
#27499,#27500,#27501,#27502,#27503,#27504,#27505,#27506,#27507,#27508,#27509,
#27510,#27511,#27512),.UNSPECIFIED.,.F.,.F.,(4,3,3,3,3,3,3,3,3,3,3,3,3,
3,3,3,3,4),(0.,0.0290398589545856,0.0579843816831171,0.0868853129794436,
0.115761457357868,0.144631560789292,0.173538323016835,0.202474581669204,
0.2314954385992,0.249999999943414,0.27901569648171,0.307965888456488,0.336869516660999,
0.365745410794178,0.394622693781442,0.423510570114995,0.452445568558389,
0.460808762537663),.UNSPECIFIED.);
#1259=B_SPLINE_CURVE_WITH_KNOTS('',3,(#27633,#27634,#27635,#27636,#27637,
#27638,#27639,#27640,#27641,#27642,#27643,#27644,#27645,#27646,#27647,#27648,
#27649,#27650,#27651,#27652,#27653,#27654,#27655,#27656,#27657,#27658,#27659,
#27660,#27661,#27662,#27663,#27664,#27665,#27666,#27667,#27668,#27669,#27670,
#27671,#27672,#27673,#27674,#27675,#27676,#27677,#27678,#27679,#27680,#27681,
#27682,#27683,#27684),.UNSPECIFIED.,.F.,.F.,(4,3,3,3,3,3,3,3,3,3,3,3,3,
3,3,3,3,4),(0.,0.0290398589546211,0.0579843816831511,0.0868853129794771,
0.115761457357895,0.144631560789324,0.173538323016875,0.202474581669245,
0.231495438599253,0.249999999943415,0.279015696481702,0.307965888456477,
0.336869516660978,0.365745410794173,0.39462269378144,0.423510570114968,
0.452445568558341,0.460808762537949),.UNSPECIFIED.);
#1260=B_SPLINE_CURVE_WITH_KNOTS('',3,(#27805,#27806,#27807,#27808,#27809,
#27810,#27811,#27812,#27813,#27814,#27815,#27816,#27817,#27818,#27819,#27820,
#27821,#27822,#27823,#27824,#27825,#27826,#27827,#27828,#27829,#27830,#27831,
#27832,#27833,#27834,#27835,#27836,#27837,#27838,#27839,#27840,#27841,#27842,
#27843,#27844,#27845,#27846,#27847,#27848,#27849,#27850,#27851,#27852,#27853,
#27854,#27855,#27856),.UNSPECIFIED.,.F.,.F.,(4,3,3,3,3,3,3,3,3,3,3,3,3,
3,3,3,3,4),(0.,0.0290398589545922,0.0579843816831198,0.0868853129794405,
0.115761457357857,0.144631560789285,0.173538323016824,0.202474581669182,
0.231495438599174,0.249999999943415,0.279015696481716,0.307965888456492,
0.336869516661011,0.365745410794209,0.394622693781464,0.42351057011501,
0.452445568558355,0.460808762537948),.UNSPECIFIED.);
#1261=B_SPLINE_CURVE_WITH_KNOTS('',3,(#27977,#27978,#27979,#27980,#27981,
#27982,#27983,#27984,#27985,#27986,#27987,#27988,#27989,#27990,#27991,#27992,
#27993,#27994,#27995,#27996,#27997,#27998,#27999,#28000,#28001,#28002,#28003,
#28004,#28005,#28006,#28007,#28008,#28009,#28010,#28011,#28012,#28013,#28014,
#28015,#28016,#28017,#28018,#28019,#28020,#28021,#28022,#28023,#28024,#28025,
#28026,#28027,#28028),.UNSPECIFIED.,.F.,.F.,(4,3,3,3,3,3,3,3,3,3,3,3,3,
3,3,3,3,4),(0.,0.0290398589546412,0.0579843816831699,0.0868853129794985,
0.115761457357923,0.144631560789358,0.173538323016903,0.202474581669269,
0.231495438599259,0.249999999943415,0.279015696481711,0.307965888456494,
0.336869516660983,0.365745410794105,0.394622693781363,0.423510570114903,
0.452445568558268,0.460808762537948),.UNSPECIFIED.);
#1262=B_SPLINE_CURVE_WITH_KNOTS('',3,(#28149,#28150,#28151,#28152,#28153,
#28154,#28155,#28156,#28157,#28158,#28159,#28160,#28161,#28162,#28163,#28164,
#28165,#28166,#28167,#28168,#28169,#28170,#28171,#28172,#28173,#28174,#28175,
#28176,#28177,#28178,#28179,#28180,#28181,#28182,#28183,#28184,#28185,#28186,
#28187,#28188,#28189,#28190,#28191,#28192,#28193,#28194,#28195,#28196,#28197,
#28198,#28199,#28200),.UNSPECIFIED.,.F.,.F.,(4,3,3,3,3,3,3,3,3,3,3,3,3,
3,3,3,3,4),(0.,0.0290398589546109,0.0579843816831413,0.0868853129794694,
0.115761457357886,0.144631560789337,0.173538323016872,0.202474581669243,
0.231495438599242,0.249999999943415,0.279015696481705,0.307965888456473,
0.336869516660985,0.365745410794155,0.394622693781409,0.423510570114964,
0.452445568558341,0.460808762537948),.UNSPECIFIED.);
#1263=B_SPLINE_CURVE_WITH_KNOTS('',3,(#28321,#28322,#28323,#28324,#28325,
#28326,#28327,#28328,#28329,#28330,#28331,#28332,#28333,#28334,#28335,#28336,
#28337,#28338,#28339,#28340,#28341,#28342,#28343,#28344,#28345,#28346,#28347,
#28348,#28349,#28350,#28351,#28352,#28353,#28354,#28355,#28356,#28357,#28358,
#28359,#28360,#28361,#28362,#28363,#28364,#28365,#28366,#28367,#28368,#28369,
#28370,#28371,#28372),.UNSPECIFIED.,.F.,.F.,(4,3,3,3,3,3,3,3,3,3,3,3,3,
3,3,3,3,4),(0.,0.0290398589546184,0.0579843816831456,0.0868853129794708,
0.115761457357885,0.144631560789321,0.173538323016869,0.202474581669233,
0.231495438599223,0.249999999943415,0.279015696481714,0.307965888456492,
0.33686951666099,0.365745410794174,0.394622693781447,0.423510570115006,
0.452445568558363,0.460808762537662),.UNSPECIFIED.);
#1264=B_SPLINE_CURVE_WITH_KNOTS('',3,(#28743,#28744,#28745,#28746,#28747,
#28748,#28749,#28750,#28751,#28752,#28753,#28754,#28755,#28756,#28757,#28758,
#28759,#28760,#28761,#28762,#28763,#28764,#28765,#28766,#28767,#28768,#28769,
#28770,#28771,#28772,#28773,#28774,#28775,#28776,#28777,#28778,#28779,#28780,
#28781,#28782,#28783,#28784,#28785,#28786,#28787,#28788,#28789,#28790,#28791,
#28792,#28793,#28794),.UNSPECIFIED.,.F.,.F.,(4,3,3,3,3,3,3,3,3,3,3,3,3,
3,3,3,3,4),(0.,0.0290398589546294,0.0579843816831567,0.0868853129794856,
0.115761457357898,0.144631560789333,0.17353832301688,0.202474581669258,
0.231495438599254,0.249999999943415,0.279015696481708,0.307965888456474,
0.336869516660986,0.365745410794101,0.394622693781369,0.423510570114902,
0.45244556855825,0.460808762537663),.UNSPECIFIED.);
#1265=B_SPLINE_CURVE_WITH_KNOTS('',3,(#28915,#28916,#28917,#28918,#28919,
#28920,#28921,#28922,#28923,#28924,#28925,#28926,#28927,#28928,#28929,#28930,
#28931,#28932,#28933,#28934,#28935,#28936,#28937,#28938,#28939,#28940,#28941,
#28942,#28943,#28944,#28945,#28946,#28947,#28948,#28949,#28950,#28951,#28952,
#28953,#28954,#28955,#28956,#28957,#28958,#28959,#28960,#28961,#28962,#28963,
#28964,#28965,#28966),.UNSPECIFIED.,.F.,.F.,(4,3,3,3,3,3,3,3,3,3,3,3,3,
3,3,3,3,4),(0.,0.0290398589546234,0.0579843816831522,0.0868853129794782,
0.115761457357893,0.144631560789316,0.173538323016863,0.202474581669234,
0.231495438599237,0.249999999943415,0.27901569648171,0.307965888456479,
0.336869516660982,0.365745410794167,0.394622693781427,0.42351057011498,
0.452445568558371,0.460808762537948),.UNSPECIFIED.);
#1266=B_SPLINE_CURVE_WITH_KNOTS('',3,(#29212,#29213,#29214,#29215,#29216,
#29217,#29218,#29219,#29220,#29221,#29222,#29223,#29224,#29225,#29226,#29227,
#29228,#29229,#29230,#29231,#29232,#29233,#29234,#29235,#29236,#29237,#29238,
#29239,#29240,#29241,#29242,#29243,#29244,#29245,#29246,#29247,#29248,#29249,
#29250,#29251,#29252,#29253,#29254,#29255,#29256,#29257,#29258,#29259,#29260,
#29261,#29262,#29263),.UNSPECIFIED.,.F.,.F.,(4,3,3,3,3,3,3,3,3,3,3,3,3,
3,3,3,3,4),(0.,0.0290398589546338,0.0579843816831629,0.0868853129794867,
0.115761457357902,0.14463156078933,0.173538323016871,0.202474581669241,
0.231495438599246,0.249999999943414,0.279015696481711,0.307965888456466,
0.336869516660969,0.365745410794144,0.39462269378141,0.423510570114948,
0.452445568558332,0.460808762537663),.UNSPECIFIED.);
#1267=B_SPLINE_CURVE_WITH_KNOTS('',3,(#29384,#29385,#29386,#29387,#29388,
#29389,#29390,#29391,#29392,#29393,#29394,#29395,#29396,#29397,#29398,#29399,
#29400,#29401,#29402,#29403,#29404,#29405,#29406,#29407,#29408,#29409,#29410,
#29411,#29412,#29413,#29414,#29415,#29416,#29417,#29418,#29419,#29420,#29421,
#29422,#29423,#29424,#29425,#29426,#29427,#29428,#29429,#29430,#29431,#29432,
#29433,#29434,#29435),.UNSPECIFIED.,.F.,.F.,(4,3,3,3,3,3,3,3,3,3,3,3,3,
3,3,3,3,4),(0.,0.0290398589546154,0.0579843816831472,0.0868853129794752,
0.115761457357892,0.144631560789324,0.173538323016871,0.202474581669217,
0.231495438599219,0.249999999943415,0.27901569648171,0.307965888456471,
0.336869516660976,0.36574541079416,0.394622693781427,0.423510570115009,
0.452445568558392,0.460808762537663),.UNSPECIFIED.);
#1268=B_SPLINE_CURVE_WITH_KNOTS('',3,(#29556,#29557,#29558,#29559,#29560,
#29561,#29562,#29563,#29564,#29565,#29566,#29567,#29568,#29569,#29570,#29571,
#29572,#29573,#29574,#29575,#29576,#29577,#29578,#29579,#29580,#29581,#29582,
#29583,#29584,#29585,#29586,#29587,#29588,#29589,#29590,#29591,#29592,#29593,
#29594,#29595,#29596,#29597,#29598,#29599,#29600,#29601,#29602,#29603,#29604,
#29605,#29606,#29607),.UNSPECIFIED.,.F.,.F.,(4,3,3,3,3,3,3,3,3,3,3,3,3,
3,3,3,3,4),(0.,0.0290398589545966,0.0579843816831232,0.0868853129794503,
0.115761457357871,0.144631560789306,0.173538323016847,0.202474581669227,
0.231495438599228,0.249999999943415,0.279015696481708,0.307965888456479,
0.336869516660994,0.365745410794156,0.394622693781412,0.423510570114948,
0.452445568558316,0.460808762537949),.UNSPECIFIED.);
#1269=B_SPLINE_CURVE_WITH_KNOTS('',3,(#29728,#29729,#29730,#29731,#29732,
#29733,#29734,#29735,#29736,#29737,#29738,#29739,#29740,#29741,#29742,#29743,
#29744,#29745,#29746,#29747,#29748,#29749,#29750,#29751,#29752,#29753,#29754,
#29755,#29756,#29757,#29758,#29759,#29760,#29761,#29762,#29763,#29764,#29765,
#29766,#29767,#29768,#29769,#29770,#29771,#29772,#29773,#29774,#29775,#29776,
#29777,#29778,#29779),.UNSPECIFIED.,.F.,.F.,(4,3,3,3,3,3,3,3,3,3,3,3,3,
3,3,3,3,4),(0.,0.0290398589546008,0.0579843816831334,0.0868853129794548,
0.115761457357876,0.144631560789317,0.173538323016859,0.202474581669222,
0.231495438599218,0.249999999943415,0.279015696481709,0.307965888456467,
0.336869516660974,0.365745410794129,0.394622693781389,0.423510570114927,
0.452445568558316,0.460808762537663),.UNSPECIFIED.);
#1270=B_SPLINE_CURVE_WITH_KNOTS('',3,(#29900,#29901,#29902,#29903,#29904,
#29905,#29906,#29907,#29908,#29909,#29910,#29911,#29912,#29913,#29914,#29915,
#29916,#29917,#29918,#29919,#29920,#29921,#29922,#29923,#29924,#29925,#29926,
#29927,#29928,#29929,#29930,#29931,#29932,#29933,#29934,#29935,#29936,#29937,
#29938,#29939,#29940,#29941,#29942,#29943,#29944,#29945,#29946,#29947,#29948,
#29949,#29950,#29951),.UNSPECIFIED.,.F.,.F.,(4,3,3,3,3,3,3,3,3,3,3,3,3,
3,3,3,3,4),(0.,0.0290398589546263,0.0579843816831578,0.0868853129794855,
0.115761457357901,0.144631560789329,0.173538323016871,0.202474581669257,
0.231495438599254,0.249999999943415,0.279015696481705,0.307965888456485,
0.336869516661016,0.365745410794173,0.394622693781439,0.423510570114975,
0.452445568558338,0.460808762537663),.UNSPECIFIED.);
#1271=B_SPLINE_CURVE_WITH_KNOTS('',3,(#30207,#30208,#30209,#30210,#30211,
#30212,#30213,#30214),.UNSPECIFIED.,.F.,.F.,(4,2,2,4),(0.0783698352504338,
0.308777376437326,0.539184917624882,0.562623087291958),.UNSPECIFIED.);
#1272=B_SPLINE_CURVE_WITH_KNOTS('',3,(#30367,#30368,#30369,#30370,#30371,
#30372,#30373,#30374),.UNSPECIFIED.,.F.,.F.,(4,2,2,4),(0.0783698388401175,
0.308777379129589,0.539184919419725,0.562623088995283),.UNSPECIFIED.);
#1273=B_SPLINE_CURVE_WITH_KNOTS('',3,(#30535,#30536,#30537,#30538,#30539,
#30540,#30541,#30542),.UNSPECIFIED.,.F.,.F.,(4,2,2,4),(0.0783698437311044,
0.308777382797829,0.539184921865218,0.562623091316491),.UNSPECIFIED.);
#1274=B_SPLINE_CURVE_WITH_KNOTS('',3,(#30543,#30544,#30545,#30546,#30547,
#30548,#30549,#30550,#30551,#30552),.UNSPECIFIED.,.F.,.F.,(4,3,3,4),(0.078369843932103,
0.308777382798096,0.539184921865232,0.563918785527715),.UNSPECIFIED.);
#1275=B_SPLINE_CURVE_WITH_KNOTS('',3,(#30713,#30714,#30715,#30716,#30717,
#30718,#30719,#30720),.UNSPECIFIED.,.F.,.F.,(4,2,2,4),(0.0783698481609191,
0.30877738612019,0.539184924080125,0.5626230934188),.UNSPECIFIED.);
#1276=B_SPLINE_CURVE_WITH_KNOTS('',3,(#30873,#30874,#30875,#30876,#30877,
#30878,#30879,#30880),.UNSPECIFIED.,.F.,.F.,(4,2,2,4),(0.0783698504851113,
0.308777387863334,0.539184925242222,0.562623094521722),.UNSPECIFIED.);
#1277=B_SPLINE_CURVE_WITH_KNOTS('',3,(#31033,#31034,#31035,#31036,#31037,
#31038,#31039,#31040),.UNSPECIFIED.,.F.,.F.,(4,2,2,4),(0.0783698504851048,
0.308777387863329,0.539184925242218,0.562623094521906),.UNSPECIFIED.);
#1278=B_SPLINE_CURVE_WITH_KNOTS('',3,(#31193,#31194,#31195,#31196,#31197,
#31198,#31199,#31200),.UNSPECIFIED.,.F.,.F.,(4,2,2,4),(0.0783698481609166,
0.308777386120188,0.539184924080124,0.562623093418605),.UNSPECIFIED.);
#1279=B_SPLINE_CURVE_WITH_KNOTS('',3,(#31353,#31354,#31355,#31356,#31357,
#31358,#31359,#31360),.UNSPECIFIED.,.F.,.F.,(4,2,2,4),(0.0783698437311068,
0.308777382797831,0.539184921865219,0.56262309131643),.UNSPECIFIED.);
#1280=B_SPLINE_CURVE_WITH_KNOTS('',3,(#31513,#31514,#31515,#31516,#31517,
#31518,#31519,#31520),.UNSPECIFIED.,.F.,.F.,(4,2,2,4),(0.0783698388401241,
0.308777379129594,0.539184919419728,0.562623088995254),.UNSPECIFIED.);
#1281=B_SPLINE_CURVE_WITH_KNOTS('',3,(#31673,#31674,#31675,#31676,#31677,
#31678,#31679,#31680),.UNSPECIFIED.,.F.,.F.,(4,2,2,4),(0.0783698352504275,
0.308777376437321,0.539184917624879,0.562623087291614),.UNSPECIFIED.);
#1282=B_SPLINE_CURVE_WITH_KNOTS('',3,(#31833,#31834,#31835,#31836,#31837,
#31838,#31839,#31840),.UNSPECIFIED.,.F.,.F.,(4,2,2,4),(0.0783698293107417,
0.308777371982557,0.539184914655036,0.562623084473152),.UNSPECIFIED.);
#1283=B_SPLINE_CURVE_WITH_KNOTS('',3,(#32001,#32002,#32003,#32004,#32005,
#32006,#32007,#32008),.UNSPECIFIED.,.F.,.F.,(4,2,2,4),(0.0783698352504225,
0.308777376437317,0.539184917624877,0.562623087291754),.UNSPECIFIED.);
#1284=B_SPLINE_CURVE_WITH_KNOTS('',3,(#32009,#32010,#32011,#32012,#32013,
#32014,#32015,#32016,#32017,#32018),.UNSPECIFIED.,.F.,.F.,(4,3,3,4),(0.0783698354514212,
0.308777376437563,0.53918491762485,0.563918781514903),.UNSPECIFIED.);
#1285=B_SPLINE_CURVE_WITH_KNOTS('',3,(#32179,#32180,#32181,#32182,#32183,
#32184,#32185,#32186),.UNSPECIFIED.,.F.,.F.,(4,2,2,4),(0.0783698388401176,
0.308777379129589,0.539184919419725,0.562623088995512),.UNSPECIFIED.);
#1286=B_SPLINE_CURVE_WITH_KNOTS('',3,(#32339,#32340,#32341,#32342,#32343,
#32344,#32345,#32346),.UNSPECIFIED.,.F.,.F.,(4,2,2,4),(0.078369843731106,
0.30877738279783,0.539184921865219,0.56262309131667),.UNSPECIFIED.);
#1287=B_SPLINE_CURVE_WITH_KNOTS('',3,(#32555,#32556,#32557,#32558,#32559,
#32560,#32561,#32562),.UNSPECIFIED.,.F.,.F.,(4,2,2,4),(0.0783698481609151,
0.308777386120187,0.539184924080123,0.562623093418658),.UNSPECIFIED.);
#1288=B_SPLINE_CURVE_WITH_KNOTS('',3,(#32659,#32660,#32661,#32662,#32663,
#32664,#32665,#32666),.UNSPECIFIED.,.F.,.F.,(4,2,2,4),(0.0783698504851104,
0.308777387863333,0.539184925242221,0.562623094521848),.UNSPECIFIED.);
#1289=B_SPLINE_CURVE_WITH_KNOTS('',3,(#32819,#32820,#32821,#32822,#32823,
#32824,#32825,#32826),.UNSPECIFIED.,.F.,.F.,(4,2,2,4),(0.0783698504851007,
0.308777387863326,0.539184925242216,0.562623094521626),.UNSPECIFIED.);
#1290=B_SPLINE_CURVE_WITH_KNOTS('',3,(#32979,#32980,#32981,#32982,#32983,
#32984,#32985,#32986),.UNSPECIFIED.,.F.,.F.,(4,2,2,4),(0.0783698481609159,
0.308777386120187,0.539184924080124,0.562623093418695),.UNSPECIFIED.);
#1291=B_SPLINE_CURVE_WITH_KNOTS('',3,(#33139,#33140,#33141,#33142,#33143,
#33144,#33145,#33146),.UNSPECIFIED.,.F.,.F.,(4,2,2,4),(0.0783698437310911,
0.308777382797819,0.539184921865211,0.562623091316394),.UNSPECIFIED.);
#1292=B_SPLINE_CURVE_WITH_KNOTS('',3,(#33299,#33300,#33301,#33302,#33303,
#33304,#33305,#33306),.UNSPECIFIED.,.F.,.F.,(4,2,2,4),(0.0783698388401225,
0.308777379129592,0.539184919419727,0.562623088994977),.UNSPECIFIED.);
#1293=B_SPLINE_CURVE_WITH_KNOTS('',3,(#33459,#33460,#33461,#33462,#33463,
#33464,#33465,#33466),.UNSPECIFIED.,.F.,.F.,(4,2,2,4),(0.0783698352504349,
0.308777376437327,0.539184917624883,0.562623087291856),.UNSPECIFIED.);
#1294=B_SPLINE_CURVE_WITH_KNOTS('',3,(#33619,#33620,#33621,#33622,#33623,
#33624,#33625,#33626),.UNSPECIFIED.,.F.,.F.,(4,2,2,4),(0.0783698293107414,
0.308777371982556,0.539184914655036,0.562623084473124),.UNSPECIFIED.);
#1295=B_SPLINE_CURVE_WITH_KNOTS('',3,(#33779,#33780,#33781,#33782,#33783,
#33784,#33785,#33786),.UNSPECIFIED.,.F.,.F.,(4,2,2,4),(0.0783698352504222,
0.308777376437317,0.539184917624877,0.562623087291584),.UNSPECIFIED.);
#1296=B_SPLINE_CURVE_WITH_KNOTS('',3,(#33939,#33940,#33941,#33942,#33943,
#33944,#33945,#33946),.UNSPECIFIED.,.F.,.F.,(4,2,2,4),(0.078369838840123,
0.308777379129593,0.539184919419728,0.562623088995037),.UNSPECIFIED.);
#1297=B_SPLINE_CURVE_WITH_KNOTS('',3,(#34107,#34108,#34109,#34110,#34111,
#34112,#34113,#34114),.UNSPECIFIED.,.F.,.F.,(4,2,2,4),(0.0783698437311085,
0.308777382797832,0.53918492186522,0.562623091316454),.UNSPECIFIED.);
#1298=B_SPLINE_CURVE_WITH_KNOTS('',3,(#34115,#34116,#34117,#34118,#34119,
#34120,#34121,#34122,#34123,#34124),.UNSPECIFIED.,.F.,.F.,(4,3,3,4),(0.078369843932107,
0.308777382798091,0.539184921865221,0.563918785527689),.UNSPECIFIED.);
#1299=B_SPLINE_CURVE_WITH_KNOTS('',3,(#34293,#34294,#34295,#34296,#34297,
#34298,#34299,#34300),.UNSPECIFIED.,.F.,.F.,(4,2,2,4),(0.078369848160917,
0.308777386120188,0.539184924080124,0.562623093418646),.UNSPECIFIED.);
#1300=B_SPLINE_CURVE_WITH_KNOTS('',3,(#34301,#34302,#34303,#34304,#34305,
#34306,#34307,#34308,#34309,#34310),.UNSPECIFIED.,.F.,.F.,(4,3,3,4),(0.0783698483619153,
0.308777386120433,0.539184924080096,0.563918787623678),.UNSPECIFIED.);
#1301=B_SPLINE_CURVE_WITH_KNOTS('',3,(#34471,#34472,#34473,#34474,#34475,
#34476,#34477,#34478),.UNSPECIFIED.,.F.,.F.,(4,2,2,4),(0.0783698504850856,
0.308777387863315,0.539184925242209,0.56262309452169),.UNSPECIFIED.);
#1302=B_SPLINE_CURVE_WITH_KNOTS('',3,(#34631,#34632,#34633,#34634,#34635,
#34636,#34637,#34638),.UNSPECIFIED.,.F.,.F.,(4,2,2,4),(0.0783698504851055,
0.30877738786333,0.539184925242219,0.562623094521574),.UNSPECIFIED.);
#1303=B_SPLINE_CURVE_WITH_KNOTS('',3,(#34791,#34792,#34793,#34794,#34795,
#34796,#34797,#34798),.UNSPECIFIED.,.F.,.F.,(4,2,2,4),(0.0783698481609001,
0.308777386120176,0.539184924080116,0.562623093418498),.UNSPECIFIED.);
#1304=B_SPLINE_CURVE_WITH_KNOTS('',3,(#34951,#34952,#34953,#34954,#34955,
#34956,#34957,#34958),.UNSPECIFIED.,.F.,.F.,(4,2,2,4),(0.0783698437310988,
0.308777382797825,0.539184921865215,0.562623091316541),.UNSPECIFIED.);
#1305=B_SPLINE_CURVE_WITH_KNOTS('',3,(#35111,#35112,#35113,#35114,#35115,
#35116,#35117,#35118),.UNSPECIFIED.,.F.,.F.,(4,2,2,4),(0.0783698388401159,
0.308777379129587,0.539184919419724,0.562623088995074),.UNSPECIFIED.);
#1306=B_SPLINE_CURVE_WITH_KNOTS('',3,(#35271,#35272,#35273,#35274,#35275,
#35276,#35277,#35278),.UNSPECIFIED.,.F.,.F.,(4,2,2,4),(0.0783698352504283,
0.308777376437322,0.53918491762488,0.562623087291795),.UNSPECIFIED.);
#1307=B_SPLINE_CURVE_WITH_KNOTS('',3,(#35439,#35440,#35441,#35442,#35443,
#35444,#35445,#35446),.UNSPECIFIED.,.F.,.F.,(4,2,2,4),(0.0783698293107271,
0.308777371982546,0.53918491465503,0.562623084473022),.UNSPECIFIED.);
#1308=B_SPLINE_CURVE_WITH_KNOTS('',3,(#35447,#35448,#35449,#35450,#35451,
#35452,#35453,#35454,#35455,#35456),.UNSPECIFIED.,.F.,.F.,(4,3,3,4),(0.0783698295117259,
0.308777371982838,0.539184914655095,0.563918778704584),.UNSPECIFIED.);
#1309=B_SPLINE_CURVE_WITH_KNOTS('',3,(#35625,#35626,#35627,#35628,#35629,
#35630,#35631,#35632),.UNSPECIFIED.,.F.,.F.,(4,2,2,4),(0.0783698352504227,
0.308777376437317,0.539184917624878,0.56262308729164),.UNSPECIFIED.);
#1310=B_SPLINE_CURVE_WITH_KNOTS('',3,(#35633,#35634,#35635,#35636,#35637,
#35638,#35639,#35640,#35641,#35642),.UNSPECIFIED.,.F.,.F.,(4,3,3,4),(0.0783698354514214,
0.308777376437584,0.539184917624891,0.563918781514891),.UNSPECIFIED.);
#1311=B_SPLINE_CURVE_WITH_KNOTS('',3,(#35803,#35804,#35805,#35806,#35807,
#35808,#35809,#35810),.UNSPECIFIED.,.F.,.F.,(4,2,2,4),(0.078369838840114,
0.308777379129586,0.539184919419723,0.562623088995413),.UNSPECIFIED.);
#1312=B_SPLINE_CURVE_WITH_KNOTS('',3,(#35963,#35964,#35965,#35966,#35967,
#35968,#35969,#35970),.UNSPECIFIED.,.F.,.F.,(4,2,2,4),(0.078369843731106,
0.30877738279783,0.539184921865219,0.562623091316345),.UNSPECIFIED.);
#1313=B_SPLINE_CURVE_WITH_KNOTS('',3,(#36179,#36180,#36181,#36182,#36183,
#36184,#36185,#36186),.UNSPECIFIED.,.F.,.F.,(4,2,2,4),(0.0783698481609172,
0.308777386120188,0.539184924080125,0.562623093418633),.UNSPECIFIED.);
#1314=B_SPLINE_CURVE_WITH_KNOTS('',3,(#36283,#36284,#36285,#36286,#36287,
#36288,#36289,#36290),.UNSPECIFIED.,.F.,.F.,(4,2,2,4),(0.0783698504850854,
0.308777387863314,0.539184925242208,0.562623094521865),.UNSPECIFIED.);
#1315=B_SPLINE_CURVE_WITH_KNOTS('',3,(#36443,#36444,#36445,#36446,#36447,
#36448,#36449,#36450),.UNSPECIFIED.,.F.,.F.,(4,2,2,4),(0.0783698504851049,
0.308777387863329,0.539184925242218,0.562623094521782),.UNSPECIFIED.);
#1316=B_SPLINE_CURVE_WITH_KNOTS('',3,(#36603,#36604,#36605,#36606,#36607,
#36608,#36609,#36610),.UNSPECIFIED.,.F.,.F.,(4,2,2,4),(0.0783698481609187,
0.30877738612019,0.539184924080125,0.562623093418547),.UNSPECIFIED.);
#1317=B_SPLINE_CURVE_WITH_KNOTS('',3,(#36763,#36764,#36765,#36766,#36767,
#36768,#36769,#36770),.UNSPECIFIED.,.F.,.F.,(4,2,2,4),(0.0783698437311104,
0.308777382797833,0.539184921865221,0.562623091316399),.UNSPECIFIED.);
#1318=B_SPLINE_CURVE_WITH_KNOTS('',3,(#36923,#36924,#36925,#36926,#36927,
#36928,#36929,#36930),.UNSPECIFIED.,.F.,.F.,(4,2,2,4),(0.0783698388401129,
0.308777379129585,0.539184919419723,0.562623088995376),.UNSPECIFIED.);
#1319=B_SPLINE_CURVE_WITH_KNOTS('',3,(#37091,#37092,#37093,#37094,#37095,
#37096,#37097,#37098),.UNSPECIFIED.,.F.,.F.,(4,2,2,4),(0.0783698352504293,
0.308777376437322,0.53918491762488,0.562623087291725),.UNSPECIFIED.);
#1320=B_SPLINE_CURVE_WITH_KNOTS('',3,(#37099,#37100,#37101,#37102,#37103,
#37104,#37105,#37106,#37107,#37108),.UNSPECIFIED.,.F.,.F.,(4,3,3,4),(0.078369835451428,
0.308777376437561,0.539184917624838,0.563918781514903),.UNSPECIFIED.);
#1321=SHAPE_REPRESENTATION_RELATIONSHIP('SRR','None',#37954,#1333);
#1322=SHAPE_REPRESENTATION_RELATIONSHIP('SRR','None',#37955,#1334);
#1323=SHAPE_REPRESENTATION_RELATIONSHIP('SRR','None',#37956,#1335);
#1324=SHAPE_REPRESENTATION_RELATIONSHIP('SRR','None',#37957,#1336);
#1325=SHAPE_REPRESENTATION_RELATIONSHIP('SRR','None',#37958,#1337);
#1326=SHAPE_REPRESENTATION_RELATIONSHIP('SRR','None',#37959,#1338);
#1327=SHAPE_REPRESENTATION_RELATIONSHIP('SRR','None',#37960,#1339);
#1328=SHAPE_REPRESENTATION_RELATIONSHIP('SRR','None',#37961,#1340);
#1329=SHAPE_REPRESENTATION_RELATIONSHIP('SRR','None',#37962,#1341);
#1330=SHAPE_REPRESENTATION_RELATIONSHIP('SRR','None',#37963,#1342);
#1331=SHAPE_REPRESENTATION_RELATIONSHIP('SRR','None',#37964,#1343);
#1332=SHAPE_REPRESENTATION_RELATIONSHIP('SRR','None',#37965,#1344);
#1333=ADVANCED_BREP_SHAPE_REPRESENTATION('',(#1357),#37869);
#1334=ADVANCED_BREP_SHAPE_REPRESENTATION('',(#1358),#37870);
#1335=ADVANCED_BREP_SHAPE_REPRESENTATION('',(#1359),#37871);
#1336=ADVANCED_BREP_SHAPE_REPRESENTATION('',(#1360),#37872);
#1337=ADVANCED_BREP_SHAPE_REPRESENTATION('',(#1361),#37873);
#1338=ADVANCED_BREP_SHAPE_REPRESENTATION('',(#1362),#37874);
#1339=ADVANCED_BREP_SHAPE_REPRESENTATION('',(#1363),#37875);
#1340=ADVANCED_BREP_SHAPE_REPRESENTATION('',(#1364),#37876);
#1341=ADVANCED_BREP_SHAPE_REPRESENTATION('',(#1365),#37877);
#1342=ADVANCED_BREP_SHAPE_REPRESENTATION('',(#1366),#37878);
#1343=ADVANCED_BREP_SHAPE_REPRESENTATION('',(#1367),#37879);
#1344=ADVANCED_BREP_SHAPE_REPRESENTATION('',(#1368),#37880);
#1345=STYLED_ITEM('',(#38023),#1357);
#1346=STYLED_ITEM('',(#38023),#1358);
#1347=STYLED_ITEM('',(#38023),#1359);
#1348=STYLED_ITEM('',(#38023),#1360);
#1349=STYLED_ITEM('',(#38023),#1361);
#1350=STYLED_ITEM('',(#38023),#1362);
#1351=STYLED_ITEM('',(#38023),#1363);
#1352=STYLED_ITEM('',(#38023),#1364);
#1353=STYLED_ITEM('',(#38023),#1365);
#1354=STYLED_ITEM('',(#38023),#1366);
#1355=STYLED_ITEM('',(#38023),#1367);
#1356=STYLED_ITEM('',(#38023),#1368);
#1357=MANIFOLD_SOLID_BREP('Body1',#10819);
#1358=MANIFOLD_SOLID_BREP('Body1',#10820);
#1359=MANIFOLD_SOLID_BREP('Body1',#10821);
#1360=MANIFOLD_SOLID_BREP('Body1',#10822);
#1361=MANIFOLD_SOLID_BREP('Body1',#10823);
#1362=MANIFOLD_SOLID_BREP('Body1',#10824);
#1363=MANIFOLD_SOLID_BREP('Body1',#10825);
#1364=MANIFOLD_SOLID_BREP('Body1',#10826);
#1365=MANIFOLD_SOLID_BREP('Body1',#10827);
#1366=MANIFOLD_SOLID_BREP('Body1',#10828);
#1367=MANIFOLD_SOLID_BREP('Body1',#10829);
#1368=MANIFOLD_SOLID_BREP('Body1',#10830);
#1369=ELLIPSE('',#11034,4.24264068711896,2.99999999999969);
#1370=ELLIPSE('',#11035,4.24264068711823,2.99999999999929);
#1371=ELLIPSE('',#11037,4.24264068711881,2.99999999999963);
#1372=ELLIPSE('',#11039,4.24264068711841,2.99999999999935);
#1373=ELLIPSE('',#11682,4.24264068711892,2.99999999999971);
#1374=ELLIPSE('',#11683,4.24264068711757,2.99999999999883);
#1375=ELLIPSE('',#11685,4.24264068711876,2.99999999999963);
#1376=ELLIPSE('',#11687,4.24264068711788,2.99999999999899);
#1377=FACE_BOUND('',#2191,.T.);
#1378=FACE_BOUND('',#2192,.T.);
#1379=FACE_BOUND('',#2195,.T.);
#1380=FACE_BOUND('',#2196,.T.);
#1381=FACE_BOUND('',#2200,.T.);
#1382=FACE_BOUND('',#2201,.T.);
#1383=FACE_BOUND('',#2204,.T.);
#1384=FACE_BOUND('',#2205,.T.);
#1385=FACE_BOUND('',#2208,.T.);
#1386=FACE_BOUND('',#2209,.T.);
#1387=FACE_BOUND('',#2210,.T.);
#1388=FACE_BOUND('',#2211,.T.);
#1389=FACE_BOUND('',#2212,.T.);
#1390=FACE_BOUND('',#2213,.T.);
#1391=FACE_BOUND('',#2214,.T.);
#1392=FACE_BOUND('',#2216,.T.);
#1393=FACE_BOUND('',#2217,.T.);
#1394=FACE_BOUND('',#2218,.T.);
#1395=FACE_BOUND('',#2219,.T.);
#1396=FACE_BOUND('',#2220,.T.);
#1397=FACE_BOUND('',#2221,.T.);
#1398=FACE_BOUND('',#2222,.T.);
#1399=FACE_BOUND('',#2246,.T.);
#1400=FACE_BOUND('',#2248,.T.);
#1401=FACE_BOUND('',#2250,.T.);
#1402=FACE_BOUND('',#2276,.T.);
#1403=FACE_BOUND('',#2278,.T.);
#1404=FACE_BOUND('',#2280,.T.);
#1405=FACE_BOUND('',#2421,.T.);
#1406=FACE_BOUND('',#2423,.T.);
#1407=FACE_BOUND('',#2710,.T.);
#1408=FACE_BOUND('',#2711,.T.);
#1409=FACE_BOUND('',#2714,.T.);
#1410=FACE_BOUND('',#2715,.T.);
#1411=FACE_BOUND('',#2718,.T.);
#1412=FACE_BOUND('',#2720,.T.);
#1413=FACE_BOUND('',#2721,.T.);
#1414=FACE_BOUND('',#2723,.T.);
#1415=FACE_BOUND('',#2725,.T.);
#1416=FACE_BOUND('',#2726,.T.);
#1417=FACE_BOUND('',#2729,.T.);
#1418=FACE_BOUND('',#2730,.T.);
#1419=FACE_BOUND('',#2731,.T.);
#1420=FACE_BOUND('',#2732,.T.);
#1421=FACE_BOUND('',#2733,.T.);
#1422=FACE_BOUND('',#2734,.T.);
#1423=FACE_BOUND('',#2735,.T.);
#1424=FACE_BOUND('',#2736,.T.);
#1425=FACE_BOUND('',#2738,.T.);
#1426=FACE_BOUND('',#2739,.T.);
#1427=FACE_BOUND('',#2740,.T.);
#1428=FACE_BOUND('',#2741,.T.);
#1429=FACE_BOUND('',#2742,.T.);
#1430=FACE_BOUND('',#2743,.T.);
#1431=FACE_BOUND('',#2744,.T.);
#1432=FACE_BOUND('',#2745,.T.);
#1433=FACE_BOUND('',#2791,.T.);
#1434=FACE_BOUND('',#2792,.T.);
#1435=FACE_BOUND('',#2793,.T.);
#1436=FACE_BOUND('',#2794,.T.);
#1437=FACE_BOUND('',#2795,.T.);
#1438=FACE_BOUND('',#2796,.T.);
#1439=FACE_BOUND('',#2797,.T.);
#1440=FACE_BOUND('',#2799,.T.);
#1441=FACE_BOUND('',#2800,.T.);
#1442=FACE_BOUND('',#2801,.T.);
#1443=FACE_BOUND('',#2802,.T.);
#1444=FACE_BOUND('',#2803,.T.);
#1445=FACE_BOUND('',#2804,.T.);
#1446=FACE_BOUND('',#2805,.T.);
#1447=FACE_BOUND('',#2815,.T.);
#1448=FACE_BOUND('',#2816,.T.);
#1449=FACE_BOUND('',#2817,.T.);
#1450=FACE_BOUND('',#2818,.T.);
#1451=FACE_BOUND('',#2819,.T.);
#1452=FACE_BOUND('',#2820,.T.);
#1453=FACE_BOUND('',#2821,.T.);
#1454=FACE_BOUND('',#2823,.T.);
#1455=FACE_BOUND('',#2824,.T.);
#1456=FACE_BOUND('',#2825,.T.);
#1457=FACE_BOUND('',#2826,.T.);
#1458=FACE_BOUND('',#2827,.T.);
#1459=FACE_BOUND('',#2828,.T.);
#1460=FACE_BOUND('',#2829,.T.);
#1461=FACE_BOUND('',#2837,.T.);
#1462=FACE_BOUND('',#2846,.T.);
#1463=FACE_BOUND('',#2868,.T.);
#1464=FACE_BOUND('',#2870,.T.);
#1465=PLANE('',#10999);
#1466=PLANE('',#11000);
#1467=PLANE('',#11001);
#1468=PLANE('',#11002);
#1469=PLANE('',#11003);
#1470=PLANE('',#11004);
#1471=PLANE('',#11008);
#1472=PLANE('',#11009);
#1473=PLANE('',#11013);
#1474=PLANE('',#11014);
#1475=PLANE('',#11015);
#1476=PLANE('',#11019);
#1477=PLANE('',#11020);
#1478=PLANE('',#11024);
#1479=PLANE('',#11025);
#1480=PLANE('',#11026);
#1481=PLANE('',#11066);
#1482=PLANE('',#11067);
#1483=PLANE('',#11068);
#1484=PLANE('',#11069);
#1485=PLANE('',#11072);
#1486=PLANE('',#11074);
#1487=PLANE('',#11075);
#1488=PLANE('',#11076);
#1489=PLANE('',#11077);
#1490=PLANE('',#11078);
#1491=PLANE('',#11079);
#1492=PLANE('',#11098);
#1493=PLANE('',#11099);
#1494=PLANE('',#11100);
#1495=PLANE('',#11101);
#1496=PLANE('',#11102);
#1497=PLANE('',#11103);
#1498=PLANE('',#11104);
#1499=PLANE('',#11105);
#1500=PLANE('',#11106);
#1501=PLANE('',#11107);
#1502=PLANE('',#11108);
#1503=PLANE('',#11109);
#1504=PLANE('',#11426);
#1505=PLANE('',#11427);
#1506=PLANE('',#11428);
#1507=PLANE('',#11429);
#1508=PLANE('',#11430);
#1509=PLANE('',#11647);
#1510=PLANE('',#11648);
#1511=PLANE('',#11649);
#1512=PLANE('',#11650);
#1513=PLANE('',#11651);
#1514=PLANE('',#11652);
#1515=PLANE('',#11656);
#1516=PLANE('',#11657);
#1517=PLANE('',#11661);
#1518=PLANE('',#11662);
#1519=PLANE('',#11663);
#1520=PLANE('',#11667);
#1521=PLANE('',#11668);
#1522=PLANE('',#11672);
#1523=PLANE('',#11673);
#1524=PLANE('',#11674);
#1525=PLANE('',#11690);
#1526=PLANE('',#11691);
#1527=PLANE('',#11692);
#1528=PLANE('',#11693);
#1529=PLANE('',#11694);
#1530=PLANE('',#11695);
#1531=PLANE('',#11765);
#1532=PLANE('',#11766);
#1533=PLANE('',#11792);
#1534=PLANE('',#11793);
#1535=PLANE('',#11807);
#1536=PLANE('',#11808);
#1537=PLANE('',#11809);
#1538=PLANE('',#11814);
#1539=PLANE('',#11815);
#1540=PLANE('',#11816);
#1541=PLANE('',#11817);
#1542=PLANE('',#11818);
#1543=PLANE('',#11819);
#1544=PLANE('',#11820);
#1545=PLANE('',#11821);
#1546=PLANE('',#11822);
#1547=PLANE('',#11824);
#1548=PLANE('',#11825);
#1549=PLANE('',#11826);
#1550=PLANE('',#11827);
#1551=PLANE('',#11828);
#1552=PLANE('',#11829);
#1553=PLANE('',#11830);
#1554=PLANE('',#11831);
#1555=PLANE('',#11832);
#1556=PLANE('',#11833);
#1557=PLANE('',#11834);
#1558=PLANE('',#11835);
#1559=PLANE('',#11836);
#1560=PLANE('',#11837);
#1561=PLANE('',#11838);
#1562=PLANE('',#11839);
#1563=PLANE('',#11847);
#1564=PLANE('',#11848);
#1565=FACE_OUTER_BOUND('',#2174,.T.);
#1566=FACE_OUTER_BOUND('',#2175,.T.);
#1567=FACE_OUTER_BOUND('',#2176,.T.);
#1568=FACE_OUTER_BOUND('',#2177,.T.);
#1569=FACE_OUTER_BOUND('',#2178,.T.);
#1570=FACE_OUTER_BOUND('',#2179,.T.);
#1571=FACE_OUTER_BOUND('',#2180,.T.);
#1572=FACE_OUTER_BOUND('',#2181,.T.);
#1573=FACE_OUTER_BOUND('',#2182,.T.);
#1574=FACE_OUTER_BOUND('',#2183,.T.);
#1575=FACE_OUTER_BOUND('',#2184,.T.);
#1576=FACE_OUTER_BOUND('',#2185,.T.);
#1577=FACE_OUTER_BOUND('',#2186,.T.);
#1578=FACE_OUTER_BOUND('',#2187,.T.);
#1579=FACE_OUTER_BOUND('',#2188,.T.);
#1580=FACE_OUTER_BOUND('',#2189,.T.);
#1581=FACE_OUTER_BOUND('',#2190,.T.);
#1582=FACE_OUTER_BOUND('',#2193,.T.);
#1583=FACE_OUTER_BOUND('',#2194,.T.);
#1584=FACE_OUTER_BOUND('',#2197,.T.);
#1585=FACE_OUTER_BOUND('',#2198,.T.);
#1586=FACE_OUTER_BOUND('',#2199,.T.);
#1587=FACE_OUTER_BOUND('',#2202,.T.);
#1588=FACE_OUTER_BOUND('',#2203,.T.);
#1589=FACE_OUTER_BOUND('',#2206,.T.);
#1590=FACE_OUTER_BOUND('',#2207,.T.);
#1591=FACE_OUTER_BOUND('',#2215,.T.);
#1592=FACE_OUTER_BOUND('',#2223,.T.);
#1593=FACE_OUTER_BOUND('',#2224,.T.);
#1594=FACE_OUTER_BOUND('',#2225,.T.);
#1595=FACE_OUTER_BOUND('',#2226,.T.);
#1596=FACE_OUTER_BOUND('',#2227,.T.);
#1597=FACE_OUTER_BOUND('',#2228,.T.);
#1598=FACE_OUTER_BOUND('',#2229,.T.);
#1599=FACE_OUTER_BOUND('',#2230,.T.);
#1600=FACE_OUTER_BOUND('',#2231,.T.);
#1601=FACE_OUTER_BOUND('',#2232,.T.);
#1602=FACE_OUTER_BOUND('',#2233,.T.);
#1603=FACE_OUTER_BOUND('',#2234,.T.);
#1604=FACE_OUTER_BOUND('',#2235,.T.);
#1605=FACE_OUTER_BOUND('',#2236,.T.);
#1606=FACE_OUTER_BOUND('',#2237,.T.);
#1607=FACE_OUTER_BOUND('',#2238,.T.);
#1608=FACE_OUTER_BOUND('',#2239,.T.);
#1609=FACE_OUTER_BOUND('',#2240,.T.);
#1610=FACE_OUTER_BOUND('',#2241,.T.);
#1611=FACE_OUTER_BOUND('',#2242,.T.);
#1612=FACE_OUTER_BOUND('',#2243,.T.);
#1613=FACE_OUTER_BOUND('',#2244,.T.);
#1614=FACE_OUTER_BOUND('',#2245,.T.);
#1615=FACE_OUTER_BOUND('',#2247,.T.);
#1616=FACE_OUTER_BOUND('',#2249,.T.);
#1617=FACE_OUTER_BOUND('',#2251,.T.);
#1618=FACE_OUTER_BOUND('',#2252,.T.);
#1619=FACE_OUTER_BOUND('',#2253,.T.);
#1620=FACE_OUTER_BOUND('',#2254,.T.);
#1621=FACE_OUTER_BOUND('',#2255,.T.);
#1622=FACE_OUTER_BOUND('',#2256,.T.);
#1623=FACE_OUTER_BOUND('',#2257,.T.);
#1624=FACE_OUTER_BOUND('',#2258,.T.);
#1625=FACE_OUTER_BOUND('',#2259,.T.);
#1626=FACE_OUTER_BOUND('',#2260,.T.);
#1627=FACE_OUTER_BOUND('',#2261,.T.);
#1628=FACE_OUTER_BOUND('',#2262,.T.);
#1629=FACE_OUTER_BOUND('',#2263,.T.);
#1630=FACE_OUTER_BOUND('',#2264,.T.);
#1631=FACE_OUTER_BOUND('',#2265,.T.);
#1632=FACE_OUTER_BOUND('',#2266,.T.);
#1633=FACE_OUTER_BOUND('',#2267,.T.);
#1634=FACE_OUTER_BOUND('',#2268,.T.);
#1635=FACE_OUTER_BOUND('',#2269,.T.);
#1636=FACE_OUTER_BOUND('',#2270,.T.);
#1637=FACE_OUTER_BOUND('',#2271,.T.);
#1638=FACE_OUTER_BOUND('',#2272,.T.);
#1639=FACE_OUTER_BOUND('',#2273,.T.);
#1640=FACE_OUTER_BOUND('',#2274,.T.);
#1641=FACE_OUTER_BOUND('',#2275,.T.);
#1642=FACE_OUTER_BOUND('',#2277,.T.);
#1643=FACE_OUTER_BOUND('',#2279,.T.);
#1644=FACE_OUTER_BOUND('',#2281,.T.);
#1645=FACE_OUTER_BOUND('',#2282,.T.);
#1646=FACE_OUTER_BOUND('',#2283,.T.);
#1647=FACE_OUTER_BOUND('',#2284,.T.);
#1648=FACE_OUTER_BOUND('',#2285,.T.);
#1649=FACE_OUTER_BOUND('',#2286,.T.);
#1650=FACE_OUTER_BOUND('',#2287,.T.);
#1651=FACE_OUTER_BOUND('',#2288,.T.);
#1652=FACE_OUTER_BOUND('',#2289,.T.);
#1653=FACE_OUTER_BOUND('',#2290,.T.);
#1654=FACE_OUTER_BOUND('',#2291,.T.);
#1655=FACE_OUTER_BOUND('',#2292,.T.);
#1656=FACE_OUTER_BOUND('',#2293,.T.);
#1657=FACE_OUTER_BOUND('',#2294,.T.);
#1658=FACE_OUTER_BOUND('',#2295,.T.);
#1659=FACE_OUTER_BOUND('',#2296,.T.);
#1660=FACE_OUTER_BOUND('',#2297,.T.);
#1661=FACE_OUTER_BOUND('',#2298,.T.);
#1662=FACE_OUTER_BOUND('',#2299,.T.);
#1663=FACE_OUTER_BOUND('',#2300,.T.);
#1664=FACE_OUTER_BOUND('',#2301,.T.);
#1665=FACE_OUTER_BOUND('',#2302,.T.);
#1666=FACE_OUTER_BOUND('',#2303,.T.);
#1667=FACE_OUTER_BOUND('',#2304,.T.);
#1668=FACE_OUTER_BOUND('',#2305,.T.);
#1669=FACE_OUTER_BOUND('',#2306,.T.);
#1670=FACE_OUTER_BOUND('',#2307,.T.);
#1671=FACE_OUTER_BOUND('',#2308,.T.);
#1672=FACE_OUTER_BOUND('',#2309,.T.);
#1673=FACE_OUTER_BOUND('',#2310,.T.);
#1674=FACE_OUTER_BOUND('',#2311,.T.);
#1675=FACE_OUTER_BOUND('',#2312,.T.);
#1676=FACE_OUTER_BOUND('',#2313,.T.);
#1677=FACE_OUTER_BOUND('',#2314,.T.);
#1678=FACE_OUTER_BOUND('',#2315,.T.);
#1679=FACE_OUTER_BOUND('',#2316,.T.);
#1680=FACE_OUTER_BOUND('',#2317,.T.);
#1681=FACE_OUTER_BOUND('',#2318,.T.);
#1682=FACE_OUTER_BOUND('',#2319,.T.);
#1683=FACE_OUTER_BOUND('',#2320,.T.);
#1684=FACE_OUTER_BOUND('',#2321,.T.);
#1685=FACE_OUTER_BOUND('',#2322,.T.);
#1686=FACE_OUTER_BOUND('',#2323,.T.);
#1687=FACE_OUTER_BOUND('',#2324,.T.);
#1688=FACE_OUTER_BOUND('',#2325,.T.);
#1689=FACE_OUTER_BOUND('',#2326,.T.);
#1690=FACE_OUTER_BOUND('',#2327,.T.);
#1691=FACE_OUTER_BOUND('',#2328,.T.);
#1692=FACE_OUTER_BOUND('',#2329,.T.);
#1693=FACE_OUTER_BOUND('',#2330,.T.);
#1694=FACE_OUTER_BOUND('',#2331,.T.);
#1695=FACE_OUTER_BOUND('',#2332,.T.);
#1696=FACE_OUTER_BOUND('',#2333,.T.);
#1697=FACE_OUTER_BOUND('',#2334,.T.);
#1698=FACE_OUTER_BOUND('',#2335,.T.);
#1699=FACE_OUTER_BOUND('',#2336,.T.);
#1700=FACE_OUTER_BOUND('',#2337,.T.);
#1701=FACE_OUTER_BOUND('',#2338,.T.);
#1702=FACE_OUTER_BOUND('',#2339,.T.);
#1703=FACE_OUTER_BOUND('',#2340,.T.);
#1704=FACE_OUTER_BOUND('',#2341,.T.);
#1705=FACE_OUTER_BOUND('',#2342,.T.);
#1706=FACE_OUTER_BOUND('',#2343,.T.);
#1707=FACE_OUTER_BOUND('',#2344,.T.);
#1708=FACE_OUTER_BOUND('',#2345,.T.);
#1709=FACE_OUTER_BOUND('',#2346,.T.);
#1710=FACE_OUTER_BOUND('',#2347,.T.);
#1711=FACE_OUTER_BOUND('',#2348,.T.);
#1712=FACE_OUTER_BOUND('',#2349,.T.);
#1713=FACE_OUTER_BOUND('',#2350,.T.);
#1714=FACE_OUTER_BOUND('',#2351,.T.);
#1715=FACE_OUTER_BOUND('',#2352,.T.);
#1716=FACE_OUTER_BOUND('',#2353,.T.);
#1717=FACE_OUTER_BOUND('',#2354,.T.);
#1718=FACE_OUTER_BOUND('',#2355,.T.);
#1719=FACE_OUTER_BOUND('',#2356,.T.);
#1720=FACE_OUTER_BOUND('',#2357,.T.);
#1721=FACE_OUTER_BOUND('',#2358,.T.);
#1722=FACE_OUTER_BOUND('',#2359,.T.);
#1723=FACE_OUTER_BOUND('',#2360,.T.);
#1724=FACE_OUTER_BOUND('',#2361,.T.);
#1725=FACE_OUTER_BOUND('',#2362,.T.);
#1726=FACE_OUTER_BOUND('',#2363,.T.);
#1727=FACE_OUTER_BOUND('',#2364,.T.);
#1728=FACE_OUTER_BOUND('',#2365,.T.);
#1729=FACE_OUTER_BOUND('',#2366,.T.);
#1730=FACE_OUTER_BOUND('',#2367,.T.);
#1731=FACE_OUTER_BOUND('',#2368,.T.);
#1732=FACE_OUTER_BOUND('',#2369,.T.);
#1733=FACE_OUTER_BOUND('',#2370,.T.);
#1734=FACE_OUTER_BOUND('',#2371,.T.);
#1735=FACE_OUTER_BOUND('',#2372,.T.);
#1736=FACE_OUTER_BOUND('',#2373,.T.);
#1737=FACE_OUTER_BOUND('',#2374,.T.);
#1738=FACE_OUTER_BOUND('',#2375,.T.);
#1739=FACE_OUTER_BOUND('',#2376,.T.);
#1740=FACE_OUTER_BOUND('',#2377,.T.);
#1741=FACE_OUTER_BOUND('',#2378,.T.);
#1742=FACE_OUTER_BOUND('',#2379,.T.);
#1743=FACE_OUTER_BOUND('',#2380,.T.);
#1744=FACE_OUTER_BOUND('',#2381,.T.);
#1745=FACE_OUTER_BOUND('',#2382,.T.);
#1746=FACE_OUTER_BOUND('',#2383,.T.);
#1747=FACE_OUTER_BOUND('',#2384,.T.);
#1748=FACE_OUTER_BOUND('',#2385,.T.);
#1749=FACE_OUTER_BOUND('',#2386,.T.);
#1750=FACE_OUTER_BOUND('',#2387,.T.);
#1751=FACE_OUTER_BOUND('',#2388,.T.);
#1752=FACE_OUTER_BOUND('',#2389,.T.);
#1753=FACE_OUTER_BOUND('',#2390,.T.);
#1754=FACE_OUTER_BOUND('',#2391,.T.);
#1755=FACE_OUTER_BOUND('',#2392,.T.);
#1756=FACE_OUTER_BOUND('',#2393,.T.);
#1757=FACE_OUTER_BOUND('',#2394,.T.);
#1758=FACE_OUTER_BOUND('',#2395,.T.);
#1759=FACE_OUTER_BOUND('',#2396,.T.);
#1760=FACE_OUTER_BOUND('',#2397,.T.);
#1761=FACE_OUTER_BOUND('',#2398,.T.);
#1762=FACE_OUTER_BOUND('',#2399,.T.);
#1763=FACE_OUTER_BOUND('',#2400,.T.);
#1764=FACE_OUTER_BOUND('',#2401,.T.);
#1765=FACE_OUTER_BOUND('',#2402,.T.);
#1766=FACE_OUTER_BOUND('',#2403,.T.);
#1767=FACE_OUTER_BOUND('',#2404,.T.);
#1768=FACE_OUTER_BOUND('',#2405,.T.);
#1769=FACE_OUTER_BOUND('',#2406,.T.);
#1770=FACE_OUTER_BOUND('',#2407,.T.);
#1771=FACE_OUTER_BOUND('',#2408,.T.);
#1772=FACE_OUTER_BOUND('',#2409,.T.);
#1773=FACE_OUTER_BOUND('',#2410,.T.);
#1774=FACE_OUTER_BOUND('',#2411,.T.);
#1775=FACE_OUTER_BOUND('',#2412,.T.);
#1776=FACE_OUTER_BOUND('',#2413,.T.);
#1777=FACE_OUTER_BOUND('',#2414,.T.);
#1778=FACE_OUTER_BOUND('',#2415,.T.);
#1779=FACE_OUTER_BOUND('',#2416,.T.);
#1780=FACE_OUTER_BOUND('',#2417,.T.);
#1781=FACE_OUTER_BOUND('',#2418,.T.);
#1782=FACE_OUTER_BOUND('',#2419,.T.);
#1783=FACE_OUTER_BOUND('',#2420,.T.);
#1784=FACE_OUTER_BOUND('',#2422,.T.);
#1785=FACE_OUTER_BOUND('',#2424,.T.);
#1786=FACE_OUTER_BOUND('',#2425,.T.);
#1787=FACE_OUTER_BOUND('',#2426,.T.);
#1788=FACE_OUTER_BOUND('',#2427,.T.);
#1789=FACE_OUTER_BOUND('',#2428,.T.);
#1790=FACE_OUTER_BOUND('',#2429,.T.);
#1791=FACE_OUTER_BOUND('',#2430,.T.);
#1792=FACE_OUTER_BOUND('',#2431,.T.);
#1793=FACE_OUTER_BOUND('',#2432,.T.);
#1794=FACE_OUTER_BOUND('',#2433,.T.);
#1795=FACE_OUTER_BOUND('',#2434,.T.);
#1796=FACE_OUTER_BOUND('',#2435,.T.);
#1797=FACE_OUTER_BOUND('',#2436,.T.);
#1798=FACE_OUTER_BOUND('',#2437,.T.);
#1799=FACE_OUTER_BOUND('',#2438,.T.);
#1800=FACE_OUTER_BOUND('',#2439,.T.);
#1801=FACE_OUTER_BOUND('',#2440,.T.);
#1802=FACE_OUTER_BOUND('',#2441,.T.);
#1803=FACE_OUTER_BOUND('',#2442,.T.);
#1804=FACE_OUTER_BOUND('',#2443,.T.);
#1805=FACE_OUTER_BOUND('',#2444,.T.);
#1806=FACE_OUTER_BOUND('',#2445,.T.);
#1807=FACE_OUTER_BOUND('',#2446,.T.);
#1808=FACE_OUTER_BOUND('',#2447,.T.);
#1809=FACE_OUTER_BOUND('',#2448,.T.);
#1810=FACE_OUTER_BOUND('',#2449,.T.);
#1811=FACE_OUTER_BOUND('',#2450,.T.);
#1812=FACE_OUTER_BOUND('',#2451,.T.);
#1813=FACE_OUTER_BOUND('',#2452,.T.);
#1814=FACE_OUTER_BOUND('',#2453,.T.);
#1815=FACE_OUTER_BOUND('',#2454,.T.);
#1816=FACE_OUTER_BOUND('',#2455,.T.);
#1817=FACE_OUTER_BOUND('',#2456,.T.);
#1818=FACE_OUTER_BOUND('',#2457,.T.);
#1819=FACE_OUTER_BOUND('',#2458,.T.);
#1820=FACE_OUTER_BOUND('',#2459,.T.);
#1821=FACE_OUTER_BOUND('',#2460,.T.);
#1822=FACE_OUTER_BOUND('',#2461,.T.);
#1823=FACE_OUTER_BOUND('',#2462,.T.);
#1824=FACE_OUTER_BOUND('',#2463,.T.);
#1825=FACE_OUTER_BOUND('',#2464,.T.);
#1826=FACE_OUTER_BOUND('',#2465,.T.);
#1827=FACE_OUTER_BOUND('',#2466,.T.);
#1828=FACE_OUTER_BOUND('',#2467,.T.);
#1829=FACE_OUTER_BOUND('',#2468,.T.);
#1830=FACE_OUTER_BOUND('',#2469,.T.);
#1831=FACE_OUTER_BOUND('',#2470,.T.);
#1832=FACE_OUTER_BOUND('',#2471,.T.);
#1833=FACE_OUTER_BOUND('',#2472,.T.);
#1834=FACE_OUTER_BOUND('',#2473,.T.);
#1835=FACE_OUTER_BOUND('',#2474,.T.);
#1836=FACE_OUTER_BOUND('',#2475,.T.);
#1837=FACE_OUTER_BOUND('',#2476,.T.);
#1838=FACE_OUTER_BOUND('',#2477,.T.);
#1839=FACE_OUTER_BOUND('',#2478,.T.);
#1840=FACE_OUTER_BOUND('',#2479,.T.);
#1841=FACE_OUTER_BOUND('',#2480,.T.);
#1842=FACE_OUTER_BOUND('',#2481,.T.);
#1843=FACE_OUTER_BOUND('',#2482,.T.);
#1844=FACE_OUTER_BOUND('',#2483,.T.);
#1845=FACE_OUTER_BOUND('',#2484,.T.);
#1846=FACE_OUTER_BOUND('',#2485,.T.);
#1847=FACE_OUTER_BOUND('',#2486,.T.);
#1848=FACE_OUTER_BOUND('',#2487,.T.);
#1849=FACE_OUTER_BOUND('',#2488,.T.);
#1850=FACE_OUTER_BOUND('',#2489,.T.);
#1851=FACE_OUTER_BOUND('',#2490,.T.);
#1852=FACE_OUTER_BOUND('',#2491,.T.);
#1853=FACE_OUTER_BOUND('',#2492,.T.);
#1854=FACE_OUTER_BOUND('',#2493,.T.);
#1855=FACE_OUTER_BOUND('',#2494,.T.);
#1856=FACE_OUTER_BOUND('',#2495,.T.);
#1857=FACE_OUTER_BOUND('',#2496,.T.);
#1858=FACE_OUTER_BOUND('',#2497,.T.);
#1859=FACE_OUTER_BOUND('',#2498,.T.);
#1860=FACE_OUTER_BOUND('',#2499,.T.);
#1861=FACE_OUTER_BOUND('',#2500,.T.);
#1862=FACE_OUTER_BOUND('',#2501,.T.);
#1863=FACE_OUTER_BOUND('',#2502,.T.);
#1864=FACE_OUTER_BOUND('',#2503,.T.);
#1865=FACE_OUTER_BOUND('',#2504,.T.);
#1866=FACE_OUTER_BOUND('',#2505,.T.);
#1867=FACE_OUTER_BOUND('',#2506,.T.);
#1868=FACE_OUTER_BOUND('',#2507,.T.);
#1869=FACE_OUTER_BOUND('',#2508,.T.);
#1870=FACE_OUTER_BOUND('',#2509,.T.);
#1871=FACE_OUTER_BOUND('',#2510,.T.);
#1872=FACE_OUTER_BOUND('',#2511,.T.);
#1873=FACE_OUTER_BOUND('',#2512,.T.);
#1874=FACE_OUTER_BOUND('',#2513,.T.);
#1875=FACE_OUTER_BOUND('',#2514,.T.);
#1876=FACE_OUTER_BOUND('',#2515,.T.);
#1877=FACE_OUTER_BOUND('',#2516,.T.);
#1878=FACE_OUTER_BOUND('',#2517,.T.);
#1879=FACE_OUTER_BOUND('',#2518,.T.);
#1880=FACE_OUTER_BOUND('',#2519,.T.);
#1881=FACE_OUTER_BOUND('',#2520,.T.);
#1882=FACE_OUTER_BOUND('',#2521,.T.);
#1883=FACE_OUTER_BOUND('',#2522,.T.);
#1884=FACE_OUTER_BOUND('',#2523,.T.);
#1885=FACE_OUTER_BOUND('',#2524,.T.);
#1886=FACE_OUTER_BOUND('',#2525,.T.);
#1887=FACE_OUTER_BOUND('',#2526,.T.);
#1888=FACE_OUTER_BOUND('',#2527,.T.);
#1889=FACE_OUTER_BOUND('',#2528,.T.);
#1890=FACE_OUTER_BOUND('',#2529,.T.);
#1891=FACE_OUTER_BOUND('',#2530,.T.);
#1892=FACE_OUTER_BOUND('',#2531,.T.);
#1893=FACE_OUTER_BOUND('',#2532,.T.);
#1894=FACE_OUTER_BOUND('',#2533,.T.);
#1895=FACE_OUTER_BOUND('',#2534,.T.);
#1896=FACE_OUTER_BOUND('',#2535,.T.);
#1897=FACE_OUTER_BOUND('',#2536,.T.);
#1898=FACE_OUTER_BOUND('',#2537,.T.);
#1899=FACE_OUTER_BOUND('',#2538,.T.);
#1900=FACE_OUTER_BOUND('',#2539,.T.);
#1901=FACE_OUTER_BOUND('',#2540,.T.);
#1902=FACE_OUTER_BOUND('',#2541,.T.);
#1903=FACE_OUTER_BOUND('',#2542,.T.);
#1904=FACE_OUTER_BOUND('',#2543,.T.);
#1905=FACE_OUTER_BOUND('',#2544,.T.);
#1906=FACE_OUTER_BOUND('',#2545,.T.);
#1907=FACE_OUTER_BOUND('',#2546,.T.);
#1908=FACE_OUTER_BOUND('',#2547,.T.);
#1909=FACE_OUTER_BOUND('',#2548,.T.);
#1910=FACE_OUTER_BOUND('',#2549,.T.);
#1911=FACE_OUTER_BOUND('',#2550,.T.);
#1912=FACE_OUTER_BOUND('',#2551,.T.);
#1913=FACE_OUTER_BOUND('',#2552,.T.);
#1914=FACE_OUTER_BOUND('',#2553,.T.);
#1915=FACE_OUTER_BOUND('',#2554,.T.);
#1916=FACE_OUTER_BOUND('',#2555,.T.);
#1917=FACE_OUTER_BOUND('',#2556,.T.);
#1918=FACE_OUTER_BOUND('',#2557,.T.);
#1919=FACE_OUTER_BOUND('',#2558,.T.);
#1920=FACE_OUTER_BOUND('',#2559,.T.);
#1921=FACE_OUTER_BOUND('',#2560,.T.);
#1922=FACE_OUTER_BOUND('',#2561,.T.);
#1923=FACE_OUTER_BOUND('',#2562,.T.);
#1924=FACE_OUTER_BOUND('',#2563,.T.);
#1925=FACE_OUTER_BOUND('',#2564,.T.);
#1926=FACE_OUTER_BOUND('',#2565,.T.);
#1927=FACE_OUTER_BOUND('',#2566,.T.);
#1928=FACE_OUTER_BOUND('',#2567,.T.);
#1929=FACE_OUTER_BOUND('',#2568,.T.);
#1930=FACE_OUTER_BOUND('',#2569,.T.);
#1931=FACE_OUTER_BOUND('',#2570,.T.);
#1932=FACE_OUTER_BOUND('',#2571,.T.);
#1933=FACE_OUTER_BOUND('',#2572,.T.);
#1934=FACE_OUTER_BOUND('',#2573,.T.);
#1935=FACE_OUTER_BOUND('',#2574,.T.);
#1936=FACE_OUTER_BOUND('',#2575,.T.);
#1937=FACE_OUTER_BOUND('',#2576,.T.);
#1938=FACE_OUTER_BOUND('',#2577,.T.);
#1939=FACE_OUTER_BOUND('',#2578,.T.);
#1940=FACE_OUTER_BOUND('',#2579,.T.);
#1941=FACE_OUTER_BOUND('',#2580,.T.);
#1942=FACE_OUTER_BOUND('',#2581,.T.);
#1943=FACE_OUTER_BOUND('',#2582,.T.);
#1944=FACE_OUTER_BOUND('',#2583,.T.);
#1945=FACE_OUTER_BOUND('',#2584,.T.);
#1946=FACE_OUTER_BOUND('',#2585,.T.);
#1947=FACE_OUTER_BOUND('',#2586,.T.);
#1948=FACE_OUTER_BOUND('',#2587,.T.);
#1949=FACE_OUTER_BOUND('',#2588,.T.);
#1950=FACE_OUTER_BOUND('',#2589,.T.);
#1951=FACE_OUTER_BOUND('',#2590,.T.);
#1952=FACE_OUTER_BOUND('',#2591,.T.);
#1953=FACE_OUTER_BOUND('',#2592,.T.);
#1954=FACE_OUTER_BOUND('',#2593,.T.);
#1955=FACE_OUTER_BOUND('',#2594,.T.);
#1956=FACE_OUTER_BOUND('',#2595,.T.);
#1957=FACE_OUTER_BOUND('',#2596,.T.);
#1958=FACE_OUTER_BOUND('',#2597,.T.);
#1959=FACE_OUTER_BOUND('',#2598,.T.);
#1960=FACE_OUTER_BOUND('',#2599,.T.);
#1961=FACE_OUTER_BOUND('',#2600,.T.);
#1962=FACE_OUTER_BOUND('',#2601,.T.);
#1963=FACE_OUTER_BOUND('',#2602,.T.);
#1964=FACE_OUTER_BOUND('',#2603,.T.);
#1965=FACE_OUTER_BOUND('',#2604,.T.);
#1966=FACE_OUTER_BOUND('',#2605,.T.);
#1967=FACE_OUTER_BOUND('',#2606,.T.);
#1968=FACE_OUTER_BOUND('',#2607,.T.);
#1969=FACE_OUTER_BOUND('',#2608,.T.);
#1970=FACE_OUTER_BOUND('',#2609,.T.);
#1971=FACE_OUTER_BOUND('',#2610,.T.);
#1972=FACE_OUTER_BOUND('',#2611,.T.);
#1973=FACE_OUTER_BOUND('',#2612,.T.);
#1974=FACE_OUTER_BOUND('',#2613,.T.);
#1975=FACE_OUTER_BOUND('',#2614,.T.);
#1976=FACE_OUTER_BOUND('',#2615,.T.);
#1977=FACE_OUTER_BOUND('',#2616,.T.);
#1978=FACE_OUTER_BOUND('',#2617,.T.);
#1979=FACE_OUTER_BOUND('',#2618,.T.);
#1980=FACE_OUTER_BOUND('',#2619,.T.);
#1981=FACE_OUTER_BOUND('',#2620,.T.);
#1982=FACE_OUTER_BOUND('',#2621,.T.);
#1983=FACE_OUTER_BOUND('',#2622,.T.);
#1984=FACE_OUTER_BOUND('',#2623,.T.);
#1985=FACE_OUTER_BOUND('',#2624,.T.);
#1986=FACE_OUTER_BOUND('',#2625,.T.);
#1987=FACE_OUTER_BOUND('',#2626,.T.);
#1988=FACE_OUTER_BOUND('',#2627,.T.);
#1989=FACE_OUTER_BOUND('',#2628,.T.);
#1990=FACE_OUTER_BOUND('',#2629,.T.);
#1991=FACE_OUTER_BOUND('',#2630,.T.);
#1992=FACE_OUTER_BOUND('',#2631,.T.);
#1993=FACE_OUTER_BOUND('',#2632,.T.);
#1994=FACE_OUTER_BOUND('',#2633,.T.);
#1995=FACE_OUTER_BOUND('',#2634,.T.);
#1996=FACE_OUTER_BOUND('',#2635,.T.);
#1997=FACE_OUTER_BOUND('',#2636,.T.);
#1998=FACE_OUTER_BOUND('',#2637,.T.);
#1999=FACE_OUTER_BOUND('',#2638,.T.);
#2000=FACE_OUTER_BOUND('',#2639,.T.);
#2001=FACE_OUTER_BOUND('',#2640,.T.);
#2002=FACE_OUTER_BOUND('',#2641,.T.);
#2003=FACE_OUTER_BOUND('',#2642,.T.);
#2004=FACE_OUTER_BOUND('',#2643,.T.);
#2005=FACE_OUTER_BOUND('',#2644,.T.);
#2006=FACE_OUTER_BOUND('',#2645,.T.);
#2007=FACE_OUTER_BOUND('',#2646,.T.);
#2008=FACE_OUTER_BOUND('',#2647,.T.);
#2009=FACE_OUTER_BOUND('',#2648,.T.);
#2010=FACE_OUTER_BOUND('',#2649,.T.);
#2011=FACE_OUTER_BOUND('',#2650,.T.);
#2012=FACE_OUTER_BOUND('',#2651,.T.);
#2013=FACE_OUTER_BOUND('',#2652,.T.);
#2014=FACE_OUTER_BOUND('',#2653,.T.);
#2015=FACE_OUTER_BOUND('',#2654,.T.);
#2016=FACE_OUTER_BOUND('',#2655,.T.);
#2017=FACE_OUTER_BOUND('',#2656,.T.);
#2018=FACE_OUTER_BOUND('',#2657,.T.);
#2019=FACE_OUTER_BOUND('',#2658,.T.);
#2020=FACE_OUTER_BOUND('',#2659,.T.);
#2021=FACE_OUTER_BOUND('',#2660,.T.);
#2022=FACE_OUTER_BOUND('',#2661,.T.);
#2023=FACE_OUTER_BOUND('',#2662,.T.);
#2024=FACE_OUTER_BOUND('',#2663,.T.);
#2025=FACE_OUTER_BOUND('',#2664,.T.);
#2026=FACE_OUTER_BOUND('',#2665,.T.);
#2027=FACE_OUTER_BOUND('',#2666,.T.);
#2028=FACE_OUTER_BOUND('',#2667,.T.);
#2029=FACE_OUTER_BOUND('',#2668,.T.);
#2030=FACE_OUTER_BOUND('',#2669,.T.);
#2031=FACE_OUTER_BOUND('',#2670,.T.);
#2032=FACE_OUTER_BOUND('',#2671,.T.);
#2033=FACE_OUTER_BOUND('',#2672,.T.);
#2034=FACE_OUTER_BOUND('',#2673,.T.);
#2035=FACE_OUTER_BOUND('',#2674,.T.);
#2036=FACE_OUTER_BOUND('',#2675,.T.);
#2037=FACE_OUTER_BOUND('',#2676,.T.);
#2038=FACE_OUTER_BOUND('',#2677,.T.);
#2039=FACE_OUTER_BOUND('',#2678,.T.);
#2040=FACE_OUTER_BOUND('',#2679,.T.);
#2041=FACE_OUTER_BOUND('',#2680,.T.);
#2042=FACE_OUTER_BOUND('',#2681,.T.);
#2043=FACE_OUTER_BOUND('',#2682,.T.);
#2044=FACE_OUTER_BOUND('',#2683,.T.);
#2045=FACE_OUTER_BOUND('',#2684,.T.);
#2046=FACE_OUTER_BOUND('',#2685,.T.);
#2047=FACE_OUTER_BOUND('',#2686,.T.);
#2048=FACE_OUTER_BOUND('',#2687,.T.);
#2049=FACE_OUTER_BOUND('',#2688,.T.);
#2050=FACE_OUTER_BOUND('',#2689,.T.);
#2051=FACE_OUTER_BOUND('',#2690,.T.);
#2052=FACE_OUTER_BOUND('',#2691,.T.);
#2053=FACE_OUTER_BOUND('',#2692,.T.);
#2054=FACE_OUTER_BOUND('',#2693,.T.);
#2055=FACE_OUTER_BOUND('',#2694,.T.);
#2056=FACE_OUTER_BOUND('',#2695,.T.);
#2057=FACE_OUTER_BOUND('',#2696,.T.);
#2058=FACE_OUTER_BOUND('',#2697,.T.);
#2059=FACE_OUTER_BOUND('',#2698,.T.);
#2060=FACE_OUTER_BOUND('',#2699,.T.);
#2061=FACE_OUTER_BOUND('',#2700,.T.);
#2062=FACE_OUTER_BOUND('',#2701,.T.);
#2063=FACE_OUTER_BOUND('',#2702,.T.);
#2064=FACE_OUTER_BOUND('',#2703,.T.);
#2065=FACE_OUTER_BOUND('',#2704,.T.);
#2066=FACE_OUTER_BOUND('',#2705,.T.);
#2067=FACE_OUTER_BOUND('',#2706,.T.);
#2068=FACE_OUTER_BOUND('',#2707,.T.);
#2069=FACE_OUTER_BOUND('',#2708,.T.);
#2070=FACE_OUTER_BOUND('',#2709,.T.);
#2071=FACE_OUTER_BOUND('',#2712,.T.);
#2072=FACE_OUTER_BOUND('',#2713,.T.);
#2073=FACE_OUTER_BOUND('',#2716,.T.);
#2074=FACE_OUTER_BOUND('',#2717,.T.);
#2075=FACE_OUTER_BOUND('',#2719,.T.);
#2076=FACE_OUTER_BOUND('',#2722,.T.);
#2077=FACE_OUTER_BOUND('',#2724,.T.);
#2078=FACE_OUTER_BOUND('',#2727,.T.);
#2079=FACE_OUTER_BOUND('',#2728,.T.);
#2080=FACE_OUTER_BOUND('',#2737,.T.);
#2081=FACE_OUTER_BOUND('',#2746,.T.);
#2082=FACE_OUTER_BOUND('',#2747,.T.);
#2083=FACE_OUTER_BOUND('',#2748,.T.);
#2084=FACE_OUTER_BOUND('',#2749,.T.);
#2085=FACE_OUTER_BOUND('',#2750,.T.);
#2086=FACE_OUTER_BOUND('',#2751,.T.);
#2087=FACE_OUTER_BOUND('',#2752,.T.);
#2088=FACE_OUTER_BOUND('',#2753,.T.);
#2089=FACE_OUTER_BOUND('',#2754,.T.);
#2090=FACE_OUTER_BOUND('',#2755,.T.);
#2091=FACE_OUTER_BOUND('',#2756,.T.);
#2092=FACE_OUTER_BOUND('',#2757,.T.);
#2093=FACE_OUTER_BOUND('',#2758,.T.);
#2094=FACE_OUTER_BOUND('',#2759,.T.);
#2095=FACE_OUTER_BOUND('',#2760,.T.);
#2096=FACE_OUTER_BOUND('',#2761,.T.);
#2097=FACE_OUTER_BOUND('',#2762,.T.);
#2098=FACE_OUTER_BOUND('',#2763,.T.);
#2099=FACE_OUTER_BOUND('',#2764,.T.);
#2100=FACE_OUTER_BOUND('',#2765,.T.);
#2101=FACE_OUTER_BOUND('',#2766,.T.);
#2102=FACE_OUTER_BOUND('',#2767,.T.);
#2103=FACE_OUTER_BOUND('',#2768,.T.);
#2104=FACE_OUTER_BOUND('',#2769,.T.);
#2105=FACE_OUTER_BOUND('',#2770,.T.);
#2106=FACE_OUTER_BOUND('',#2771,.T.);
#2107=FACE_OUTER_BOUND('',#2772,.T.);
#2108=FACE_OUTER_BOUND('',#2773,.T.);
#2109=FACE_OUTER_BOUND('',#2774,.T.);
#2110=FACE_OUTER_BOUND('',#2775,.T.);
#2111=FACE_OUTER_BOUND('',#2776,.T.);
#2112=FACE_OUTER_BOUND('',#2777,.T.);
#2113=FACE_OUTER_BOUND('',#2778,.T.);
#2114=FACE_OUTER_BOUND('',#2779,.T.);
#2115=FACE_OUTER_BOUND('',#2780,.T.);
#2116=FACE_OUTER_BOUND('',#2781,.T.);
#2117=FACE_OUTER_BOUND('',#2782,.T.);
#2118=FACE_OUTER_BOUND('',#2783,.T.);
#2119=FACE_OUTER_BOUND('',#2784,.T.);
#2120=FACE_OUTER_BOUND('',#2785,.T.);
#2121=FACE_OUTER_BOUND('',#2786,.T.);
#2122=FACE_OUTER_BOUND('',#2787,.T.);
#2123=FACE_OUTER_BOUND('',#2788,.T.);
#2124=FACE_OUTER_BOUND('',#2789,.T.);
#2125=FACE_OUTER_BOUND('',#2790,.T.);
#2126=FACE_OUTER_BOUND('',#2798,.T.);
#2127=FACE_OUTER_BOUND('',#2806,.T.);
#2128=FACE_OUTER_BOUND('',#2807,.T.);
#2129=FACE_OUTER_BOUND('',#2808,.T.);
#2130=FACE_OUTER_BOUND('',#2809,.T.);
#2131=FACE_OUTER_BOUND('',#2810,.T.);
#2132=FACE_OUTER_BOUND('',#2811,.T.);
#2133=FACE_OUTER_BOUND('',#2812,.T.);
#2134=FACE_OUTER_BOUND('',#2813,.T.);
#2135=FACE_OUTER_BOUND('',#2814,.T.);
#2136=FACE_OUTER_BOUND('',#2822,.T.);
#2137=FACE_OUTER_BOUND('',#2830,.T.);
#2138=FACE_OUTER_BOUND('',#2831,.T.);
#2139=FACE_OUTER_BOUND('',#2832,.T.);
#2140=FACE_OUTER_BOUND('',#2833,.T.);
#2141=FACE_OUTER_BOUND('',#2834,.T.);
#2142=FACE_OUTER_BOUND('',#2835,.T.);
#2143=FACE_OUTER_BOUND('',#2836,.T.);
#2144=FACE_OUTER_BOUND('',#2838,.T.);
#2145=FACE_OUTER_BOUND('',#2839,.T.);
#2146=FACE_OUTER_BOUND('',#2840,.T.);
#2147=FACE_OUTER_BOUND('',#2841,.T.);
#2148=FACE_OUTER_BOUND('',#2842,.T.);
#2149=FACE_OUTER_BOUND('',#2843,.T.);
#2150=FACE_OUTER_BOUND('',#2844,.T.);
#2151=FACE_OUTER_BOUND('',#2845,.T.);
#2152=FACE_OUTER_BOUND('',#2847,.T.);
#2153=FACE_OUTER_BOUND('',#2848,.T.);
#2154=FACE_OUTER_BOUND('',#2849,.T.);
#2155=FACE_OUTER_BOUND('',#2850,.T.);
#2156=FACE_OUTER_BOUND('',#2851,.T.);
#2157=FACE_OUTER_BOUND('',#2852,.T.);
#2158=FACE_OUTER_BOUND('',#2853,.T.);
#2159=FACE_OUTER_BOUND('',#2854,.T.);
#2160=FACE_OUTER_BOUND('',#2855,.T.);
#2161=FACE_OUTER_BOUND('',#2856,.T.);
#2162=FACE_OUTER_BOUND('',#2857,.T.);
#2163=FACE_OUTER_BOUND('',#2858,.T.);
#2164=FACE_OUTER_BOUND('',#2859,.T.);
#2165=FACE_OUTER_BOUND('',#2860,.T.);
#2166=FACE_OUTER_BOUND('',#2861,.T.);
#2167=FACE_OUTER_BOUND('',#2862,.T.);
#2168=FACE_OUTER_BOUND('',#2863,.T.);
#2169=FACE_OUTER_BOUND('',#2864,.T.);
#2170=FACE_OUTER_BOUND('',#2865,.T.);
#2171=FACE_OUTER_BOUND('',#2866,.T.);
#2172=FACE_OUTER_BOUND('',#2867,.T.);
#2173=FACE_OUTER_BOUND('',#2869,.T.);
#2174=EDGE_LOOP('',(#6725,#6726,#6727,#6728));
#2175=EDGE_LOOP('',(#6729,#6730,#6731,#6732));
#2176=EDGE_LOOP('',(#6733,#6734,#6735,#6736));
#2177=EDGE_LOOP('',(#6737,#6738,#6739,#6740));
#2178=EDGE_LOOP('',(#6741,#6742,#6743,#6744));
#2179=EDGE_LOOP('',(#6745,#6746,#6747,#6748));
#2180=EDGE_LOOP('',(#6749,#6750,#6751,#6752));
#2181=EDGE_LOOP('',(#6753,#6754,#6755,#6756));
#2182=EDGE_LOOP('',(#6757,#6758,#6759,#6760));
#2183=EDGE_LOOP('',(#6761,#6762,#6763,#6764));
#2184=EDGE_LOOP('',(#6765,#6766,#6767,#6768));
#2185=EDGE_LOOP('',(#6769,#6770,#6771,#6772,#6773,#6774,#6775,#6776));
#2186=EDGE_LOOP('',(#6777,#6778,#6779,#6780));
#2187=EDGE_LOOP('',(#6781,#6782,#6783,#6784));
#2188=EDGE_LOOP('',(#6785,#6786,#6787,#6788));
#2189=EDGE_LOOP('',(#6789,#6790,#6791,#6792));
#2190=EDGE_LOOP('',(#6793,#6794,#6795,#6796,#6797,#6798,#6799,#6800,#6801,
#6802));
#2191=EDGE_LOOP('',(#6803));
#2192=EDGE_LOOP('',(#6804));
#2193=EDGE_LOOP('',(#6805,#6806,#6807,#6808,#6809,#6810,#6811,#6812));
#2194=EDGE_LOOP('',(#6813,#6814,#6815,#6816,#6817,#6818,#6819,#6820,#6821,
#6822));
#2195=EDGE_LOOP('',(#6823));
#2196=EDGE_LOOP('',(#6824));
#2197=EDGE_LOOP('',(#6825,#6826,#6827,#6828));
#2198=EDGE_LOOP('',(#6829,#6830,#6831,#6832));
#2199=EDGE_LOOP('',(#6833,#6834,#6835,#6836,#6837,#6838,#6839,#6840,#6841,
#6842));
#2200=EDGE_LOOP('',(#6843));
#2201=EDGE_LOOP('',(#6844));
#2202=EDGE_LOOP('',(#6845,#6846,#6847,#6848));
#2203=EDGE_LOOP('',(#6849,#6850,#6851,#6852,#6853,#6854,#6855,#6856,#6857,
#6858));
#2204=EDGE_LOOP('',(#6859));
#2205=EDGE_LOOP('',(#6860));
#2206=EDGE_LOOP('',(#6861,#6862,#6863,#6864));
#2207=EDGE_LOOP('',(#6865,#6866,#6867,#6868));
#2208=EDGE_LOOP('',(#6869));
#2209=EDGE_LOOP('',(#6870));
#2210=EDGE_LOOP('',(#6871));
#2211=EDGE_LOOP('',(#6872));
#2212=EDGE_LOOP('',(#6873));
#2213=EDGE_LOOP('',(#6874));
#2214=EDGE_LOOP('',(#6875));
#2215=EDGE_LOOP('',(#6876,#6877,#6878,#6879));
#2216=EDGE_LOOP('',(#6880));
#2217=EDGE_LOOP('',(#6881));
#2218=EDGE_LOOP('',(#6882));
#2219=EDGE_LOOP('',(#6883));
#2220=EDGE_LOOP('',(#6884));
#2221=EDGE_LOOP('',(#6885));
#2222=EDGE_LOOP('',(#6886));
#2223=EDGE_LOOP('',(#6887,#6888,#6889,#6890));
#2224=EDGE_LOOP('',(#6891,#6892,#6893,#6894));
#2225=EDGE_LOOP('',(#6895,#6896,#6897,#6898));
#2226=EDGE_LOOP('',(#6899,#6900,#6901,#6902));
#2227=EDGE_LOOP('',(#6903,#6904,#6905,#6906));
#2228=EDGE_LOOP('',(#6907,#6908,#6909,#6910));
#2229=EDGE_LOOP('',(#6911,#6912,#6913,#6914));
#2230=EDGE_LOOP('',(#6915,#6916,#6917,#6918));
#2231=EDGE_LOOP('',(#6919,#6920,#6921,#6922));
#2232=EDGE_LOOP('',(#6923,#6924,#6925,#6926));
#2233=EDGE_LOOP('',(#6927,#6928,#6929,#6930,#6931,#6932,#6933,#6934));
#2234=EDGE_LOOP('',(#6935,#6936,#6937,#6938));
#2235=EDGE_LOOP('',(#6939,#6940,#6941,#6942));
#2236=EDGE_LOOP('',(#6943,#6944,#6945,#6946,#6947));
#2237=EDGE_LOOP('',(#6948,#6949,#6950,#6951,#6952));
#2238=EDGE_LOOP('',(#6953,#6954,#6955,#6956));
#2239=EDGE_LOOP('',(#6957,#6958,#6959,#6960,#6961,#6962,#6963,#6964));
#2240=EDGE_LOOP('',(#6965,#6966,#6967,#6968,#6969));
#2241=EDGE_LOOP('',(#6970,#6971,#6972,#6973,#6974,#6975,#6976,#6977));
#2242=EDGE_LOOP('',(#6978,#6979,#6980,#6981));
#2243=EDGE_LOOP('',(#6982,#6983,#6984,#6985,#6986));
#2244=EDGE_LOOP('',(#6987,#6988,#6989,#6990));
#2245=EDGE_LOOP('',(#6991));
#2246=EDGE_LOOP('',(#6992));
#2247=EDGE_LOOP('',(#6993));
#2248=EDGE_LOOP('',(#6994));
#2249=EDGE_LOOP('',(#6995));
#2250=EDGE_LOOP('',(#6996));
#2251=EDGE_LOOP('',(#6997,#6998,#6999,#7000));
#2252=EDGE_LOOP('',(#7001,#7002,#7003,#7004,#7005,#7006,#7007,#7008));
#2253=EDGE_LOOP('',(#7009,#7010,#7011,#7012));
#2254=EDGE_LOOP('',(#7013,#7014,#7015,#7016,#7017,#7018,#7019,#7020));
#2255=EDGE_LOOP('',(#7021,#7022,#7023,#7024));
#2256=EDGE_LOOP('',(#7025,#7026,#7027,#7028,#7029,#7030,#7031,#7032));
#2257=EDGE_LOOP('',(#7033,#7034,#7035,#7036));
#2258=EDGE_LOOP('',(#7037,#7038,#7039,#7040,#7041,#7042,#7043,#7044));
#2259=EDGE_LOOP('',(#7045,#7046,#7047,#7048,#7049));
#2260=EDGE_LOOP('',(#7050,#7051,#7052,#7053));
#2261=EDGE_LOOP('',(#7054,#7055,#7056,#7057));
#2262=EDGE_LOOP('',(#7058,#7059,#7060,#7061));
#2263=EDGE_LOOP('',(#7062,#7063,#7064,#7065));
#2264=EDGE_LOOP('',(#7066));
#2265=EDGE_LOOP('',(#7067,#7068,#7069,#7070,#7071));
#2266=EDGE_LOOP('',(#7072,#7073,#7074,#7075));
#2267=EDGE_LOOP('',(#7076,#7077,#7078,#7079));
#2268=EDGE_LOOP('',(#7080,#7081,#7082,#7083,#7084));
#2269=EDGE_LOOP('',(#7085,#7086,#7087,#7088,#7089,#7090,#7091,#7092));
#2270=EDGE_LOOP('',(#7093,#7094,#7095,#7096,#7097));
#2271=EDGE_LOOP('',(#7098));
#2272=EDGE_LOOP('',(#7099,#7100,#7101,#7102));
#2273=EDGE_LOOP('',(#7103,#7104,#7105,#7106));
#2274=EDGE_LOOP('',(#7107,#7108,#7109,#7110));
#2275=EDGE_LOOP('',(#7111,#7112,#7113,#7114));
#2276=EDGE_LOOP('',(#7115));
#2277=EDGE_LOOP('',(#7116,#7117,#7118,#7119));
#2278=EDGE_LOOP('',(#7120));
#2279=EDGE_LOOP('',(#7121));
#2280=EDGE_LOOP('',(#7122));
#2281=EDGE_LOOP('',(#7123,#7124,#7125,#7126));
#2282=EDGE_LOOP('',(#7127,#7128,#7129,#7130));
#2283=EDGE_LOOP('',(#7131,#7132,#7133,#7134));
#2284=EDGE_LOOP('',(#7135,#7136,#7137,#7138));
#2285=EDGE_LOOP('',(#7139,#7140,#7141,#7142,#7143,#7144));
#2286=EDGE_LOOP('',(#7145,#7146,#7147,#7148,#7149,#7150));
#2287=EDGE_LOOP('',(#7151,#7152,#7153,#7154,#7155,#7156));
#2288=EDGE_LOOP('',(#7157,#7158,#7159,#7160,#7161,#7162));
#2289=EDGE_LOOP('',(#7163,#7164,#7165,#7166,#7167,#7168));
#2290=EDGE_LOOP('',(#7169,#7170,#7171,#7172,#7173,#7174));
#2291=EDGE_LOOP('',(#7175,#7176,#7177,#7178,#7179,#7180));
#2292=EDGE_LOOP('',(#7181,#7182,#7183,#7184,#7185,#7186));
#2293=EDGE_LOOP('',(#7187,#7188,#7189,#7190,#7191,#7192));
#2294=EDGE_LOOP('',(#7193,#7194,#7195,#7196,#7197,#7198));
#2295=EDGE_LOOP('',(#7199,#7200,#7201,#7202,#7203,#7204));
#2296=EDGE_LOOP('',(#7205,#7206,#7207,#7208,#7209,#7210));
#2297=EDGE_LOOP('',(#7211,#7212,#7213,#7214,#7215,#7216));
#2298=EDGE_LOOP('',(#7217,#7218,#7219,#7220,#7221,#7222));
#2299=EDGE_LOOP('',(#7223,#7224,#7225,#7226,#7227,#7228));
#2300=EDGE_LOOP('',(#7229,#7230,#7231,#7232,#7233,#7234));
#2301=EDGE_LOOP('',(#7235,#7236,#7237,#7238,#7239,#7240));
#2302=EDGE_LOOP('',(#7241,#7242,#7243,#7244,#7245,#7246));
#2303=EDGE_LOOP('',(#7247,#7248,#7249,#7250,#7251,#7252));
#2304=EDGE_LOOP('',(#7253,#7254,#7255,#7256,#7257,#7258));
#2305=EDGE_LOOP('',(#7259,#7260,#7261,#7262,#7263,#7264));
#2306=EDGE_LOOP('',(#7265,#7266,#7267,#7268,#7269,#7270));
#2307=EDGE_LOOP('',(#7271,#7272,#7273,#7274,#7275,#7276));
#2308=EDGE_LOOP('',(#7277,#7278,#7279,#7280,#7281,#7282));
#2309=EDGE_LOOP('',(#7283,#7284,#7285,#7286,#7287,#7288));
#2310=EDGE_LOOP('',(#7289,#7290,#7291,#7292,#7293,#7294));
#2311=EDGE_LOOP('',(#7295,#7296,#7297,#7298,#7299,#7300));
#2312=EDGE_LOOP('',(#7301,#7302,#7303,#7304,#7305,#7306));
#2313=EDGE_LOOP('',(#7307,#7308,#7309,#7310,#7311,#7312));
#2314=EDGE_LOOP('',(#7313,#7314,#7315,#7316,#7317,#7318));
#2315=EDGE_LOOP('',(#7319,#7320,#7321,#7322,#7323,#7324));
#2316=EDGE_LOOP('',(#7325,#7326,#7327,#7328,#7329,#7330));
#2317=EDGE_LOOP('',(#7331,#7332,#7333,#7334,#7335,#7336));
#2318=EDGE_LOOP('',(#7337,#7338,#7339,#7340,#7341,#7342));
#2319=EDGE_LOOP('',(#7343,#7344,#7345,#7346,#7347,#7348));
#2320=EDGE_LOOP('',(#7349,#7350,#7351,#7352,#7353,#7354));
#2321=EDGE_LOOP('',(#7355,#7356,#7357,#7358,#7359,#7360));
#2322=EDGE_LOOP('',(#7361,#7362,#7363,#7364,#7365,#7366));
#2323=EDGE_LOOP('',(#7367,#7368,#7369,#7370,#7371,#7372));
#2324=EDGE_LOOP('',(#7373,#7374,#7375,#7376,#7377,#7378));
#2325=EDGE_LOOP('',(#7379,#7380,#7381,#7382,#7383,#7384));
#2326=EDGE_LOOP('',(#7385,#7386,#7387,#7388,#7389,#7390));
#2327=EDGE_LOOP('',(#7391,#7392,#7393,#7394,#7395,#7396));
#2328=EDGE_LOOP('',(#7397,#7398,#7399,#7400,#7401,#7402));
#2329=EDGE_LOOP('',(#7403,#7404,#7405,#7406,#7407,#7408,#7409,#7410,#7411,
#7412,#7413,#7414,#7415,#7416,#7417,#7418,#7419,#7420,#7421,#7422,#7423,
#7424,#7425,#7426,#7427,#7428,#7429,#7430,#7431,#7432,#7433,#7434,#7435,
#7436,#7437,#7438,#7439,#7440,#7441,#7442,#7443,#7444,#7445,#7446,#7447,
#7448,#7449,#7450,#7451,#7452,#7453,#7454,#7455,#7456,#7457,#7458,#7459,
#7460,#7461,#7462,#7463,#7464,#7465,#7466,#7467,#7468,#7469,#7470,#7471,
#7472,#7473,#7474,#7475,#7476,#7477,#7478,#7479,#7480,#7481,#7482,#7483,
#7484,#7485,#7486,#7487,#7488,#7489,#7490,#7491,#7492,#7493,#7494,#7495,
#7496,#7497,#7498,#7499,#7500,#7501,#7502,#7503,#7504,#7505,#7506,#7507,
#7508,#7509,#7510,#7511,#7512,#7513,#7514,#7515,#7516,#7517,#7518,#7519,
#7520,#7521,#7522,#7523,#7524,#7525,#7526,#7527,#7528,#7529,#7530,#7531,
#7532,#7533,#7534,#7535,#7536,#7537,#7538,#7539,#7540,#7541,#7542,#7543,
#7544,#7545,#7546,#7547,#7548,#7549,#7550,#7551,#7552,#7553,#7554,#7555,
#7556,#7557,#7558,#7559,#7560,#7561,#7562,#7563,#7564,#7565,#7566,#7567,
#7568,#7569,#7570,#7571,#7572,#7573,#7574,#7575,#7576,#7577,#7578,#7579,
#7580,#7581,#7582));
#2330=EDGE_LOOP('',(#7583,#7584,#7585,#7586));
#2331=EDGE_LOOP('',(#7587,#7588,#7589,#7590,#7591,#7592,#7593,#7594,#7595,
#7596,#7597,#7598,#7599,#7600,#7601,#7602,#7603,#7604,#7605,#7606,#7607,
#7608,#7609,#7610,#7611,#7612,#7613,#7614,#7615,#7616,#7617,#7618,#7619,
#7620,#7621,#7622,#7623,#7624,#7625,#7626,#7627,#7628,#7629,#7630,#7631,
#7632,#7633,#7634,#7635,#7636,#7637,#7638,#7639,#7640,#7641,#7642,#7643,
#7644,#7645,#7646,#7647,#7648,#7649,#7650,#7651,#7652,#7653,#7654,#7655,
#7656,#7657,#7658,#7659,#7660,#7661,#7662,#7663,#7664,#7665,#7666,#7667,
#7668,#7669,#7670,#7671,#7672,#7673,#7674,#7675,#7676,#7677,#7678,#7679,
#7680,#7681,#7682,#7683,#7684,#7685,#7686,#7687,#7688,#7689,#7690,#7691,
#7692,#7693,#7694,#7695,#7696,#7697,#7698,#7699,#7700,#7701,#7702,#7703,
#7704,#7705,#7706,#7707,#7708,#7709,#7710,#7711,#7712,#7713,#7714,#7715,
#7716,#7717,#7718,#7719,#7720,#7721,#7722,#7723,#7724,#7725,#7726,#7727,
#7728,#7729,#7730,#7731,#7732,#7733,#7734,#7735,#7736,#7737,#7738,#7739,
#7740,#7741,#7742,#7743,#7744,#7745,#7746,#7747,#7748,#7749,#7750,#7751,
#7752,#7753,#7754,#7755,#7756,#7757,#7758,#7759,#7760,#7761,#7762,#7763,
#7764,#7765,#7766));
#2332=EDGE_LOOP('',(#7767,#7768,#7769,#7770));
#2333=EDGE_LOOP('',(#7771,#7772,#7773,#7774));
#2334=EDGE_LOOP('',(#7775,#7776,#7777,#7778));
#2335=EDGE_LOOP('',(#7779,#7780,#7781,#7782));
#2336=EDGE_LOOP('',(#7783,#7784,#7785,#7786));
#2337=EDGE_LOOP('',(#7787,#7788,#7789,#7790));
#2338=EDGE_LOOP('',(#7791,#7792,#7793,#7794));
#2339=EDGE_LOOP('',(#7795,#7796,#7797,#7798));
#2340=EDGE_LOOP('',(#7799,#7800,#7801,#7802));
#2341=EDGE_LOOP('',(#7803,#7804,#7805,#7806));
#2342=EDGE_LOOP('',(#7807,#7808,#7809,#7810));
#2343=EDGE_LOOP('',(#7811,#7812,#7813,#7814));
#2344=EDGE_LOOP('',(#7815,#7816,#7817,#7818));
#2345=EDGE_LOOP('',(#7819,#7820,#7821,#7822));
#2346=EDGE_LOOP('',(#7823,#7824,#7825,#7826));
#2347=EDGE_LOOP('',(#7827,#7828,#7829,#7830));
#2348=EDGE_LOOP('',(#7831,#7832,#7833,#7834));
#2349=EDGE_LOOP('',(#7835,#7836,#7837,#7838));
#2350=EDGE_LOOP('',(#7839,#7840,#7841,#7842));
#2351=EDGE_LOOP('',(#7843,#7844,#7845,#7846));
#2352=EDGE_LOOP('',(#7847,#7848,#7849,#7850));
#2353=EDGE_LOOP('',(#7851,#7852,#7853,#7854));
#2354=EDGE_LOOP('',(#7855,#7856,#7857,#7858));
#2355=EDGE_LOOP('',(#7859,#7860,#7861,#7862));
#2356=EDGE_LOOP('',(#7863,#7864,#7865,#7866));
#2357=EDGE_LOOP('',(#7867,#7868,#7869,#7870));
#2358=EDGE_LOOP('',(#7871,#7872,#7873,#7874));
#2359=EDGE_LOOP('',(#7875,#7876,#7877,#7878));
#2360=EDGE_LOOP('',(#7879,#7880,#7881,#7882));
#2361=EDGE_LOOP('',(#7883,#7884,#7885,#7886));
#2362=EDGE_LOOP('',(#7887,#7888,#7889,#7890));
#2363=EDGE_LOOP('',(#7891,#7892,#7893,#7894));
#2364=EDGE_LOOP('',(#7895,#7896,#7897,#7898));
#2365=EDGE_LOOP('',(#7899,#7900,#7901,#7902));
#2366=EDGE_LOOP('',(#7903,#7904,#7905,#7906));
#2367=EDGE_LOOP('',(#7907,#7908,#7909,#7910));
#2368=EDGE_LOOP('',(#7911,#7912,#7913,#7914));
#2369=EDGE_LOOP('',(#7915,#7916,#7917,#7918));
#2370=EDGE_LOOP('',(#7919,#7920,#7921,#7922));
#2371=EDGE_LOOP('',(#7923,#7924,#7925,#7926));
#2372=EDGE_LOOP('',(#7927,#7928,#7929,#7930));
#2373=EDGE_LOOP('',(#7931,#7932,#7933,#7934));
#2374=EDGE_LOOP('',(#7935,#7936,#7937,#7938));
#2375=EDGE_LOOP('',(#7939,#7940,#7941,#7942));
#2376=EDGE_LOOP('',(#7943,#7944,#7945,#7946));
#2377=EDGE_LOOP('',(#7947,#7948,#7949,#7950));
#2378=EDGE_LOOP('',(#7951,#7952,#7953,#7954));
#2379=EDGE_LOOP('',(#7955,#7956,#7957,#7958));
#2380=EDGE_LOOP('',(#7959,#7960,#7961,#7962));
#2381=EDGE_LOOP('',(#7963,#7964,#7965,#7966));
#2382=EDGE_LOOP('',(#7967,#7968,#7969,#7970));
#2383=EDGE_LOOP('',(#7971,#7972,#7973,#7974));
#2384=EDGE_LOOP('',(#7975,#7976,#7977,#7978));
#2385=EDGE_LOOP('',(#7979,#7980,#7981,#7982));
#2386=EDGE_LOOP('',(#7983,#7984,#7985,#7986));
#2387=EDGE_LOOP('',(#7987,#7988,#7989,#7990));
#2388=EDGE_LOOP('',(#7991,#7992,#7993,#7994));
#2389=EDGE_LOOP('',(#7995,#7996,#7997,#7998));
#2390=EDGE_LOOP('',(#7999,#8000,#8001,#8002));
#2391=EDGE_LOOP('',(#8003,#8004,#8005,#8006));
#2392=EDGE_LOOP('',(#8007,#8008,#8009,#8010));
#2393=EDGE_LOOP('',(#8011,#8012,#8013,#8014));
#2394=EDGE_LOOP('',(#8015,#8016,#8017,#8018));
#2395=EDGE_LOOP('',(#8019,#8020,#8021,#8022));
#2396=EDGE_LOOP('',(#8023,#8024,#8025,#8026));
#2397=EDGE_LOOP('',(#8027,#8028,#8029,#8030));
#2398=EDGE_LOOP('',(#8031,#8032,#8033,#8034));
#2399=EDGE_LOOP('',(#8035,#8036,#8037,#8038));
#2400=EDGE_LOOP('',(#8039,#8040,#8041,#8042));
#2401=EDGE_LOOP('',(#8043,#8044,#8045,#8046));
#2402=EDGE_LOOP('',(#8047,#8048,#8049,#8050));
#2403=EDGE_LOOP('',(#8051,#8052,#8053,#8054));
#2404=EDGE_LOOP('',(#8055,#8056,#8057,#8058));
#2405=EDGE_LOOP('',(#8059,#8060,#8061,#8062));
#2406=EDGE_LOOP('',(#8063,#8064,#8065,#8066));
#2407=EDGE_LOOP('',(#8067,#8068,#8069,#8070));
#2408=EDGE_LOOP('',(#8071,#8072,#8073,#8074));
#2409=EDGE_LOOP('',(#8075,#8076,#8077,#8078));
#2410=EDGE_LOOP('',(#8079,#8080,#8081,#8082));
#2411=EDGE_LOOP('',(#8083,#8084,#8085,#8086));
#2412=EDGE_LOOP('',(#8087,#8088,#8089,#8090));
#2413=EDGE_LOOP('',(#8091,#8092,#8093,#8094));
#2414=EDGE_LOOP('',(#8095,#8096,#8097,#8098));
#2415=EDGE_LOOP('',(#8099,#8100,#8101,#8102));
#2416=EDGE_LOOP('',(#8103,#8104,#8105,#8106));
#2417=EDGE_LOOP('',(#8107,#8108,#8109,#8110));
#2418=EDGE_LOOP('',(#8111,#8112,#8113,#8114));
#2419=EDGE_LOOP('',(#8115,#8116,#8117,#8118));
#2420=EDGE_LOOP('',(#8119));
#2421=EDGE_LOOP('',(#8120,#8121,#8122,#8123));
#2422=EDGE_LOOP('',(#8124));
#2423=EDGE_LOOP('',(#8125,#8126,#8127,#8128));
#2424=EDGE_LOOP('',(#8129,#8130,#8131,#8132));
#2425=EDGE_LOOP('',(#8133,#8134,#8135,#8136));
#2426=EDGE_LOOP('',(#8137,#8138,#8139,#8140));
#2427=EDGE_LOOP('',(#8141,#8142,#8143,#8144,#8145));
#2428=EDGE_LOOP('',(#8146,#8147,#8148,#8149,#8150));
#2429=EDGE_LOOP('',(#8151,#8152,#8153,#8154,#8155));
#2430=EDGE_LOOP('',(#8156,#8157,#8158,#8159,#8160));
#2431=EDGE_LOOP('',(#8161,#8162,#8163,#8164,#8165));
#2432=EDGE_LOOP('',(#8166,#8167,#8168,#8169,#8170));
#2433=EDGE_LOOP('',(#8171,#8172,#8173,#8174,#8175));
#2434=EDGE_LOOP('',(#8176,#8177,#8178,#8179,#8180));
#2435=EDGE_LOOP('',(#8181,#8182,#8183,#8184,#8185));
#2436=EDGE_LOOP('',(#8186,#8187,#8188,#8189,#8190));
#2437=EDGE_LOOP('',(#8191,#8192,#8193,#8194,#8195));
#2438=EDGE_LOOP('',(#8196,#8197,#8198,#8199,#8200));
#2439=EDGE_LOOP('',(#8201,#8202,#8203,#8204,#8205));
#2440=EDGE_LOOP('',(#8206,#8207,#8208,#8209,#8210));
#2441=EDGE_LOOP('',(#8211,#8212,#8213,#8214,#8215));
#2442=EDGE_LOOP('',(#8216,#8217,#8218,#8219,#8220));
#2443=EDGE_LOOP('',(#8221,#8222,#8223,#8224,#8225));
#2444=EDGE_LOOP('',(#8226,#8227,#8228,#8229,#8230));
#2445=EDGE_LOOP('',(#8231,#8232,#8233,#8234,#8235));
#2446=EDGE_LOOP('',(#8236,#8237,#8238,#8239,#8240));
#2447=EDGE_LOOP('',(#8241,#8242,#8243,#8244,#8245));
#2448=EDGE_LOOP('',(#8246,#8247,#8248,#8249,#8250));
#2449=EDGE_LOOP('',(#8251,#8252,#8253,#8254,#8255));
#2450=EDGE_LOOP('',(#8256,#8257,#8258,#8259,#8260));
#2451=EDGE_LOOP('',(#8261,#8262,#8263,#8264,#8265));
#2452=EDGE_LOOP('',(#8266,#8267,#8268,#8269,#8270));
#2453=EDGE_LOOP('',(#8271,#8272,#8273,#8274,#8275));
#2454=EDGE_LOOP('',(#8276,#8277,#8278,#8279,#8280));
#2455=EDGE_LOOP('',(#8281,#8282,#8283,#8284,#8285));
#2456=EDGE_LOOP('',(#8286,#8287,#8288,#8289,#8290));
#2457=EDGE_LOOP('',(#8291,#8292,#8293,#8294,#8295));
#2458=EDGE_LOOP('',(#8296,#8297,#8298,#8299,#8300));
#2459=EDGE_LOOP('',(#8301,#8302,#8303,#8304,#8305));
#2460=EDGE_LOOP('',(#8306,#8307,#8308,#8309,#8310));
#2461=EDGE_LOOP('',(#8311,#8312,#8313,#8314,#8315));
#2462=EDGE_LOOP('',(#8316,#8317,#8318,#8319,#8320));
#2463=EDGE_LOOP('',(#8321,#8322,#8323,#8324,#8325));
#2464=EDGE_LOOP('',(#8326,#8327,#8328,#8329,#8330));
#2465=EDGE_LOOP('',(#8331,#8332,#8333,#8334,#8335));
#2466=EDGE_LOOP('',(#8336,#8337,#8338,#8339,#8340));
#2467=EDGE_LOOP('',(#8341,#8342,#8343,#8344,#8345));
#2468=EDGE_LOOP('',(#8346,#8347,#8348,#8349,#8350));
#2469=EDGE_LOOP('',(#8351,#8352,#8353,#8354,#8355));
#2470=EDGE_LOOP('',(#8356,#8357,#8358,#8359,#8360));
#2471=EDGE_LOOP('',(#8361,#8362,#8363,#8364,#8365));
#2472=EDGE_LOOP('',(#8366,#8367,#8368,#8369,#8370));
#2473=EDGE_LOOP('',(#8371,#8372,#8373,#8374,#8375));
#2474=EDGE_LOOP('',(#8376,#8377,#8378,#8379,#8380));
#2475=EDGE_LOOP('',(#8381,#8382,#8383,#8384,#8385));
#2476=EDGE_LOOP('',(#8386,#8387,#8388,#8389,#8390));
#2477=EDGE_LOOP('',(#8391,#8392,#8393,#8394,#8395));
#2478=EDGE_LOOP('',(#8396,#8397,#8398,#8399,#8400));
#2479=EDGE_LOOP('',(#8401,#8402,#8403,#8404,#8405));
#2480=EDGE_LOOP('',(#8406,#8407,#8408,#8409,#8410));
#2481=EDGE_LOOP('',(#8411,#8412,#8413,#8414,#8415));
#2482=EDGE_LOOP('',(#8416,#8417,#8418,#8419,#8420));
#2483=EDGE_LOOP('',(#8421,#8422,#8423,#8424,#8425));
#2484=EDGE_LOOP('',(#8426,#8427,#8428,#8429,#8430));
#2485=EDGE_LOOP('',(#8431,#8432,#8433,#8434,#8435));
#2486=EDGE_LOOP('',(#8436,#8437,#8438,#8439,#8440));
#2487=EDGE_LOOP('',(#8441,#8442,#8443,#8444,#8445));
#2488=EDGE_LOOP('',(#8446,#8447,#8448,#8449,#8450));
#2489=EDGE_LOOP('',(#8451,#8452,#8453,#8454,#8455));
#2490=EDGE_LOOP('',(#8456,#8457,#8458,#8459,#8460));
#2491=EDGE_LOOP('',(#8461,#8462,#8463,#8464,#8465));
#2492=EDGE_LOOP('',(#8466,#8467,#8468,#8469,#8470));
#2493=EDGE_LOOP('',(#8471,#8472,#8473,#8474,#8475));
#2494=EDGE_LOOP('',(#8476,#8477,#8478,#8479,#8480));
#2495=EDGE_LOOP('',(#8481,#8482,#8483,#8484,#8485));
#2496=EDGE_LOOP('',(#8486,#8487,#8488,#8489,#8490));
#2497=EDGE_LOOP('',(#8491,#8492,#8493,#8494,#8495));
#2498=EDGE_LOOP('',(#8496,#8497,#8498,#8499,#8500));
#2499=EDGE_LOOP('',(#8501,#8502,#8503,#8504,#8505));
#2500=EDGE_LOOP('',(#8506,#8507,#8508,#8509,#8510));
#2501=EDGE_LOOP('',(#8511,#8512,#8513,#8514,#8515));
#2502=EDGE_LOOP('',(#8516,#8517,#8518,#8519,#8520));
#2503=EDGE_LOOP('',(#8521,#8522,#8523,#8524,#8525));
#2504=EDGE_LOOP('',(#8526,#8527,#8528,#8529,#8530));
#2505=EDGE_LOOP('',(#8531,#8532,#8533,#8534,#8535));
#2506=EDGE_LOOP('',(#8536,#8537,#8538,#8539,#8540));
#2507=EDGE_LOOP('',(#8541,#8542,#8543,#8544,#8545));
#2508=EDGE_LOOP('',(#8546,#8547,#8548,#8549,#8550));
#2509=EDGE_LOOP('',(#8551,#8552,#8553,#8554,#8555));
#2510=EDGE_LOOP('',(#8556,#8557,#8558,#8559,#8560));
#2511=EDGE_LOOP('',(#8561,#8562,#8563,#8564,#8565));
#2512=EDGE_LOOP('',(#8566,#8567,#8568,#8569,#8570));
#2513=EDGE_LOOP('',(#8571,#8572,#8573,#8574,#8575));
#2514=EDGE_LOOP('',(#8576,#8577,#8578,#8579,#8580));
#2515=EDGE_LOOP('',(#8581,#8582,#8583,#8584,#8585));
#2516=EDGE_LOOP('',(#8586,#8587,#8588,#8589,#8590));
#2517=EDGE_LOOP('',(#8591,#8592,#8593,#8594,#8595));
#2518=EDGE_LOOP('',(#8596,#8597,#8598,#8599,#8600));
#2519=EDGE_LOOP('',(#8601,#8602,#8603,#8604,#8605));
#2520=EDGE_LOOP('',(#8606,#8607,#8608,#8609,#8610));
#2521=EDGE_LOOP('',(#8611,#8612,#8613,#8614,#8615));
#2522=EDGE_LOOP('',(#8616,#8617,#8618,#8619,#8620));
#2523=EDGE_LOOP('',(#8621,#8622,#8623,#8624,#8625));
#2524=EDGE_LOOP('',(#8626,#8627,#8628,#8629,#8630));
#2525=EDGE_LOOP('',(#8631,#8632,#8633,#8634,#8635));
#2526=EDGE_LOOP('',(#8636,#8637,#8638,#8639,#8640));
#2527=EDGE_LOOP('',(#8641,#8642,#8643,#8644,#8645));
#2528=EDGE_LOOP('',(#8646,#8647,#8648,#8649,#8650));
#2529=EDGE_LOOP('',(#8651,#8652,#8653,#8654,#8655));
#2530=EDGE_LOOP('',(#8656,#8657,#8658,#8659,#8660));
#2531=EDGE_LOOP('',(#8661,#8662,#8663,#8664,#8665,#8666));
#2532=EDGE_LOOP('',(#8667,#8668,#8669,#8670,#8671));
#2533=EDGE_LOOP('',(#8672,#8673,#8674,#8675,#8676));
#2534=EDGE_LOOP('',(#8677,#8678,#8679,#8680,#8681));
#2535=EDGE_LOOP('',(#8682,#8683,#8684,#8685,#8686));
#2536=EDGE_LOOP('',(#8687,#8688,#8689,#8690,#8691));
#2537=EDGE_LOOP('',(#8692,#8693,#8694,#8695,#8696));
#2538=EDGE_LOOP('',(#8697,#8698,#8699,#8700,#8701));
#2539=EDGE_LOOP('',(#8702,#8703,#8704,#8705,#8706));
#2540=EDGE_LOOP('',(#8707,#8708,#8709,#8710,#8711));
#2541=EDGE_LOOP('',(#8712,#8713,#8714,#8715,#8716));
#2542=EDGE_LOOP('',(#8717,#8718,#8719,#8720,#8721));
#2543=EDGE_LOOP('',(#8722,#8723,#8724,#8725,#8726));
#2544=EDGE_LOOP('',(#8727,#8728,#8729,#8730,#8731));
#2545=EDGE_LOOP('',(#8732,#8733,#8734,#8735,#8736));
#2546=EDGE_LOOP('',(#8737,#8738,#8739,#8740,#8741));
#2547=EDGE_LOOP('',(#8742,#8743,#8744,#8745,#8746));
#2548=EDGE_LOOP('',(#8747,#8748,#8749,#8750,#8751));
#2549=EDGE_LOOP('',(#8752,#8753,#8754,#8755,#8756));
#2550=EDGE_LOOP('',(#8757,#8758,#8759,#8760,#8761));
#2551=EDGE_LOOP('',(#8762,#8763,#8764,#8765,#8766));
#2552=EDGE_LOOP('',(#8767,#8768,#8769,#8770,#8771));
#2553=EDGE_LOOP('',(#8772,#8773,#8774,#8775,#8776));
#2554=EDGE_LOOP('',(#8777,#8778,#8779,#8780,#8781));
#2555=EDGE_LOOP('',(#8782,#8783,#8784,#8785,#8786));
#2556=EDGE_LOOP('',(#8787,#8788,#8789,#8790,#8791));
#2557=EDGE_LOOP('',(#8792,#8793,#8794,#8795,#8796));
#2558=EDGE_LOOP('',(#8797,#8798,#8799,#8800,#8801));
#2559=EDGE_LOOP('',(#8802,#8803,#8804,#8805,#8806));
#2560=EDGE_LOOP('',(#8807,#8808,#8809,#8810,#8811));
#2561=EDGE_LOOP('',(#8812,#8813,#8814,#8815,#8816));
#2562=EDGE_LOOP('',(#8817,#8818,#8819,#8820,#8821));
#2563=EDGE_LOOP('',(#8822,#8823,#8824,#8825,#8826));
#2564=EDGE_LOOP('',(#8827,#8828,#8829,#8830,#8831));
#2565=EDGE_LOOP('',(#8832,#8833,#8834,#8835,#8836));
#2566=EDGE_LOOP('',(#8837,#8838,#8839,#8840,#8841));
#2567=EDGE_LOOP('',(#8842,#8843,#8844,#8845,#8846));
#2568=EDGE_LOOP('',(#8847,#8848,#8849,#8850,#8851));
#2569=EDGE_LOOP('',(#8852,#8853,#8854,#8855,#8856));
#2570=EDGE_LOOP('',(#8857,#8858,#8859,#8860,#8861));
#2571=EDGE_LOOP('',(#8862,#8863,#8864,#8865,#8866));
#2572=EDGE_LOOP('',(#8867,#8868,#8869,#8870,#8871));
#2573=EDGE_LOOP('',(#8872,#8873,#8874,#8875,#8876));
#2574=EDGE_LOOP('',(#8877,#8878,#8879,#8880,#8881));
#2575=EDGE_LOOP('',(#8882,#8883,#8884,#8885,#8886));
#2576=EDGE_LOOP('',(#8887,#8888,#8889,#8890,#8891));
#2577=EDGE_LOOP('',(#8892,#8893,#8894,#8895,#8896));
#2578=EDGE_LOOP('',(#8897,#8898,#8899,#8900,#8901));
#2579=EDGE_LOOP('',(#8902,#8903,#8904,#8905,#8906));
#2580=EDGE_LOOP('',(#8907,#8908,#8909,#8910,#8911));
#2581=EDGE_LOOP('',(#8912,#8913,#8914,#8915,#8916));
#2582=EDGE_LOOP('',(#8917,#8918,#8919,#8920,#8921));
#2583=EDGE_LOOP('',(#8922,#8923,#8924,#8925,#8926));
#2584=EDGE_LOOP('',(#8927,#8928,#8929,#8930,#8931));
#2585=EDGE_LOOP('',(#8932,#8933,#8934,#8935,#8936));
#2586=EDGE_LOOP('',(#8937,#8938,#8939,#8940,#8941));
#2587=EDGE_LOOP('',(#8942,#8943,#8944,#8945,#8946));
#2588=EDGE_LOOP('',(#8947,#8948,#8949,#8950,#8951));
#2589=EDGE_LOOP('',(#8952,#8953,#8954,#8955,#8956));
#2590=EDGE_LOOP('',(#8957,#8958,#8959,#8960,#8961));
#2591=EDGE_LOOP('',(#8962,#8963,#8964,#8965,#8966));
#2592=EDGE_LOOP('',(#8967,#8968,#8969,#8970,#8971,#8972));
#2593=EDGE_LOOP('',(#8973,#8974,#8975,#8976,#8977));
#2594=EDGE_LOOP('',(#8978,#8979,#8980,#8981,#8982));
#2595=EDGE_LOOP('',(#8983,#8984,#8985,#8986,#8987));
#2596=EDGE_LOOP('',(#8988,#8989,#8990,#8991,#8992));
#2597=EDGE_LOOP('',(#8993,#8994,#8995,#8996,#8997));
#2598=EDGE_LOOP('',(#8998,#8999,#9000,#9001,#9002));
#2599=EDGE_LOOP('',(#9003,#9004,#9005,#9006,#9007));
#2600=EDGE_LOOP('',(#9008,#9009,#9010,#9011,#9012));
#2601=EDGE_LOOP('',(#9013,#9014,#9015,#9016,#9017));
#2602=EDGE_LOOP('',(#9018,#9019,#9020,#9021,#9022));
#2603=EDGE_LOOP('',(#9023,#9024,#9025,#9026,#9027));
#2604=EDGE_LOOP('',(#9028,#9029,#9030,#9031,#9032));
#2605=EDGE_LOOP('',(#9033,#9034,#9035,#9036,#9037));
#2606=EDGE_LOOP('',(#9038,#9039,#9040,#9041,#9042));
#2607=EDGE_LOOP('',(#9043,#9044,#9045,#9046,#9047));
#2608=EDGE_LOOP('',(#9048,#9049,#9050,#9051,#9052));
#2609=EDGE_LOOP('',(#9053,#9054,#9055,#9056,#9057));
#2610=EDGE_LOOP('',(#9058,#9059,#9060,#9061,#9062));
#2611=EDGE_LOOP('',(#9063,#9064,#9065,#9066,#9067));
#2612=EDGE_LOOP('',(#9068,#9069,#9070,#9071,#9072));
#2613=EDGE_LOOP('',(#9073,#9074,#9075,#9076,#9077));
#2614=EDGE_LOOP('',(#9078,#9079,#9080,#9081,#9082));
#2615=EDGE_LOOP('',(#9083,#9084,#9085,#9086,#9087));
#2616=EDGE_LOOP('',(#9088,#9089,#9090,#9091,#9092));
#2617=EDGE_LOOP('',(#9093,#9094,#9095,#9096,#9097));
#2618=EDGE_LOOP('',(#9098,#9099,#9100,#9101,#9102));
#2619=EDGE_LOOP('',(#9103,#9104,#9105,#9106,#9107));
#2620=EDGE_LOOP('',(#9108,#9109,#9110,#9111,#9112));
#2621=EDGE_LOOP('',(#9113,#9114,#9115,#9116,#9117));
#2622=EDGE_LOOP('',(#9118,#9119,#9120,#9121,#9122));
#2623=EDGE_LOOP('',(#9123,#9124,#9125,#9126,#9127));
#2624=EDGE_LOOP('',(#9128,#9129,#9130,#9131,#9132));
#2625=EDGE_LOOP('',(#9133,#9134,#9135,#9136,#9137));
#2626=EDGE_LOOP('',(#9138,#9139,#9140,#9141,#9142));
#2627=EDGE_LOOP('',(#9143,#9144,#9145,#9146,#9147));
#2628=EDGE_LOOP('',(#9148,#9149,#9150,#9151,#9152));
#2629=EDGE_LOOP('',(#9153,#9154,#9155,#9156,#9157));
#2630=EDGE_LOOP('',(#9158,#9159,#9160,#9161,#9162));
#2631=EDGE_LOOP('',(#9163,#9164,#9165,#9166,#9167));
#2632=EDGE_LOOP('',(#9168,#9169,#9170,#9171,#9172));
#2633=EDGE_LOOP('',(#9173,#9174,#9175,#9176,#9177));
#2634=EDGE_LOOP('',(#9178,#9179,#9180,#9181,#9182));
#2635=EDGE_LOOP('',(#9183,#9184,#9185,#9186,#9187));
#2636=EDGE_LOOP('',(#9188,#9189,#9190,#9191,#9192));
#2637=EDGE_LOOP('',(#9193,#9194,#9195,#9196,#9197));
#2638=EDGE_LOOP('',(#9198,#9199,#9200,#9201,#9202));
#2639=EDGE_LOOP('',(#9203,#9204,#9205,#9206,#9207));
#2640=EDGE_LOOP('',(#9208,#9209,#9210,#9211,#9212));
#2641=EDGE_LOOP('',(#9213,#9214,#9215,#9216,#9217));
#2642=EDGE_LOOP('',(#9218,#9219,#9220,#9221,#9222));
#2643=EDGE_LOOP('',(#9223,#9224,#9225,#9226,#9227));
#2644=EDGE_LOOP('',(#9228,#9229,#9230,#9231,#9232));
#2645=EDGE_LOOP('',(#9233,#9234,#9235,#9236,#9237));
#2646=EDGE_LOOP('',(#9238,#9239,#9240,#9241,#9242));
#2647=EDGE_LOOP('',(#9243,#9244,#9245,#9246,#9247));
#2648=EDGE_LOOP('',(#9248,#9249,#9250,#9251,#9252));
#2649=EDGE_LOOP('',(#9253,#9254,#9255,#9256,#9257));
#2650=EDGE_LOOP('',(#9258,#9259,#9260,#9261,#9262));
#2651=EDGE_LOOP('',(#9263,#9264,#9265,#9266,#9267));
#2652=EDGE_LOOP('',(#9268,#9269,#9270,#9271,#9272));
#2653=EDGE_LOOP('',(#9273,#9274,#9275,#9276,#9277));
#2654=EDGE_LOOP('',(#9278,#9279,#9280,#9281,#9282));
#2655=EDGE_LOOP('',(#9283,#9284,#9285,#9286,#9287));
#2656=EDGE_LOOP('',(#9288,#9289,#9290,#9291,#9292));
#2657=EDGE_LOOP('',(#9293,#9294,#9295,#9296,#9297));
#2658=EDGE_LOOP('',(#9298,#9299,#9300,#9301,#9302));
#2659=EDGE_LOOP('',(#9303,#9304,#9305,#9306,#9307));
#2660=EDGE_LOOP('',(#9308,#9309,#9310,#9311,#9312));
#2661=EDGE_LOOP('',(#9313,#9314,#9315,#9316,#9317));
#2662=EDGE_LOOP('',(#9318,#9319,#9320,#9321,#9322));
#2663=EDGE_LOOP('',(#9323,#9324,#9325,#9326,#9327));
#2664=EDGE_LOOP('',(#9328,#9329,#9330,#9331,#9332));
#2665=EDGE_LOOP('',(#9333,#9334,#9335,#9336,#9337));
#2666=EDGE_LOOP('',(#9338,#9339,#9340,#9341,#9342));
#2667=EDGE_LOOP('',(#9343,#9344,#9345,#9346,#9347));
#2668=EDGE_LOOP('',(#9348,#9349,#9350,#9351,#9352));
#2669=EDGE_LOOP('',(#9353,#9354,#9355,#9356,#9357));
#2670=EDGE_LOOP('',(#9358,#9359,#9360,#9361,#9362));
#2671=EDGE_LOOP('',(#9363,#9364,#9365,#9366,#9367));
#2672=EDGE_LOOP('',(#9368,#9369,#9370,#9371,#9372));
#2673=EDGE_LOOP('',(#9373,#9374,#9375,#9376,#9377));
#2674=EDGE_LOOP('',(#9378,#9379,#9380,#9381,#9382));
#2675=EDGE_LOOP('',(#9383,#9384,#9385,#9386,#9387));
#2676=EDGE_LOOP('',(#9388,#9389,#9390,#9391,#9392));
#2677=EDGE_LOOP('',(#9393,#9394,#9395,#9396,#9397));
#2678=EDGE_LOOP('',(#9398,#9399,#9400,#9401,#9402));
#2679=EDGE_LOOP('',(#9403,#9404,#9405,#9406,#9407));
#2680=EDGE_LOOP('',(#9408,#9409,#9410,#9411,#9412));
#2681=EDGE_LOOP('',(#9413,#9414,#9415,#9416,#9417));
#2682=EDGE_LOOP('',(#9418,#9419,#9420,#9421,#9422));
#2683=EDGE_LOOP('',(#9423,#9424,#9425,#9426,#9427));
#2684=EDGE_LOOP('',(#9428,#9429,#9430,#9431,#9432));
#2685=EDGE_LOOP('',(#9433,#9434,#9435,#9436,#9437));
#2686=EDGE_LOOP('',(#9438,#9439,#9440,#9441,#9442));
#2687=EDGE_LOOP('',(#9443,#9444,#9445,#9446,#9447));
#2688=EDGE_LOOP('',(#9448,#9449,#9450,#9451,#9452));
#2689=EDGE_LOOP('',(#9453,#9454,#9455,#9456,#9457));
#2690=EDGE_LOOP('',(#9458,#9459,#9460,#9461,#9462));
#2691=EDGE_LOOP('',(#9463,#9464,#9465,#9466));
#2692=EDGE_LOOP('',(#9467,#9468,#9469,#9470));
#2693=EDGE_LOOP('',(#9471,#9472,#9473,#9474));
#2694=EDGE_LOOP('',(#9475,#9476,#9477,#9478));
#2695=EDGE_LOOP('',(#9479,#9480,#9481,#9482));
#2696=EDGE_LOOP('',(#9483,#9484,#9485,#9486));
#2697=EDGE_LOOP('',(#9487,#9488,#9489,#9490));
#2698=EDGE_LOOP('',(#9491,#9492,#9493,#9494));
#2699=EDGE_LOOP('',(#9495,#9496,#9497,#9498));
#2700=EDGE_LOOP('',(#9499,#9500,#9501,#9502));
#2701=EDGE_LOOP('',(#9503,#9504,#9505,#9506));
#2702=EDGE_LOOP('',(#9507,#9508,#9509,#9510));
#2703=EDGE_LOOP('',(#9511,#9512,#9513,#9514));
#2704=EDGE_LOOP('',(#9515,#9516,#9517,#9518,#9519,#9520,#9521,#9522));
#2705=EDGE_LOOP('',(#9523,#9524,#9525,#9526));
#2706=EDGE_LOOP('',(#9527,#9528,#9529,#9530));
#2707=EDGE_LOOP('',(#9531,#9532,#9533,#9534));
#2708=EDGE_LOOP('',(#9535,#9536,#9537,#9538));
#2709=EDGE_LOOP('',(#9539,#9540,#9541,#9542,#9543,#9544,#9545,#9546,#9547,
#9548));
#2710=EDGE_LOOP('',(#9549));
#2711=EDGE_LOOP('',(#9550));
#2712=EDGE_LOOP('',(#9551,#9552,#9553,#9554,#9555,#9556,#9557,#9558));
#2713=EDGE_LOOP('',(#9559,#9560,#9561,#9562,#9563,#9564,#9565,#9566,#9567,
#9568));
#2714=EDGE_LOOP('',(#9569));
#2715=EDGE_LOOP('',(#9570));
#2716=EDGE_LOOP('',(#9571,#9572,#9573,#9574));
#2717=EDGE_LOOP('',(#9575,#9576,#9577,#9578));
#2718=EDGE_LOOP('',(#9579));
#2719=EDGE_LOOP('',(#9580,#9581,#9582,#9583,#9584,#9585,#9586,#9587,#9588,
#9589));
#2720=EDGE_LOOP('',(#9590));
#2721=EDGE_LOOP('',(#9591));
#2722=EDGE_LOOP('',(#9592,#9593,#9594,#9595));
#2723=EDGE_LOOP('',(#9596));
#2724=EDGE_LOOP('',(#9597,#9598,#9599,#9600,#9601,#9602,#9603,#9604,#9605,
#9606));
#2725=EDGE_LOOP('',(#9607));
#2726=EDGE_LOOP('',(#9608));
#2727=EDGE_LOOP('',(#9609,#9610,#9611,#9612));
#2728=EDGE_LOOP('',(#9613,#9614,#9615,#9616));
#2729=EDGE_LOOP('',(#9617));
#2730=EDGE_LOOP('',(#9618));
#2731=EDGE_LOOP('',(#9619));
#2732=EDGE_LOOP('',(#9620));
#2733=EDGE_LOOP('',(#9621));
#2734=EDGE_LOOP('',(#9622));
#2735=EDGE_LOOP('',(#9623));
#2736=EDGE_LOOP('',(#9624));
#2737=EDGE_LOOP('',(#9625,#9626,#9627,#9628));
#2738=EDGE_LOOP('',(#9629));
#2739=EDGE_LOOP('',(#9630));
#2740=EDGE_LOOP('',(#9631));
#2741=EDGE_LOOP('',(#9632));
#2742=EDGE_LOOP('',(#9633));
#2743=EDGE_LOOP('',(#9634));
#2744=EDGE_LOOP('',(#9635));
#2745=EDGE_LOOP('',(#9636));
#2746=EDGE_LOOP('',(#9637,#9638,#9639,#9640));
#2747=EDGE_LOOP('',(#9641,#9642,#9643,#9644));
#2748=EDGE_LOOP('',(#9645,#9646,#9647,#9648));
#2749=EDGE_LOOP('',(#9649,#9650,#9651,#9652));
#2750=EDGE_LOOP('',(#9653,#9654,#9655,#9656));
#2751=EDGE_LOOP('',(#9657,#9658,#9659,#9660));
#2752=EDGE_LOOP('',(#9661,#9662,#9663,#9664));
#2753=EDGE_LOOP('',(#9665,#9666,#9667,#9668));
#2754=EDGE_LOOP('',(#9669,#9670,#9671,#9672));
#2755=EDGE_LOOP('',(#9673,#9674,#9675,#9676));
#2756=EDGE_LOOP('',(#9677,#9678,#9679,#9680));
#2757=EDGE_LOOP('',(#9681,#9682,#9683,#9684));
#2758=EDGE_LOOP('',(#9685,#9686,#9687,#9688));
#2759=EDGE_LOOP('',(#9689,#9690,#9691,#9692));
#2760=EDGE_LOOP('',(#9693,#9694,#9695,#9696));
#2761=EDGE_LOOP('',(#9697,#9698,#9699,#9700));
#2762=EDGE_LOOP('',(#9701,#9702,#9703,#9704));
#2763=EDGE_LOOP('',(#9705,#9706,#9707));
#2764=EDGE_LOOP('',(#9708,#9709,#9710));
#2765=EDGE_LOOP('',(#9711,#9712,#9713,#9714));
#2766=EDGE_LOOP('',(#9715,#9716,#9717,#9718));
#2767=EDGE_LOOP('',(#9719,#9720,#9721,#9722));
#2768=EDGE_LOOP('',(#9723,#9724,#9725,#9726));
#2769=EDGE_LOOP('',(#9727,#9728,#9729,#9730));
#2770=EDGE_LOOP('',(#9731,#9732,#9733,#9734));
#2771=EDGE_LOOP('',(#9735,#9736,#9737));
#2772=EDGE_LOOP('',(#9738,#9739,#9740));
#2773=EDGE_LOOP('',(#9741,#9742,#9743));
#2774=EDGE_LOOP('',(#9744,#9745,#9746));
#2775=EDGE_LOOP('',(#9747,#9748,#9749,#9750));
#2776=EDGE_LOOP('',(#9751,#9752,#9753,#9754));
#2777=EDGE_LOOP('',(#9755,#9756,#9757,#9758));
#2778=EDGE_LOOP('',(#9759,#9760,#9761,#9762));
#2779=EDGE_LOOP('',(#9763,#9764,#9765));
#2780=EDGE_LOOP('',(#9766,#9767,#9768));
#2781=EDGE_LOOP('',(#9769,#9770,#9771,#9772));
#2782=EDGE_LOOP('',(#9773,#9774,#9775,#9776));
#2783=EDGE_LOOP('',(#9777,#9778,#9779,#9780));
#2784=EDGE_LOOP('',(#9781,#9782,#9783,#9784));
#2785=EDGE_LOOP('',(#9785,#9786,#9787,#9788));
#2786=EDGE_LOOP('',(#9789,#9790,#9791,#9792));
#2787=EDGE_LOOP('',(#9793,#9794,#9795,#9796));
#2788=EDGE_LOOP('',(#9797,#9798,#9799,#9800));
#2789=EDGE_LOOP('',(#9801,#9802,#9803,#9804));
#2790=EDGE_LOOP('',(#9805));
#2791=EDGE_LOOP('',(#9806));
#2792=EDGE_LOOP('',(#9807));
#2793=EDGE_LOOP('',(#9808));
#2794=EDGE_LOOP('',(#9809));
#2795=EDGE_LOOP('',(#9810));
#2796=EDGE_LOOP('',(#9811));
#2797=EDGE_LOOP('',(#9812));
#2798=EDGE_LOOP('',(#9813));
#2799=EDGE_LOOP('',(#9814));
#2800=EDGE_LOOP('',(#9815));
#2801=EDGE_LOOP('',(#9816));
#2802=EDGE_LOOP('',(#9817));
#2803=EDGE_LOOP('',(#9818));
#2804=EDGE_LOOP('',(#9819));
#2805=EDGE_LOOP('',(#9820));
#2806=EDGE_LOOP('',(#9821,#9822,#9823,#9824));
#2807=EDGE_LOOP('',(#9825,#9826,#9827,#9828));
#2808=EDGE_LOOP('',(#9829,#9830,#9831,#9832));
#2809=EDGE_LOOP('',(#9833,#9834,#9835,#9836));
#2810=EDGE_LOOP('',(#9837,#9838,#9839,#9840));
#2811=EDGE_LOOP('',(#9841,#9842,#9843,#9844));
#2812=EDGE_LOOP('',(#9845,#9846,#9847,#9848));
#2813=EDGE_LOOP('',(#9849,#9850,#9851,#9852));
#2814=EDGE_LOOP('',(#9853));
#2815=EDGE_LOOP('',(#9854));
#2816=EDGE_LOOP('',(#9855));
#2817=EDGE_LOOP('',(#9856));
#2818=EDGE_LOOP('',(#9857));
#2819=EDGE_LOOP('',(#9858));
#2820=EDGE_LOOP('',(#9859));
#2821=EDGE_LOOP('',(#9860));
#2822=EDGE_LOOP('',(#9861));
#2823=EDGE_LOOP('',(#9862));
#2824=EDGE_LOOP('',(#9863));
#2825=EDGE_LOOP('',(#9864));
#2826=EDGE_LOOP('',(#9865));
#2827=EDGE_LOOP('',(#9866));
#2828=EDGE_LOOP('',(#9867));
#2829=EDGE_LOOP('',(#9868));
#2830=EDGE_LOOP('',(#9869,#9870,#9871,#9872));
#2831=EDGE_LOOP('',(#9873,#9874,#9875,#9876,#9877));
#2832=EDGE_LOOP('',(#9878,#9879,#9880,#9881,#9882));
#2833=EDGE_LOOP('',(#9883,#9884,#9885,#9886));
#2834=EDGE_LOOP('',(#9887));
#2835=EDGE_LOOP('',(#9888));
#2836=EDGE_LOOP('',(#9889));
#2837=EDGE_LOOP('',(#9890));
#2838=EDGE_LOOP('',(#9891,#9892,#9893,#9894));
#2839=EDGE_LOOP('',(#9895,#9896,#9897,#9898));
#2840=EDGE_LOOP('',(#9899,#9900,#9901,#9902));
#2841=EDGE_LOOP('',(#9903,#9904,#9905,#9906));
#2842=EDGE_LOOP('',(#9907,#9908,#9909,#9910));
#2843=EDGE_LOOP('',(#9911,#9912,#9913,#9914));
#2844=EDGE_LOOP('',(#9915,#9916,#9917,#9918));
#2845=EDGE_LOOP('',(#9919,#9920,#9921,#9922,#9923,#9924));
#2846=EDGE_LOOP('',(#9925));
#2847=EDGE_LOOP('',(#9926,#9927,#9928,#9929,#9930,#9931));
#2848=EDGE_LOOP('',(#9932));
#2849=EDGE_LOOP('',(#9933,#9934,#9935,#9936));
#2850=EDGE_LOOP('',(#9937,#9938,#9939,#9940));
#2851=EDGE_LOOP('',(#9941,#9942,#9943,#9944));
#2852=EDGE_LOOP('',(#9945,#9946,#9947,#9948));
#2853=EDGE_LOOP('',(#9949,#9950,#9951,#9952));
#2854=EDGE_LOOP('',(#9953,#9954,#9955,#9956));
#2855=EDGE_LOOP('',(#9957,#9958,#9959,#9960));
#2856=EDGE_LOOP('',(#9961,#9962,#9963,#9964));
#2857=EDGE_LOOP('',(#9965,#9966,#9967,#9968,#9969,#9970,#9971,#9972,#9973,
#9974,#9975,#9976,#9977,#9978));
#2858=EDGE_LOOP('',(#9979,#9980,#9981,#9982,#9983,#9984,#9985,#9986,#9987,
#9988,#9989,#9990,#9991,#9992));
#2859=EDGE_LOOP('',(#9993,#9994,#9995,#9996));
#2860=EDGE_LOOP('',(#9997,#9998,#9999,#10000));
#2861=EDGE_LOOP('',(#10001,#10002,#10003,#10004));
#2862=EDGE_LOOP('',(#10005,#10006,#10007,#10008));
#2863=EDGE_LOOP('',(#10009,#10010,#10011,#10012));
#2864=EDGE_LOOP('',(#10013,#10014,#10015,#10016));
#2865=EDGE_LOOP('',(#10017,#10018,#10019,#10020));
#2866=EDGE_LOOP('',(#10021,#10022,#10023,#10024));
#2867=EDGE_LOOP('',(#10025));
#2868=EDGE_LOOP('',(#10026));
#2869=EDGE_LOOP('',(#10027));
#2870=EDGE_LOOP('',(#10028));
#2871=LINE('',#14049,#3172);
#2872=LINE('',#14055,#3173);
#2873=LINE('',#14061,#3174);
#2874=LINE('',#14067,#3175);
#2875=LINE('',#14073,#3176);
#2876=LINE('',#14079,#3177);
#2877=LINE('',#14085,#3178);
#2878=LINE('',#14091,#3179);
#2879=LINE('',#14097,#3180);
#2880=LINE('',#14103,#3181);
#2881=LINE('',#14109,#3182);
#2882=LINE('',#14114,#3183);
#2883=LINE('',#14116,#3184);
#2884=LINE('',#14118,#3185);
#2885=LINE('',#14120,#3186);
#2886=LINE('',#14122,#3187);
#2887=LINE('',#14124,#3188);
#2888=LINE('',#14126,#3189);
#2889=LINE('',#14127,#3190);
#2890=LINE('',#14131,#3191);
#2891=LINE('',#14133,#3192);
#2892=LINE('',#14135,#3193);
#2893=LINE('',#14136,#3194);
#2894=LINE('',#14140,#3195);
#2895=LINE('',#14142,#3196);
#2896=LINE('',#14144,#3197);
#2897=LINE('',#14145,#3198);
#2898=LINE('',#14149,#3199);
#2899=LINE('',#14151,#3200);
#2900=LINE('',#14153,#3201);
#2901=LINE('',#14154,#3202);
#2902=LINE('',#14158,#3203);
#2903=LINE('',#14160,#3204);
#2904=LINE('',#14162,#3205);
#2905=LINE('',#14163,#3206);
#2906=LINE('',#14166,#3207);
#2907=LINE('',#14168,#3208);
#2908=LINE('',#14170,#3209);
#2909=LINE('',#14172,#3210);
#2910=LINE('',#14178,#3211);
#2911=LINE('',#14180,#3212);
#2912=LINE('',#14182,#3213);
#2913=LINE('',#14184,#3214);
#2914=LINE('',#14186,#3215);
#2915=LINE('',#14188,#3216);
#2916=LINE('',#14189,#3217);
#2917=LINE('',#14192,#3218);
#2918=LINE('',#14194,#3219);
#2919=LINE('',#14195,#3220);
#2920=LINE('',#14200,#3221);
#2921=LINE('',#14202,#3222);
#2922=LINE('',#14208,#3223);
#2923=LINE('',#14210,#3224);
#2924=LINE('',#14211,#3225);
#2925=LINE('',#14214,#3226);
#2926=LINE('',#14215,#3227);
#2927=LINE('',#14219,#3228);
#2928=LINE('',#14220,#3229);
#2929=LINE('',#14224,#3230);
#2930=LINE('',#14229,#3231);
#2931=LINE('',#14231,#3232);
#2932=LINE('',#14233,#3233);
#2933=LINE('',#14234,#3234);
#2934=LINE('',#14253,#3235);
#2935=LINE('',#14276,#3236);
#2936=LINE('',#14299,#3237);
#2937=LINE('',#14340,#3238);
#2938=LINE('',#14418,#3239);
#2939=LINE('',#14496,#3240);
#2940=LINE('',#14577,#3241);
#2941=LINE('',#14658,#3242);
#2942=LINE('',#14735,#3243);
#2943=LINE('',#14774,#3244);
#2944=LINE('',#14797,#3245);
#2945=LINE('',#14824,#3246);
#2946=LINE('',#14831,#3247);
#2947=LINE('',#14835,#3248);
#2948=LINE('',#14839,#3249);
#2949=LINE('',#14844,#3250);
#2950=LINE('',#14849,#3251);
#2951=LINE('',#14930,#3252);
#2952=LINE('',#14932,#3253);
#2953=LINE('',#15161,#3254);
#2954=LINE('',#16068,#3255);
#2955=LINE('',#16071,#3256);
#2956=LINE('',#16074,#3257);
#2957=LINE('',#17207,#3258);
#2958=LINE('',#17209,#3259);
#2959=LINE('',#17210,#3260);
#2960=LINE('',#17213,#3261);
#2961=LINE('',#17214,#3262);
#2962=LINE('',#17217,#3263);
#2963=LINE('',#17218,#3264);
#2964=LINE('',#17220,#3265);
#2965=LINE('',#17230,#3266);
#2966=LINE('',#17236,#3267);
#2967=LINE('',#17243,#3268);
#2968=LINE('',#17246,#3269);
#2969=LINE('',#17249,#3270);
#2970=LINE('',#17255,#3271);
#2971=LINE('',#17259,#3272);
#2972=LINE('',#17263,#3273);
#2973=LINE('',#17268,#3274);
#2974=LINE('',#17269,#3275);
#2975=LINE('',#17270,#3276);
#2976=LINE('',#17274,#3277);
#2977=LINE('',#17276,#3278);
#2978=LINE('',#17277,#3279);
#2979=LINE('',#17280,#3280);
#2980=LINE('',#17282,#3281);
#2981=LINE('',#17283,#3282);
#2982=LINE('',#17285,#3283);
#2983=LINE('',#17286,#3284);
#2984=LINE('',#17292,#3285);
#2985=LINE('',#17294,#3286);
#2986=LINE('',#17295,#3287);
#2987=LINE('',#17297,#3288);
#2988=LINE('',#17299,#3289);
#2989=LINE('',#19756,#3290);
#2990=LINE('',#20400,#3291);
#2991=LINE('',#20403,#3292);
#2992=LINE('',#21058,#3293);
#2993=LINE('',#22839,#3294);
#2994=LINE('',#22841,#3295);
#2995=LINE('',#22842,#3296);
#2996=LINE('',#22845,#3297);
#2997=LINE('',#22847,#3298);
#2998=LINE('',#22848,#3299);
#2999=LINE('',#22850,#3300);
#3000=LINE('',#22852,#3301);
#3001=LINE('',#37226,#3302);
#3002=LINE('',#37232,#3303);
#3003=LINE('',#37238,#3304);
#3004=LINE('',#37244,#3305);
#3005=LINE('',#37250,#3306);
#3006=LINE('',#37256,#3307);
#3007=LINE('',#37262,#3308);
#3008=LINE('',#37268,#3309);
#3009=LINE('',#37274,#3310);
#3010=LINE('',#37280,#3311);
#3011=LINE('',#37286,#3312);
#3012=LINE('',#37292,#3313);
#3013=LINE('',#37298,#3314);
#3014=LINE('',#37303,#3315);
#3015=LINE('',#37305,#3316);
#3016=LINE('',#37307,#3317);
#3017=LINE('',#37309,#3318);
#3018=LINE('',#37311,#3319);
#3019=LINE('',#37313,#3320);
#3020=LINE('',#37315,#3321);
#3021=LINE('',#37316,#3322);
#3022=LINE('',#37320,#3323);
#3023=LINE('',#37322,#3324);
#3024=LINE('',#37324,#3325);
#3025=LINE('',#37325,#3326);
#3026=LINE('',#37329,#3327);
#3027=LINE('',#37331,#3328);
#3028=LINE('',#37333,#3329);
#3029=LINE('',#37334,#3330);
#3030=LINE('',#37338,#3331);
#3031=LINE('',#37340,#3332);
#3032=LINE('',#37342,#3333);
#3033=LINE('',#37343,#3334);
#3034=LINE('',#37347,#3335);
#3035=LINE('',#37349,#3336);
#3036=LINE('',#37351,#3337);
#3037=LINE('',#37352,#3338);
#3038=LINE('',#37355,#3339);
#3039=LINE('',#37361,#3340);
#3040=LINE('',#37363,#3341);
#3041=LINE('',#37364,#3342);
#3042=LINE('',#37367,#3343);
#3043=LINE('',#37369,#3344);
#3044=LINE('',#37371,#3345);
#3045=LINE('',#37373,#3346);
#3046=LINE('',#37375,#3347);
#3047=LINE('',#37377,#3348);
#3048=LINE('',#37378,#3349);
#3049=LINE('',#37381,#3350);
#3050=LINE('',#37386,#3351);
#3051=LINE('',#37387,#3352);
#3052=LINE('',#37389,#3353);
#3053=LINE('',#37391,#3354);
#3054=LINE('',#37395,#3355);
#3055=LINE('',#37397,#3356);
#3056=LINE('',#37398,#3357);
#3057=LINE('',#37403,#3358);
#3058=LINE('',#37404,#3359);
#3059=LINE('',#37410,#3360);
#3060=LINE('',#37411,#3361);
#3061=LINE('',#37413,#3362);
#3062=LINE('',#37418,#3363);
#3063=LINE('',#37420,#3364);
#3064=LINE('',#37422,#3365);
#3065=LINE('',#37423,#3366);
#3066=LINE('',#37442,#3367);
#3067=LINE('',#37444,#3368);
#3068=LINE('',#37446,#3369);
#3069=LINE('',#37447,#3370);
#3070=LINE('',#37451,#3371);
#3071=LINE('',#37453,#3372);
#3072=LINE('',#37455,#3373);
#3073=LINE('',#37456,#3374);
#3074=LINE('',#37460,#3375);
#3075=LINE('',#37462,#3376);
#3076=LINE('',#37464,#3377);
#3077=LINE('',#37465,#3378);
#3078=LINE('',#37469,#3379);
#3079=LINE('',#37471,#3380);
#3080=LINE('',#37473,#3381);
#3081=LINE('',#37474,#3382);
#3082=LINE('',#37478,#3383);
#3083=LINE('',#37480,#3384);
#3084=LINE('',#37482,#3385);
#3085=LINE('',#37483,#3386);
#3086=LINE('',#37487,#3387);
#3087=LINE('',#37489,#3388);
#3088=LINE('',#37491,#3389);
#3089=LINE('',#37492,#3390);
#3090=LINE('',#37542,#3391);
#3091=LINE('',#37548,#3392);
#3092=LINE('',#37554,#3393);
#3093=LINE('',#37560,#3394);
#3094=LINE('',#37566,#3395);
#3095=LINE('',#37572,#3396);
#3096=LINE('',#37578,#3397);
#3097=LINE('',#37584,#3398);
#3098=LINE('',#37593,#3399);
#3099=LINE('',#37599,#3400);
#3100=LINE('',#37605,#3401);
#3101=LINE('',#37611,#3402);
#3102=LINE('',#37617,#3403);
#3103=LINE('',#37623,#3404);
#3104=LINE('',#37629,#3405);
#3105=LINE('',#37635,#3406);
#3106=LINE('',#37644,#3407);
#3107=LINE('',#37657,#3408);
#3108=LINE('',#37661,#3409);
#3109=LINE('',#37670,#3410);
#3110=LINE('',#37675,#3411);
#3111=LINE('',#37677,#3412);
#3112=LINE('',#37679,#3413);
#3113=LINE('',#37680,#3414);
#3114=LINE('',#37683,#3415);
#3115=LINE('',#37685,#3416);
#3116=LINE('',#37686,#3417);
#3117=LINE('',#37689,#3418);
#3118=LINE('',#37691,#3419);
#3119=LINE('',#37692,#3420);
#3120=LINE('',#37695,#3421);
#3121=LINE('',#37697,#3422);
#3122=LINE('',#37698,#3423);
#3123=LINE('',#37701,#3424);
#3124=LINE('',#37703,#3425);
#3125=LINE('',#37704,#3426);
#3126=LINE('',#37706,#3427);
#3127=LINE('',#37707,#3428);
#3128=LINE('',#37715,#3429);
#3129=LINE('',#37717,#3430);
#3130=LINE('',#37719,#3431);
#3131=LINE('',#37720,#3432);
#3132=LINE('',#37724,#3433);
#3133=LINE('',#37726,#3434);
#3134=LINE('',#37728,#3435);
#3135=LINE('',#37729,#3436);
#3136=LINE('',#37733,#3437);
#3137=LINE('',#37735,#3438);
#3138=LINE('',#37737,#3439);
#3139=LINE('',#37738,#3440);
#3140=LINE('',#37742,#3441);
#3141=LINE('',#37744,#3442);
#3142=LINE('',#37746,#3443);
#3143=LINE('',#37747,#3444);
#3144=LINE('',#37750,#3445);
#3145=LINE('',#37752,#3446);
#3146=LINE('',#37753,#3447);
#3147=LINE('',#37756,#3448);
#3148=LINE('',#37758,#3449);
#3149=LINE('',#37759,#3450);
#3150=LINE('',#37763,#3451);
#3151=LINE('',#37765,#3452);
#3152=LINE('',#37767,#3453);
#3153=LINE('',#37768,#3454);
#3154=LINE('',#37772,#3455);
#3155=LINE('',#37774,#3456);
#3156=LINE('',#37776,#3457);
#3157=LINE('',#37777,#3458);
#3158=LINE('',#37779,#3459);
#3159=LINE('',#37780,#3460);
#3160=LINE('',#37781,#3461);
#3161=LINE('',#37782,#3462);
#3162=LINE('',#37783,#3463);
#3163=LINE('',#37784,#3464);
#3164=LINE('',#37786,#3465);
#3165=LINE('',#37787,#3466);
#3166=LINE('',#37788,#3467);
#3167=LINE('',#37789,#3468);
#3168=LINE('',#37790,#3469);
#3169=LINE('',#37791,#3470);
#3170=LINE('',#37803,#3471);
#3171=LINE('',#37809,#3472);
#3172=VECTOR('',#11898,2.5);
#3173=VECTOR('',#11905,2.5);
#3174=VECTOR('',#11912,2.5);
#3175=VECTOR('',#11919,2.5);
#3176=VECTOR('',#11926,3.);
#3177=VECTOR('',#11933,2.99999999999999);
#3178=VECTOR('',#11940,3.);
#3179=VECTOR('',#11947,3.);
#3180=VECTOR('',#11954,3.);
#3181=VECTOR('',#11961,3.);
#3182=VECTOR('',#11968,17.5);
#3183=VECTOR('',#11973,1000.);
#3184=VECTOR('',#11974,1000.);
#3185=VECTOR('',#11975,1000.);
#3186=VECTOR('',#11976,1000.);
#3187=VECTOR('',#11977,1000.);
#3188=VECTOR('',#11978,1000.);
#3189=VECTOR('',#11979,1000.);
#3190=VECTOR('',#11980,1000.);
#3191=VECTOR('',#11983,1000.);
#3192=VECTOR('',#11984,1000.);
#3193=VECTOR('',#11985,1000.);
#3194=VECTOR('',#11986,1000.);
#3195=VECTOR('',#11989,1000.);
#3196=VECTOR('',#11990,1000.);
#3197=VECTOR('',#11991,1000.);
#3198=VECTOR('',#11992,1000.);
#3199=VECTOR('',#11995,1000.);
#3200=VECTOR('',#11996,1000.);
#3201=VECTOR('',#11997,1000.);
#3202=VECTOR('',#11998,1000.);
#3203=VECTOR('',#12001,1000.);
#3204=VECTOR('',#12002,1000.);
#3205=VECTOR('',#12003,1000.);
#3206=VECTOR('',#12004,1000.);
#3207=VECTOR('',#12007,1000.);
#3208=VECTOR('',#12008,1000.);
#3209=VECTOR('',#12009,1000.);
#3210=VECTOR('',#12010,1000.);
#3211=VECTOR('',#12019,1000.);
#3212=VECTOR('',#12020,1000.);
#3213=VECTOR('',#12021,1000.);
#3214=VECTOR('',#12022,1000.);
#3215=VECTOR('',#12023,1000.);
#3216=VECTOR('',#12024,1000.);
#3217=VECTOR('',#12025,1000.);
#3218=VECTOR('',#12028,1000.);
#3219=VECTOR('',#12029,1000.);
#3220=VECTOR('',#12030,1000.);
#3221=VECTOR('',#12039,1000.);
#3222=VECTOR('',#12042,1000.);
#3223=VECTOR('',#12051,1000.);
#3224=VECTOR('',#12052,1000.);
#3225=VECTOR('',#12053,1000.);
#3226=VECTOR('',#12056,1000.);
#3227=VECTOR('',#12057,1000.);
#3228=VECTOR('',#12062,1000.);
#3229=VECTOR('',#12063,1000.);
#3230=VECTOR('',#12070,1000.);
#3231=VECTOR('',#12075,1000.);
#3232=VECTOR('',#12076,1000.);
#3233=VECTOR('',#12077,1000.);
#3234=VECTOR('',#12078,1000.);
#3235=VECTOR('',#12111,9.49999999999999);
#3236=VECTOR('',#12112,1000.);
#3237=VECTOR('',#12113,9.49999999999999);
#3238=VECTOR('',#12118,9.49999999999999);
#3239=VECTOR('',#12121,9.49999999999999);
#3240=VECTOR('',#12124,9.49999999999999);
#3241=VECTOR('',#12127,9.49999999999999);
#3242=VECTOR('',#12130,9.49999999999999);
#3243=VECTOR('',#12135,9.49999999999999);
#3244=VECTOR('',#12136,9.49999999999999);
#3245=VECTOR('',#12137,1000.);
#3246=VECTOR('',#12144,7.);
#3247=VECTOR('',#12151,1000.);
#3248=VECTOR('',#12154,7.49999999999999);
#3249=VECTOR('',#12159,1000.);
#3250=VECTOR('',#12164,7.99999999999999);
#3251=VECTOR('',#12171,7.5);
#3252=VECTOR('',#12182,1000.);
#3253=VECTOR('',#12183,1000.);
#3254=VECTOR('',#12186,1000.);
#3255=VECTOR('',#12189,1000.);
#3256=VECTOR('',#12192,1000.);
#3257=VECTOR('',#12195,1000.);
#3258=VECTOR('',#12198,1000.);
#3259=VECTOR('',#12199,1000.);
#3260=VECTOR('',#12200,1000.);
#3261=VECTOR('',#12203,1000.);
#3262=VECTOR('',#12204,1000.);
#3263=VECTOR('',#12207,1000.);
#3264=VECTOR('',#12208,1000.);
#3265=VECTOR('',#12211,1000.);
#3266=VECTOR('',#12224,6.95000000000004);
#3267=VECTOR('',#12231,7.5);
#3268=VECTOR('',#12238,1000.);
#3269=VECTOR('',#12241,1000.);
#3270=VECTOR('',#12244,7.45);
#3271=VECTOR('',#12251,6.25);
#3272=VECTOR('',#12254,1000.);
#3273=VECTOR('',#12257,1000.);
#3274=VECTOR('',#12262,1000.);
#3275=VECTOR('',#12263,1000.);
#3276=VECTOR('',#12264,1000.);
#3277=VECTOR('',#12269,1000.);
#3278=VECTOR('',#12270,1000.);
#3279=VECTOR('',#12271,1000.);
#3280=VECTOR('',#12274,1000.);
#3281=VECTOR('',#12275,1000.);
#3282=VECTOR('',#12276,1000.);
#3283=VECTOR('',#12279,1000.);
#3284=VECTOR('',#12280,1000.);
#3285=VECTOR('',#12289,1000.);
#3286=VECTOR('',#12290,1000.);
#3287=VECTOR('',#12291,1000.);
#3288=VECTOR('',#12294,1000.);
#3289=VECTOR('',#12297,1000.);
#3290=VECTOR('',#12612,41.5);
#3291=VECTOR('',#12663,1000.);
#3292=VECTOR('',#12666,1000.);
#3293=VECTOR('',#12713,43.5);
#3294=VECTOR('',#12938,1000.);
#3295=VECTOR('',#12939,1000.);
#3296=VECTOR('',#12940,1000.);
#3297=VECTOR('',#12943,1000.);
#3298=VECTOR('',#12944,1000.);
#3299=VECTOR('',#12945,1000.);
#3300=VECTOR('',#12948,1000.);
#3301=VECTOR('',#12951,1000.);
#3302=VECTOR('',#13312,4.);
#3303=VECTOR('',#13319,4.);
#3304=VECTOR('',#13326,2.5);
#3305=VECTOR('',#13333,2.5);
#3306=VECTOR('',#13340,2.5);
#3307=VECTOR('',#13347,2.5);
#3308=VECTOR('',#13354,3.);
#3309=VECTOR('',#13361,2.99999999999999);
#3310=VECTOR('',#13368,3.);
#3311=VECTOR('',#13375,3.);
#3312=VECTOR('',#13382,3.);
#3313=VECTOR('',#13389,3.);
#3314=VECTOR('',#13396,17.5);
#3315=VECTOR('',#13401,1000.);
#3316=VECTOR('',#13402,1000.);
#3317=VECTOR('',#13403,1000.);
#3318=VECTOR('',#13404,1000.);
#3319=VECTOR('',#13405,1000.);
#3320=VECTOR('',#13406,1000.);
#3321=VECTOR('',#13407,1000.);
#3322=VECTOR('',#13408,1000.);
#3323=VECTOR('',#13411,1000.);
#3324=VECTOR('',#13412,1000.);
#3325=VECTOR('',#13413,1000.);
#3326=VECTOR('',#13414,1000.);
#3327=VECTOR('',#13417,1000.);
#3328=VECTOR('',#13418,1000.);
#3329=VECTOR('',#13419,1000.);
#3330=VECTOR('',#13420,1000.);
#3331=VECTOR('',#13423,1000.);
#3332=VECTOR('',#13424,1000.);
#3333=VECTOR('',#13425,1000.);
#3334=VECTOR('',#13426,1000.);
#3335=VECTOR('',#13429,1000.);
#3336=VECTOR('',#13430,1000.);
#3337=VECTOR('',#13431,1000.);
#3338=VECTOR('',#13432,1000.);
#3339=VECTOR('',#13435,1000.);
#3340=VECTOR('',#13442,1000.);
#3341=VECTOR('',#13443,1000.);
#3342=VECTOR('',#13444,1000.);
#3343=VECTOR('',#13447,1000.);
#3344=VECTOR('',#13448,1000.);
#3345=VECTOR('',#13449,1000.);
#3346=VECTOR('',#13450,1000.);
#3347=VECTOR('',#13451,1000.);
#3348=VECTOR('',#13452,1000.);
#3349=VECTOR('',#13453,1000.);
#3350=VECTOR('',#13456,1000.);
#3351=VECTOR('',#13463,1000.);
#3352=VECTOR('',#13464,1000.);
#3353=VECTOR('',#13467,1000.);
#3354=VECTOR('',#13470,1000.);
#3355=VECTOR('',#13475,1000.);
#3356=VECTOR('',#13476,1000.);
#3357=VECTOR('',#13477,1000.);
#3358=VECTOR('',#13484,1000.);
#3359=VECTOR('',#13485,1000.);
#3360=VECTOR('',#13494,1000.);
#3361=VECTOR('',#13495,1000.);
#3362=VECTOR('',#13498,1000.);
#3363=VECTOR('',#13503,1000.);
#3364=VECTOR('',#13504,1000.);
#3365=VECTOR('',#13505,1000.);
#3366=VECTOR('',#13506,1000.);
#3367=VECTOR('',#13539,1000.);
#3368=VECTOR('',#13540,1000.);
#3369=VECTOR('',#13541,1000.);
#3370=VECTOR('',#13542,1000.);
#3371=VECTOR('',#13545,1000.);
#3372=VECTOR('',#13546,1000.);
#3373=VECTOR('',#13547,1000.);
#3374=VECTOR('',#13548,1000.);
#3375=VECTOR('',#13551,1000.);
#3376=VECTOR('',#13552,1000.);
#3377=VECTOR('',#13553,1000.);
#3378=VECTOR('',#13554,1000.);
#3379=VECTOR('',#13557,1000.);
#3380=VECTOR('',#13558,1000.);
#3381=VECTOR('',#13559,1000.);
#3382=VECTOR('',#13560,1000.);
#3383=VECTOR('',#13563,1000.);
#3384=VECTOR('',#13564,1000.);
#3385=VECTOR('',#13565,1000.);
#3386=VECTOR('',#13566,1000.);
#3387=VECTOR('',#13569,1000.);
#3388=VECTOR('',#13570,1000.);
#3389=VECTOR('',#13571,1000.);
#3390=VECTOR('',#13572,1000.);
#3391=VECTOR('',#13667,3.);
#3392=VECTOR('',#13674,3.);
#3393=VECTOR('',#13681,3.);
#3394=VECTOR('',#13688,3.00000000000001);
#3395=VECTOR('',#13695,3.);
#3396=VECTOR('',#13702,3.);
#3397=VECTOR('',#13709,7.6);
#3398=VECTOR('',#13716,30.);
#3399=VECTOR('',#13729,2.5);
#3400=VECTOR('',#13736,2.5);
#3401=VECTOR('',#13743,2.5);
#3402=VECTOR('',#13750,2.5);
#3403=VECTOR('',#13757,2.5);
#3404=VECTOR('',#13764,2.5);
#3405=VECTOR('',#13771,7.6);
#3406=VECTOR('',#13778,27.5);
#3407=VECTOR('',#13791,3.47500000000001);
#3408=VECTOR('',#13808,5.00000000000001);
#3409=VECTOR('',#13813,3.97500000000001);
#3410=VECTOR('',#13826,2.5);
#3411=VECTOR('',#13831,1000.);
#3412=VECTOR('',#13832,1000.);
#3413=VECTOR('',#13833,1000.);
#3414=VECTOR('',#13834,1000.);
#3415=VECTOR('',#13837,1000.);
#3416=VECTOR('',#13838,1000.);
#3417=VECTOR('',#13839,1000.);
#3418=VECTOR('',#13842,1000.);
#3419=VECTOR('',#13843,1000.);
#3420=VECTOR('',#13844,1000.);
#3421=VECTOR('',#13847,1000.);
#3422=VECTOR('',#13848,1000.);
#3423=VECTOR('',#13849,1000.);
#3424=VECTOR('',#13852,1000.);
#3425=VECTOR('',#13853,1000.);
#3426=VECTOR('',#13854,1000.);
#3427=VECTOR('',#13857,1000.);
#3428=VECTOR('',#13858,1000.);
#3429=VECTOR('',#13869,1000.);
#3430=VECTOR('',#13870,1000.);
#3431=VECTOR('',#13871,1000.);
#3432=VECTOR('',#13872,1000.);
#3433=VECTOR('',#13875,1000.);
#3434=VECTOR('',#13876,1000.);
#3435=VECTOR('',#13877,1000.);
#3436=VECTOR('',#13878,1000.);
#3437=VECTOR('',#13881,1000.);
#3438=VECTOR('',#13882,1000.);
#3439=VECTOR('',#13883,1000.);
#3440=VECTOR('',#13884,1000.);
#3441=VECTOR('',#13887,1000.);
#3442=VECTOR('',#13888,1000.);
#3443=VECTOR('',#13889,1000.);
#3444=VECTOR('',#13890,1000.);
#3445=VECTOR('',#13893,1000.);
#3446=VECTOR('',#13894,1000.);
#3447=VECTOR('',#13895,1000.);
#3448=VECTOR('',#13898,1000.);
#3449=VECTOR('',#13899,1000.);
#3450=VECTOR('',#13900,1000.);
#3451=VECTOR('',#13903,1000.);
#3452=VECTOR('',#13904,1000.);
#3453=VECTOR('',#13905,1000.);
#3454=VECTOR('',#13906,1000.);
#3455=VECTOR('',#13909,1000.);
#3456=VECTOR('',#13910,1000.);
#3457=VECTOR('',#13911,1000.);
#3458=VECTOR('',#13912,1000.);
#3459=VECTOR('',#13915,1000.);
#3460=VECTOR('',#13916,1000.);
#3461=VECTOR('',#13917,1000.);
#3462=VECTOR('',#13918,1000.);
#3463=VECTOR('',#13919,1000.);
#3464=VECTOR('',#13920,1000.);
#3465=VECTOR('',#13923,1000.);
#3466=VECTOR('',#13924,1000.);
#3467=VECTOR('',#13925,1000.);
#3468=VECTOR('',#13926,1000.);
#3469=VECTOR('',#13927,1000.);
#3470=VECTOR('',#13928,1000.);
#3471=VECTOR('',#13947,7.5);
#3472=VECTOR('',#13954,17.5);
#3473=CIRCLE('',#10967,2.5);
#3474=CIRCLE('',#10968,2.5);
#3475=CIRCLE('',#10970,2.5);
#3476=CIRCLE('',#10971,2.5);
#3477=CIRCLE('',#10973,2.5);
#3478=CIRCLE('',#10974,2.5);
#3479=CIRCLE('',#10976,2.5);
#3480=CIRCLE('',#10977,2.5);
#3481=CIRCLE('',#10979,3.);
#3482=CIRCLE('',#10980,3.);
#3483=CIRCLE('',#10982,2.99999999999999);
#3484=CIRCLE('',#10983,2.99999999999999);
#3485=CIRCLE('',#10985,3.);
#3486=CIRCLE('',#10986,3.);
#3487=CIRCLE('',#10988,3.);
#3488=CIRCLE('',#10989,3.);
#3489=CIRCLE('',#10991,3.);
#3490=CIRCLE('',#10992,3.);
#3491=CIRCLE('',#10994,3.);
#3492=CIRCLE('',#10995,3.);
#3493=CIRCLE('',#10997,17.5);
#3494=CIRCLE('',#10998,17.5);
#3495=CIRCLE('',#11005,2.50000000000001);
#3496=CIRCLE('',#11006,17.5);
#3497=CIRCLE('',#11007,2.5);
#3498=CIRCLE('',#11010,2.5);
#3499=CIRCLE('',#11011,17.5);
#3500=CIRCLE('',#11012,2.50000000000001);
#3501=CIRCLE('',#11016,2.5);
#3502=CIRCLE('',#11017,17.5);
#3503=CIRCLE('',#11018,2.50000000000001);
#3504=CIRCLE('',#11021,2.5);
#3505=CIRCLE('',#11022,2.50000000000001);
#3506=CIRCLE('',#11023,17.5);
#3507=CIRCLE('',#11043,9.5);
#3508=CIRCLE('',#11050,9.49999999999999);
#3509=CIRCLE('',#11052,7.5);
#3510=CIRCLE('',#11053,7.5);
#3511=CIRCLE('',#11054,7.);
#3512=CIRCLE('',#11056,7.49999999999999);
#3513=CIRCLE('',#11057,7.49999999999999);
#3514=CIRCLE('',#11058,7.49999999999999);
#3515=CIRCLE('',#11059,7.49999999999999);
#3516=CIRCLE('',#11061,7.99999999999999);
#3517=CIRCLE('',#11062,8.);
#3518=CIRCLE('',#11064,7.5);
#3519=CIRCLE('',#11070,1.);
#3520=CIRCLE('',#11071,1.);
#3521=CIRCLE('',#11073,1.);
#3522=CIRCLE('',#11082,7.45);
#3523=CIRCLE('',#11083,7.45);
#3524=CIRCLE('',#11084,6.95000000000004);
#3525=CIRCLE('',#11086,7.5);
#3526=CIRCLE('',#11087,7.5);
#3527=CIRCLE('',#11089,15.);
#3528=CIRCLE('',#11090,15.);
#3529=CIRCLE('',#11092,7.45);
#3530=CIRCLE('',#11094,6.25);
#3531=CIRCLE('',#11095,6.25);
#3532=CIRCLE('',#11096,6.25);
#3533=CIRCLE('',#11097,6.25);
#3534=CIRCLE('',#11112,43.5);
#3535=CIRCLE('',#11113,43.5);
#3536=CIRCLE('',#11115,43.5);
#3537=CIRCLE('',#11116,43.5);
#3538=CIRCLE('',#11118,43.5);
#3539=CIRCLE('',#11119,43.5);
#3540=CIRCLE('',#11121,43.5);
#3541=CIRCLE('',#11122,43.5);
#3542=CIRCLE('',#11124,43.5);
#3543=CIRCLE('',#11125,43.5);
#3544=CIRCLE('',#11127,43.5);
#3545=CIRCLE('',#11128,43.5);
#3546=CIRCLE('',#11130,43.5);
#3547=CIRCLE('',#11131,43.5);
#3548=CIRCLE('',#11133,43.5);
#3549=CIRCLE('',#11134,43.5);
#3550=CIRCLE('',#11136,43.5);
#3551=CIRCLE('',#11137,43.5);
#3552=CIRCLE('',#11139,43.5);
#3553=CIRCLE('',#11140,43.5);
#3554=CIRCLE('',#11142,43.5);
#3555=CIRCLE('',#11143,43.5);
#3556=CIRCLE('',#11145,43.5);
#3557=CIRCLE('',#11146,43.5);
#3558=CIRCLE('',#11148,43.5);
#3559=CIRCLE('',#11149,43.5);
#3560=CIRCLE('',#11151,43.5);
#3561=CIRCLE('',#11152,43.5);
#3562=CIRCLE('',#11154,43.5);
#3563=CIRCLE('',#11155,43.5);
#3564=CIRCLE('',#11157,43.5);
#3565=CIRCLE('',#11158,43.5);
#3566=CIRCLE('',#11160,43.5);
#3567=CIRCLE('',#11161,43.5);
#3568=CIRCLE('',#11163,43.5);
#3569=CIRCLE('',#11164,43.5);
#3570=CIRCLE('',#11166,43.5);
#3571=CIRCLE('',#11167,43.5);
#3572=CIRCLE('',#11169,43.5);
#3573=CIRCLE('',#11170,43.5);
#3574=CIRCLE('',#11172,43.5);
#3575=CIRCLE('',#11173,43.5);
#3576=CIRCLE('',#11175,43.5);
#3577=CIRCLE('',#11176,43.5);
#3578=CIRCLE('',#11178,43.5);
#3579=CIRCLE('',#11179,43.5);
#3580=CIRCLE('',#11181,43.5);
#3581=CIRCLE('',#11182,43.5);
#3582=CIRCLE('',#11184,43.5);
#3583=CIRCLE('',#11185,43.5);
#3584=CIRCLE('',#11187,43.5);
#3585=CIRCLE('',#11188,43.5);
#3586=CIRCLE('',#11190,43.5);
#3587=CIRCLE('',#11191,43.5);
#3588=CIRCLE('',#11193,43.5);
#3589=CIRCLE('',#11194,43.5);
#3590=CIRCLE('',#11196,43.5);
#3591=CIRCLE('',#11197,43.5);
#3592=CIRCLE('',#11199,43.5);
#3593=CIRCLE('',#11200,43.5);
#3594=CIRCLE('',#11202,43.5);
#3595=CIRCLE('',#11203,43.5);
#3596=CIRCLE('',#11205,43.5);
#3597=CIRCLE('',#11206,43.5);
#3598=CIRCLE('',#11208,43.5);
#3599=CIRCLE('',#11209,43.5);
#3600=CIRCLE('',#11211,43.5);
#3601=CIRCLE('',#11212,43.5);
#3602=CIRCLE('',#11214,43.5);
#3603=CIRCLE('',#11215,43.5);
#3604=CIRCLE('',#11217,43.5);
#3605=CIRCLE('',#11218,43.5);
#3606=CIRCLE('',#11220,43.5);
#3607=CIRCLE('',#11221,43.5);
#3608=CIRCLE('',#11223,43.5);
#3609=CIRCLE('',#11224,43.5);
#3610=CIRCLE('',#11226,43.5);
#3611=CIRCLE('',#11227,43.5);
#3612=CIRCLE('',#11229,43.5);
#3613=CIRCLE('',#11230,43.5);
#3614=CIRCLE('',#11232,43.5);
#3615=CIRCLE('',#11233,43.5);
#3616=CIRCLE('',#11235,43.5);
#3617=CIRCLE('',#11236,43.5);
#3618=CIRCLE('',#11238,43.5);
#3619=CIRCLE('',#11239,43.5);
#3620=CIRCLE('',#11241,43.5);
#3621=CIRCLE('',#11242,43.5);
#3622=CIRCLE('',#11244,43.5);
#3623=CIRCLE('',#11245,43.5);
#3624=CIRCLE('',#11246,43.5);
#3625=CIRCLE('',#11247,43.5);
#3626=CIRCLE('',#11248,43.5);
#3627=CIRCLE('',#11249,43.5);
#3628=CIRCLE('',#11250,43.5);
#3629=CIRCLE('',#11251,43.5);
#3630=CIRCLE('',#11252,43.5);
#3631=CIRCLE('',#11253,43.5);
#3632=CIRCLE('',#11254,43.5);
#3633=CIRCLE('',#11255,43.5);
#3634=CIRCLE('',#11256,43.5);
#3635=CIRCLE('',#11257,43.5);
#3636=CIRCLE('',#11258,43.5);
#3637=CIRCLE('',#11259,43.5);
#3638=CIRCLE('',#11260,43.5);
#3639=CIRCLE('',#11261,43.5);
#3640=CIRCLE('',#11262,43.5);
#3641=CIRCLE('',#11263,43.5);
#3642=CIRCLE('',#11264,43.5);
#3643=CIRCLE('',#11265,43.5);
#3644=CIRCLE('',#11266,41.5);
#3645=CIRCLE('',#11267,43.5);
#3646=CIRCLE('',#11268,43.5);
#3647=CIRCLE('',#11269,43.5);
#3648=CIRCLE('',#11270,43.5);
#3649=CIRCLE('',#11271,43.5);
#3650=CIRCLE('',#11272,43.5);
#3651=CIRCLE('',#11273,43.5);
#3652=CIRCLE('',#11274,43.5);
#3653=CIRCLE('',#11275,43.5);
#3654=CIRCLE('',#11276,43.5);
#3655=CIRCLE('',#11277,43.5);
#3656=CIRCLE('',#11278,43.5);
#3657=CIRCLE('',#11279,43.5);
#3658=CIRCLE('',#11280,43.5);
#3659=CIRCLE('',#11281,43.5);
#3660=CIRCLE('',#11282,43.5);
#3661=CIRCLE('',#11283,43.5);
#3662=CIRCLE('',#11284,43.5);
#3663=CIRCLE('',#11285,43.5);
#3664=CIRCLE('',#11286,43.5);
#3665=CIRCLE('',#11287,43.5);
#3666=CIRCLE('',#11288,43.5);
#3667=CIRCLE('',#11290,15.);
#3668=CIRCLE('',#11291,15.);
#3669=CIRCLE('',#11293,43.5);
#3670=CIRCLE('',#11294,43.5);
#3671=CIRCLE('',#11295,43.5);
#3672=CIRCLE('',#11296,43.5);
#3673=CIRCLE('',#11297,43.5);
#3674=CIRCLE('',#11298,43.5);
#3675=CIRCLE('',#11299,43.5);
#3676=CIRCLE('',#11300,43.5);
#3677=CIRCLE('',#11301,43.5);
#3678=CIRCLE('',#11302,43.5);
#3679=CIRCLE('',#11303,43.5);
#3680=CIRCLE('',#11304,43.5);
#3681=CIRCLE('',#11305,43.5);
#3682=CIRCLE('',#11306,43.5);
#3683=CIRCLE('',#11307,43.5);
#3684=CIRCLE('',#11308,43.5);
#3685=CIRCLE('',#11309,43.5);
#3686=CIRCLE('',#11310,43.5);
#3687=CIRCLE('',#11311,43.5);
#3688=CIRCLE('',#11312,43.5);
#3689=CIRCLE('',#11313,43.5);
#3690=CIRCLE('',#11314,43.5);
#3691=CIRCLE('',#11315,41.5);
#3692=CIRCLE('',#11316,43.5);
#3693=CIRCLE('',#11317,43.5);
#3694=CIRCLE('',#11318,43.5);
#3695=CIRCLE('',#11319,43.5);
#3696=CIRCLE('',#11320,43.5);
#3697=CIRCLE('',#11321,43.5);
#3698=CIRCLE('',#11322,43.5);
#3699=CIRCLE('',#11323,43.5);
#3700=CIRCLE('',#11324,43.5);
#3701=CIRCLE('',#11325,43.5);
#3702=CIRCLE('',#11326,43.5);
#3703=CIRCLE('',#11327,43.5);
#3704=CIRCLE('',#11328,43.5);
#3705=CIRCLE('',#11329,43.5);
#3706=CIRCLE('',#11330,43.5);
#3707=CIRCLE('',#11331,43.5);
#3708=CIRCLE('',#11332,43.5);
#3709=CIRCLE('',#11333,43.5);
#3710=CIRCLE('',#11334,43.5);
#3711=CIRCLE('',#11335,43.5);
#3712=CIRCLE('',#11336,43.5);
#3713=CIRCLE('',#11337,43.5);
#3714=CIRCLE('',#11431,1.8);
#3715=CIRCLE('',#11432,1.8);
#3716=CIRCLE('',#11433,18.);
#3717=CIRCLE('',#11434,18.);
#3718=CIRCLE('',#11435,18.);
#3719=CIRCLE('',#11436,18.);
#3720=CIRCLE('',#11437,1.8);
#3721=CIRCLE('',#11438,1.8);
#3722=CIRCLE('',#11439,18.);
#3723=CIRCLE('',#11440,18.);
#3724=CIRCLE('',#11441,1.8);
#3725=CIRCLE('',#11442,1.8);
#3726=CIRCLE('',#11443,18.);
#3727=CIRCLE('',#11444,18.);
#3728=CIRCLE('',#11445,1.8);
#3729=CIRCLE('',#11446,1.8);
#3730=CIRCLE('',#11447,18.);
#3731=CIRCLE('',#11448,18.);
#3732=CIRCLE('',#11449,1.8);
#3733=CIRCLE('',#11450,1.8);
#3734=CIRCLE('',#11451,18.);
#3735=CIRCLE('',#11452,18.);
#3736=CIRCLE('',#11453,1.8);
#3737=CIRCLE('',#11454,1.8);
#3738=CIRCLE('',#11455,18.);
#3739=CIRCLE('',#11456,18.);
#3740=CIRCLE('',#11457,1.8);
#3741=CIRCLE('',#11458,1.8);
#3742=CIRCLE('',#11459,18.);
#3743=CIRCLE('',#11460,18.);
#3744=CIRCLE('',#11461,1.8);
#3745=CIRCLE('',#11462,1.8);
#3746=CIRCLE('',#11463,18.);
#3747=CIRCLE('',#11464,18.);
#3748=CIRCLE('',#11465,1.8);
#3749=CIRCLE('',#11466,1.8);
#3750=CIRCLE('',#11467,18.);
#3751=CIRCLE('',#11468,18.);
#3752=CIRCLE('',#11469,1.8);
#3753=CIRCLE('',#11470,1.8);
#3754=CIRCLE('',#11471,18.);
#3755=CIRCLE('',#11472,18.);
#3756=CIRCLE('',#11473,1.8);
#3757=CIRCLE('',#11474,1.8);
#3758=CIRCLE('',#11475,18.);
#3759=CIRCLE('',#11476,18.);
#3760=CIRCLE('',#11477,1.8);
#3761=CIRCLE('',#11478,1.8);
#3762=CIRCLE('',#11479,18.);
#3763=CIRCLE('',#11480,18.);
#3764=CIRCLE('',#11481,1.8);
#3765=CIRCLE('',#11482,1.8);
#3766=CIRCLE('',#11483,18.);
#3767=CIRCLE('',#11484,18.);
#3768=CIRCLE('',#11485,1.8);
#3769=CIRCLE('',#11486,1.8);
#3770=CIRCLE('',#11487,18.);
#3771=CIRCLE('',#11488,18.);
#3772=CIRCLE('',#11489,1.8);
#3773=CIRCLE('',#11490,1.8);
#3774=CIRCLE('',#11491,18.);
#3775=CIRCLE('',#11492,17.9999999999999);
#3776=CIRCLE('',#11493,1.80000000000001);
#3777=CIRCLE('',#11494,1.80000000000001);
#3778=CIRCLE('',#11495,18.);
#3779=CIRCLE('',#11496,18.);
#3780=CIRCLE('',#11497,1.8);
#3781=CIRCLE('',#11498,1.8);
#3782=CIRCLE('',#11499,18.);
#3783=CIRCLE('',#11500,18.);
#3784=CIRCLE('',#11501,1.8);
#3785=CIRCLE('',#11502,1.8);
#3786=CIRCLE('',#11503,18.);
#3787=CIRCLE('',#11504,18.);
#3788=CIRCLE('',#11505,1.8);
#3789=CIRCLE('',#11506,1.8);
#3790=CIRCLE('',#11507,18.);
#3791=CIRCLE('',#11508,18.);
#3792=CIRCLE('',#11509,1.8);
#3793=CIRCLE('',#11510,1.8);
#3794=CIRCLE('',#11511,18.);
#3795=CIRCLE('',#11512,18.);
#3796=CIRCLE('',#11513,1.8);
#3797=CIRCLE('',#11514,1.8);
#3798=CIRCLE('',#11515,18.);
#3799=CIRCLE('',#11516,18.);
#3800=CIRCLE('',#11517,1.8);
#3801=CIRCLE('',#11518,1.8);
#3802=CIRCLE('',#11519,18.);
#3803=CIRCLE('',#11520,18.);
#3804=CIRCLE('',#11521,1.8);
#3805=CIRCLE('',#11522,1.8);
#3806=CIRCLE('',#11523,18.);
#3807=CIRCLE('',#11524,18.);
#3808=CIRCLE('',#11525,1.8);
#3809=CIRCLE('',#11526,1.8);
#3810=CIRCLE('',#11527,18.);
#3811=CIRCLE('',#11528,18.);
#3812=CIRCLE('',#11529,1.8);
#3813=CIRCLE('',#11530,1.8);
#3814=CIRCLE('',#11531,18.);
#3815=CIRCLE('',#11532,18.);
#3816=CIRCLE('',#11533,1.8);
#3817=CIRCLE('',#11534,1.8);
#3818=CIRCLE('',#11535,18.);
#3819=CIRCLE('',#11536,18.);
#3820=CIRCLE('',#11537,1.8);
#3821=CIRCLE('',#11538,1.8);
#3822=CIRCLE('',#11539,18.);
#3823=CIRCLE('',#11540,18.);
#3824=CIRCLE('',#11541,1.8);
#3825=CIRCLE('',#11542,1.8);
#3826=CIRCLE('',#11543,18.);
#3827=CIRCLE('',#11544,18.);
#3828=CIRCLE('',#11545,1.8);
#3829=CIRCLE('',#11546,1.8);
#3830=CIRCLE('',#11547,18.);
#3831=CIRCLE('',#11548,18.);
#3832=CIRCLE('',#11549,1.8);
#3833=CIRCLE('',#11550,1.8);
#3834=CIRCLE('',#11551,18.);
#3835=CIRCLE('',#11552,18.);
#3836=CIRCLE('',#11553,1.8);
#3837=CIRCLE('',#11554,1.8);
#3838=CIRCLE('',#11555,18.);
#3839=CIRCLE('',#11556,18.);
#3840=CIRCLE('',#11557,1.8);
#3841=CIRCLE('',#11558,1.8);
#3842=CIRCLE('',#11559,18.);
#3843=CIRCLE('',#11560,18.);
#3844=CIRCLE('',#11561,1.8);
#3845=CIRCLE('',#11562,1.8);
#3846=CIRCLE('',#11563,18.);
#3847=CIRCLE('',#11564,18.);
#3848=CIRCLE('',#11565,1.8);
#3849=CIRCLE('',#11566,1.8);
#3850=CIRCLE('',#11567,18.);
#3851=CIRCLE('',#11568,18.);
#3852=CIRCLE('',#11569,1.8);
#3853=CIRCLE('',#11570,1.8);
#3854=CIRCLE('',#11571,18.);
#3855=CIRCLE('',#11572,18.);
#3856=CIRCLE('',#11573,1.8);
#3857=CIRCLE('',#11574,1.8);
#3858=CIRCLE('',#11575,18.);
#3859=CIRCLE('',#11576,18.);
#3860=CIRCLE('',#11577,1.8);
#3861=CIRCLE('',#11578,1.8);
#3862=CIRCLE('',#11579,17.9999999999999);
#3863=CIRCLE('',#11580,18.);
#3864=CIRCLE('',#11581,1.8);
#3865=CIRCLE('',#11582,1.8);
#3866=CIRCLE('',#11583,18.);
#3867=CIRCLE('',#11584,18.);
#3868=CIRCLE('',#11585,1.8);
#3869=CIRCLE('',#11586,1.8);
#3870=CIRCLE('',#11587,18.);
#3871=CIRCLE('',#11588,18.);
#3872=CIRCLE('',#11589,1.8);
#3873=CIRCLE('',#11590,1.8);
#3874=CIRCLE('',#11591,18.);
#3875=CIRCLE('',#11592,18.);
#3876=CIRCLE('',#11593,1.8);
#3877=CIRCLE('',#11594,1.8);
#3878=CIRCLE('',#11595,18.);
#3879=CIRCLE('',#11596,18.);
#3880=CIRCLE('',#11597,1.8);
#3881=CIRCLE('',#11598,1.8);
#3882=CIRCLE('',#11599,18.);
#3883=CIRCLE('',#11600,18.);
#3884=CIRCLE('',#11601,1.8);
#3885=CIRCLE('',#11602,1.8);
#3886=CIRCLE('',#11603,18.);
#3887=CIRCLE('',#11604,18.);
#3888=CIRCLE('',#11605,1.8);
#3889=CIRCLE('',#11606,1.8);
#3890=CIRCLE('',#11609,4.);
#3891=CIRCLE('',#11610,4.);
#3892=CIRCLE('',#11612,4.);
#3893=CIRCLE('',#11613,4.);
#3894=CIRCLE('',#11615,2.5);
#3895=CIRCLE('',#11616,2.5);
#3896=CIRCLE('',#11618,2.5);
#3897=CIRCLE('',#11619,2.5);
#3898=CIRCLE('',#11621,2.5);
#3899=CIRCLE('',#11622,2.5);
#3900=CIRCLE('',#11624,2.5);
#3901=CIRCLE('',#11625,2.5);
#3902=CIRCLE('',#11627,3.);
#3903=CIRCLE('',#11628,3.);
#3904=CIRCLE('',#11630,2.99999999999999);
#3905=CIRCLE('',#11631,2.99999999999999);
#3906=CIRCLE('',#11633,3.);
#3907=CIRCLE('',#11634,3.);
#3908=CIRCLE('',#11636,3.);
#3909=CIRCLE('',#11637,3.);
#3910=CIRCLE('',#11639,3.);
#3911=CIRCLE('',#11640,3.);
#3912=CIRCLE('',#11642,3.);
#3913=CIRCLE('',#11643,3.);
#3914=CIRCLE('',#11645,17.5);
#3915=CIRCLE('',#11646,17.5);
#3916=CIRCLE('',#11653,2.5);
#3917=CIRCLE('',#11654,17.5);
#3918=CIRCLE('',#11655,2.50000000000001);
#3919=CIRCLE('',#11658,2.50000000000001);
#3920=CIRCLE('',#11659,17.5);
#3921=CIRCLE('',#11660,2.5);
#3922=CIRCLE('',#11664,2.5);
#3923=CIRCLE('',#11665,2.50000000000001);
#3924=CIRCLE('',#11666,17.5);
#3925=CIRCLE('',#11669,2.5);
#3926=CIRCLE('',#11670,17.5);
#3927=CIRCLE('',#11671,2.50000000000001);
#3928=CIRCLE('',#11697,0.5);
#3929=CIRCLE('',#11698,0.5);
#3930=CIRCLE('',#11700,0.5);
#3931=CIRCLE('',#11701,0.5);
#3932=CIRCLE('',#11703,0.5);
#3933=CIRCLE('',#11704,0.5);
#3934=CIRCLE('',#11706,0.5);
#3935=CIRCLE('',#11708,0.5);
#3936=CIRCLE('',#11710,0.5);
#3937=CIRCLE('',#11711,0.5);
#3938=CIRCLE('',#11713,0.5);
#3939=CIRCLE('',#11715,0.5);
#3940=CIRCLE('',#11717,0.5);
#3941=CIRCLE('',#11718,0.5);
#3942=CIRCLE('',#11720,0.5);
#3943=CIRCLE('',#11722,0.5);
#3944=CIRCLE('',#11724,0.5);
#3945=CIRCLE('',#11726,0.5);
#3946=CIRCLE('',#11728,0.5);
#3947=CIRCLE('',#11730,0.5);
#3948=CIRCLE('',#11732,0.5);
#3949=CIRCLE('',#11734,0.5);
#3950=CIRCLE('',#11736,0.5);
#3951=CIRCLE('',#11738,0.5);
#3952=CIRCLE('',#11742,3.);
#3953=CIRCLE('',#11743,3.);
#3954=CIRCLE('',#11745,3.);
#3955=CIRCLE('',#11746,3.);
#3956=CIRCLE('',#11748,3.);
#3957=CIRCLE('',#11749,3.);
#3958=CIRCLE('',#11751,3.00000000000001);
#3959=CIRCLE('',#11752,3.00000000000001);
#3960=CIRCLE('',#11754,3.);
#3961=CIRCLE('',#11755,3.);
#3962=CIRCLE('',#11757,3.);
#3963=CIRCLE('',#11758,3.);
#3964=CIRCLE('',#11760,7.6);
#3965=CIRCLE('',#11761,7.6);
#3966=CIRCLE('',#11763,30.);
#3967=CIRCLE('',#11764,30.);
#3968=CIRCLE('',#11769,2.5);
#3969=CIRCLE('',#11770,2.5);
#3970=CIRCLE('',#11772,2.5);
#3971=CIRCLE('',#11773,2.5);
#3972=CIRCLE('',#11775,2.5);
#3973=CIRCLE('',#11776,2.5);
#3974=CIRCLE('',#11778,2.5);
#3975=CIRCLE('',#11779,2.5);
#3976=CIRCLE('',#11781,2.5);
#3977=CIRCLE('',#11782,2.5);
#3978=CIRCLE('',#11784,2.5);
#3979=CIRCLE('',#11785,2.5);
#3980=CIRCLE('',#11787,7.6);
#3981=CIRCLE('',#11788,7.6);
#3982=CIRCLE('',#11790,27.5);
#3983=CIRCLE('',#11791,27.5);
#3984=CIRCLE('',#11796,3.97500000000001);
#3985=CIRCLE('',#11797,3.47500000000001);
#3986=CIRCLE('',#11799,3.);
#3987=CIRCLE('',#11800,2.);
#3988=CIRCLE('',#11801,5.00000000000001);
#3989=CIRCLE('',#11802,5.00000000000001);
#3990=CIRCLE('',#11804,5.00000000000001);
#3991=CIRCLE('',#11806,3.97500000000001);
#3992=CIRCLE('',#11812,2.5);
#3993=CIRCLE('',#11813,2.5);
#3994=CIRCLE('',#11842,7.5);
#3995=CIRCLE('',#11843,7.5);
#3996=CIRCLE('',#11845,17.5);
#3997=CIRCLE('',#11846,17.5);
#3998=VERTEX_POINT('',#14046);
#3999=VERTEX_POINT('',#14048);
#4000=VERTEX_POINT('',#14052);
#4001=VERTEX_POINT('',#14054);
#4002=VERTEX_POINT('',#14058);
#4003=VERTEX_POINT('',#14060);
#4004=VERTEX_POINT('',#14064);
#4005=VERTEX_POINT('',#14066);
#4006=VERTEX_POINT('',#14070);
#4007=VERTEX_POINT('',#14072);
#4008=VERTEX_POINT('',#14076);
#4009=VERTEX_POINT('',#14078);
#4010=VERTEX_POINT('',#14082);
#4011=VERTEX_POINT('',#14084);
#4012=VERTEX_POINT('',#14088);
#4013=VERTEX_POINT('',#14090);
#4014=VERTEX_POINT('',#14094);
#4015=VERTEX_POINT('',#14096);
#4016=VERTEX_POINT('',#14100);
#4017=VERTEX_POINT('',#14102);
#4018=VERTEX_POINT('',#14106);
#4019=VERTEX_POINT('',#14108);
#4020=VERTEX_POINT('',#14112);
#4021=VERTEX_POINT('',#14113);
#4022=VERTEX_POINT('',#14115);
#4023=VERTEX_POINT('',#14117);
#4024=VERTEX_POINT('',#14119);
#4025=VERTEX_POINT('',#14121);
#4026=VERTEX_POINT('',#14123);
#4027=VERTEX_POINT('',#14125);
#4028=VERTEX_POINT('',#14129);
#4029=VERTEX_POINT('',#14130);
#4030=VERTEX_POINT('',#14132);
#4031=VERTEX_POINT('',#14134);
#4032=VERTEX_POINT('',#14138);
#4033=VERTEX_POINT('',#14139);
#4034=VERTEX_POINT('',#14141);
#4035=VERTEX_POINT('',#14143);
#4036=VERTEX_POINT('',#14147);
#4037=VERTEX_POINT('',#14148);
#4038=VERTEX_POINT('',#14150);
#4039=VERTEX_POINT('',#14152);
#4040=VERTEX_POINT('',#14156);
#4041=VERTEX_POINT('',#14157);
#4042=VERTEX_POINT('',#14159);
#4043=VERTEX_POINT('',#14161);
#4044=VERTEX_POINT('',#14165);
#4045=VERTEX_POINT('',#14167);
#4046=VERTEX_POINT('',#14169);
#4047=VERTEX_POINT('',#14171);
#4048=VERTEX_POINT('',#14177);
#4049=VERTEX_POINT('',#14179);
#4050=VERTEX_POINT('',#14181);
#4051=VERTEX_POINT('',#14183);
#4052=VERTEX_POINT('',#14185);
#4053=VERTEX_POINT('',#14187);
#4054=VERTEX_POINT('',#14191);
#4055=VERTEX_POINT('',#14193);
#4056=VERTEX_POINT('',#14207);
#4057=VERTEX_POINT('',#14209);
#4058=VERTEX_POINT('',#14213);
#4059=VERTEX_POINT('',#14218);
#4060=VERTEX_POINT('',#14227);
#4061=VERTEX_POINT('',#14228);
#4062=VERTEX_POINT('',#14230);
#4063=VERTEX_POINT('',#14232);
#4064=VERTEX_POINT('',#14251);
#4065=VERTEX_POINT('',#14252);
#4066=VERTEX_POINT('',#14254);
#4067=VERTEX_POINT('',#14275);
#4068=VERTEX_POINT('',#14277);
#4069=VERTEX_POINT('',#14298);
#4070=VERTEX_POINT('',#14338);
#4071=VERTEX_POINT('',#14339);
#4072=VERTEX_POINT('',#14416);
#4073=VERTEX_POINT('',#14417);
#4074=VERTEX_POINT('',#14494);
#4075=VERTEX_POINT('',#14495);
#4076=VERTEX_POINT('',#14533);
#4077=VERTEX_POINT('',#14575);
#4078=VERTEX_POINT('',#14576);
#4079=VERTEX_POINT('',#14578);
#4080=VERTEX_POINT('',#14656);
#4081=VERTEX_POINT('',#14657);
#4082=VERTEX_POINT('',#14732);
#4083=VERTEX_POINT('',#14734);
#4084=VERTEX_POINT('',#14736);
#4085=VERTEX_POINT('',#14773);
#4086=VERTEX_POINT('',#14775);
#4087=VERTEX_POINT('',#14796);
#4088=VERTEX_POINT('',#14819);
#4089=VERTEX_POINT('',#14820);
#4090=VERTEX_POINT('',#14823);
#4091=VERTEX_POINT('',#14827);
#4092=VERTEX_POINT('',#14828);
#4093=VERTEX_POINT('',#14830);
#4094=VERTEX_POINT('',#14832);
#4095=VERTEX_POINT('',#14834);
#4096=VERTEX_POINT('',#14837);
#4097=VERTEX_POINT('',#14841);
#4098=VERTEX_POINT('',#14843);
#4099=VERTEX_POINT('',#14847);
#4100=VERTEX_POINT('',#14929);
#4101=VERTEX_POINT('',#14931);
#4102=VERTEX_POINT('',#15160);
#4103=VERTEX_POINT('',#15727);
#4104=VERTEX_POINT('',#16070);
#4105=VERTEX_POINT('',#16072);
#4106=VERTEX_POINT('',#17206);
#4107=VERTEX_POINT('',#17208);
#4108=VERTEX_POINT('',#17212);
#4109=VERTEX_POINT('',#17216);
#4110=VERTEX_POINT('',#17225);
#4111=VERTEX_POINT('',#17226);
#4112=VERTEX_POINT('',#17229);
#4113=VERTEX_POINT('',#17233);
#4114=VERTEX_POINT('',#17235);
#4115=VERTEX_POINT('',#17239);
#4116=VERTEX_POINT('',#17240);
#4117=VERTEX_POINT('',#17242);
#4118=VERTEX_POINT('',#17244);
#4119=VERTEX_POINT('',#17248);
#4120=VERTEX_POINT('',#17252);
#4121=VERTEX_POINT('',#17254);
#4122=VERTEX_POINT('',#17256);
#4123=VERTEX_POINT('',#17258);
#4124=VERTEX_POINT('',#17260);
#4125=VERTEX_POINT('',#17262);
#4126=VERTEX_POINT('',#17266);
#4127=VERTEX_POINT('',#17267);
#4128=VERTEX_POINT('',#17273);
#4129=VERTEX_POINT('',#17275);
#4130=VERTEX_POINT('',#17279);
#4131=VERTEX_POINT('',#17281);
#4132=VERTEX_POINT('',#17291);
#4133=VERTEX_POINT('',#17293);
#4134=VERTEX_POINT('',#17303);
#4135=VERTEX_POINT('',#17304);
#4136=VERTEX_POINT('',#17311);
#4137=VERTEX_POINT('',#17318);
#4138=VERTEX_POINT('',#17320);
#4139=VERTEX_POINT('',#17335);
#4140=VERTEX_POINT('',#17344);
#4141=VERTEX_POINT('',#17345);
#4142=VERTEX_POINT('',#17352);
#4143=VERTEX_POINT('',#17359);
#4144=VERTEX_POINT('',#17361);
#4145=VERTEX_POINT('',#17376);
#4146=VERTEX_POINT('',#17385);
#4147=VERTEX_POINT('',#17386);
#4148=VERTEX_POINT('',#17393);
#4149=VERTEX_POINT('',#17406);
#4150=VERTEX_POINT('',#17408);
#4151=VERTEX_POINT('',#17423);
#4152=VERTEX_POINT('',#17432);
#4153=VERTEX_POINT('',#17433);
#4154=VERTEX_POINT('',#17440);
#4155=VERTEX_POINT('',#17447);
#4156=VERTEX_POINT('',#17449);
#4157=VERTEX_POINT('',#17458);
#4158=VERTEX_POINT('',#17467);
#4159=VERTEX_POINT('',#17468);
#4160=VERTEX_POINT('',#17475);
#4161=VERTEX_POINT('',#17482);
#4162=VERTEX_POINT('',#17484);
#4163=VERTEX_POINT('',#17499);
#4164=VERTEX_POINT('',#17508);
#4165=VERTEX_POINT('',#17509);
#4166=VERTEX_POINT('',#17516);
#4167=VERTEX_POINT('',#17523);
#4168=VERTEX_POINT('',#17525);
#4169=VERTEX_POINT('',#17540);
#4170=VERTEX_POINT('',#17549);
#4171=VERTEX_POINT('',#17550);
#4172=VERTEX_POINT('',#17557);
#4173=VERTEX_POINT('',#17564);
#4174=VERTEX_POINT('',#17566);
#4175=VERTEX_POINT('',#17581);
#4176=VERTEX_POINT('',#17590);
#4177=VERTEX_POINT('',#17591);
#4178=VERTEX_POINT('',#17598);
#4179=VERTEX_POINT('',#17605);
#4180=VERTEX_POINT('',#17607);
#4181=VERTEX_POINT('',#17622);
#4182=VERTEX_POINT('',#17631);
#4183=VERTEX_POINT('',#17632);
#4184=VERTEX_POINT('',#17639);
#4185=VERTEX_POINT('',#17646);
#4186=VERTEX_POINT('',#17648);
#4187=VERTEX_POINT('',#17663);
#4188=VERTEX_POINT('',#17672);
#4189=VERTEX_POINT('',#17673);
#4190=VERTEX_POINT('',#17680);
#4191=VERTEX_POINT('',#17687);
#4192=VERTEX_POINT('',#17689);
#4193=VERTEX_POINT('',#17704);
#4194=VERTEX_POINT('',#17713);
#4195=VERTEX_POINT('',#17714);
#4196=VERTEX_POINT('',#17721);
#4197=VERTEX_POINT('',#17728);
#4198=VERTEX_POINT('',#17730);
#4199=VERTEX_POINT('',#17745);
#4200=VERTEX_POINT('',#17754);
#4201=VERTEX_POINT('',#17755);
#4202=VERTEX_POINT('',#17762);
#4203=VERTEX_POINT('',#17775);
#4204=VERTEX_POINT('',#17777);
#4205=VERTEX_POINT('',#17792);
#4206=VERTEX_POINT('',#17801);
#4207=VERTEX_POINT('',#17802);
#4208=VERTEX_POINT('',#17809);
#4209=VERTEX_POINT('',#17816);
#4210=VERTEX_POINT('',#17818);
#4211=VERTEX_POINT('',#17827);
#4212=VERTEX_POINT('',#17836);
#4213=VERTEX_POINT('',#17837);
#4214=VERTEX_POINT('',#17844);
#4215=VERTEX_POINT('',#17851);
#4216=VERTEX_POINT('',#17853);
#4217=VERTEX_POINT('',#17868);
#4218=VERTEX_POINT('',#17877);
#4219=VERTEX_POINT('',#17878);
#4220=VERTEX_POINT('',#17885);
#4221=VERTEX_POINT('',#17892);
#4222=VERTEX_POINT('',#17894);
#4223=VERTEX_POINT('',#17909);
#4224=VERTEX_POINT('',#17918);
#4225=VERTEX_POINT('',#17919);
#4226=VERTEX_POINT('',#17926);
#4227=VERTEX_POINT('',#17933);
#4228=VERTEX_POINT('',#17935);
#4229=VERTEX_POINT('',#17950);
#4230=VERTEX_POINT('',#17959);
#4231=VERTEX_POINT('',#17960);
#4232=VERTEX_POINT('',#17967);
#4233=VERTEX_POINT('',#17974);
#4234=VERTEX_POINT('',#17976);
#4235=VERTEX_POINT('',#17991);
#4236=VERTEX_POINT('',#18000);
#4237=VERTEX_POINT('',#18001);
#4238=VERTEX_POINT('',#18008);
#4239=VERTEX_POINT('',#18015);
#4240=VERTEX_POINT('',#18017);
#4241=VERTEX_POINT('',#18032);
#4242=VERTEX_POINT('',#18041);
#4243=VERTEX_POINT('',#18042);
#4244=VERTEX_POINT('',#18049);
#4245=VERTEX_POINT('',#18056);
#4246=VERTEX_POINT('',#18058);
#4247=VERTEX_POINT('',#18073);
#4248=VERTEX_POINT('',#18082);
#4249=VERTEX_POINT('',#18083);
#4250=VERTEX_POINT('',#18090);
#4251=VERTEX_POINT('',#18097);
#4252=VERTEX_POINT('',#18099);
#4253=VERTEX_POINT('',#18114);
#4254=VERTEX_POINT('',#18123);
#4255=VERTEX_POINT('',#18124);
#4256=VERTEX_POINT('',#18131);
#4257=VERTEX_POINT('',#18138);
#4258=VERTEX_POINT('',#18140);
#4259=VERTEX_POINT('',#18155);
#4260=VERTEX_POINT('',#18164);
#4261=VERTEX_POINT('',#18165);
#4262=VERTEX_POINT('',#18172);
#4263=VERTEX_POINT('',#18179);
#4264=VERTEX_POINT('',#18181);
#4265=VERTEX_POINT('',#18196);
#4266=VERTEX_POINT('',#18205);
#4267=VERTEX_POINT('',#18206);
#4268=VERTEX_POINT('',#18213);
#4269=VERTEX_POINT('',#18220);
#4270=VERTEX_POINT('',#18222);
#4271=VERTEX_POINT('',#18237);
#4272=VERTEX_POINT('',#18246);
#4273=VERTEX_POINT('',#18247);
#4274=VERTEX_POINT('',#18254);
#4275=VERTEX_POINT('',#18261);
#4276=VERTEX_POINT('',#18263);
#4277=VERTEX_POINT('',#18278);
#4278=VERTEX_POINT('',#18287);
#4279=VERTEX_POINT('',#18288);
#4280=VERTEX_POINT('',#18295);
#4281=VERTEX_POINT('',#18308);
#4282=VERTEX_POINT('',#18310);
#4283=VERTEX_POINT('',#18325);
#4284=VERTEX_POINT('',#18334);
#4285=VERTEX_POINT('',#18335);
#4286=VERTEX_POINT('',#18342);
#4287=VERTEX_POINT('',#18355);
#4288=VERTEX_POINT('',#18357);
#4289=VERTEX_POINT('',#18366);
#4290=VERTEX_POINT('',#18375);
#4291=VERTEX_POINT('',#18376);
#4292=VERTEX_POINT('',#18383);
#4293=VERTEX_POINT('',#18390);
#4294=VERTEX_POINT('',#18392);
#4295=VERTEX_POINT('',#18401);
#4296=VERTEX_POINT('',#18410);
#4297=VERTEX_POINT('',#18411);
#4298=VERTEX_POINT('',#18418);
#4299=VERTEX_POINT('',#18425);
#4300=VERTEX_POINT('',#18427);
#4301=VERTEX_POINT('',#18442);
#4302=VERTEX_POINT('',#18451);
#4303=VERTEX_POINT('',#18452);
#4304=VERTEX_POINT('',#18459);
#4305=VERTEX_POINT('',#18466);
#4306=VERTEX_POINT('',#18468);
#4307=VERTEX_POINT('',#18483);
#4308=VERTEX_POINT('',#18492);
#4309=VERTEX_POINT('',#18493);
#4310=VERTEX_POINT('',#18500);
#4311=VERTEX_POINT('',#18507);
#4312=VERTEX_POINT('',#18509);
#4313=VERTEX_POINT('',#18524);
#4314=VERTEX_POINT('',#18533);
#4315=VERTEX_POINT('',#18534);
#4316=VERTEX_POINT('',#18541);
#4317=VERTEX_POINT('',#18548);
#4318=VERTEX_POINT('',#18550);
#4319=VERTEX_POINT('',#18565);
#4320=VERTEX_POINT('',#18574);
#4321=VERTEX_POINT('',#18575);
#4322=VERTEX_POINT('',#18582);
#4323=VERTEX_POINT('',#18589);
#4324=VERTEX_POINT('',#18591);
#4325=VERTEX_POINT('',#18606);
#4326=VERTEX_POINT('',#18615);
#4327=VERTEX_POINT('',#18616);
#4328=VERTEX_POINT('',#18623);
#4329=VERTEX_POINT('',#18636);
#4330=VERTEX_POINT('',#18638);
#4331=VERTEX_POINT('',#18653);
#4332=VERTEX_POINT('',#18662);
#4333=VERTEX_POINT('',#18663);
#4334=VERTEX_POINT('',#18670);
#4335=VERTEX_POINT('',#18683);
#4336=VERTEX_POINT('',#18685);
#4337=VERTEX_POINT('',#18694);
#4338=VERTEX_POINT('',#18703);
#4339=VERTEX_POINT('',#18704);
#4340=VERTEX_POINT('',#18711);
#4341=VERTEX_POINT('',#18718);
#4342=VERTEX_POINT('',#18720);
#4343=VERTEX_POINT('',#18729);
#4344=VERTEX_POINT('',#18738);
#4345=VERTEX_POINT('',#18739);
#4346=VERTEX_POINT('',#18746);
#4347=VERTEX_POINT('',#18753);
#4348=VERTEX_POINT('',#18755);
#4349=VERTEX_POINT('',#18770);
#4350=VERTEX_POINT('',#18779);
#4351=VERTEX_POINT('',#18780);
#4352=VERTEX_POINT('',#18787);
#4353=VERTEX_POINT('',#18794);
#4354=VERTEX_POINT('',#18796);
#4355=VERTEX_POINT('',#18811);
#4356=VERTEX_POINT('',#18820);
#4357=VERTEX_POINT('',#18821);
#4358=VERTEX_POINT('',#18828);
#4359=VERTEX_POINT('',#18835);
#4360=VERTEX_POINT('',#18837);
#4361=VERTEX_POINT('',#18852);
#4362=VERTEX_POINT('',#18861);
#4363=VERTEX_POINT('',#18862);
#4364=VERTEX_POINT('',#18869);
#4365=VERTEX_POINT('',#18876);
#4366=VERTEX_POINT('',#18878);
#4367=VERTEX_POINT('',#18893);
#4368=VERTEX_POINT('',#18902);
#4369=VERTEX_POINT('',#18903);
#4370=VERTEX_POINT('',#18910);
#4371=VERTEX_POINT('',#18917);
#4372=VERTEX_POINT('',#18919);
#4373=VERTEX_POINT('',#18934);
#4374=VERTEX_POINT('',#18943);
#4375=VERTEX_POINT('',#18944);
#4376=VERTEX_POINT('',#18951);
#4377=VERTEX_POINT('',#18958);
#4378=VERTEX_POINT('',#18960);
#4379=VERTEX_POINT('',#18975);
#4380=VERTEX_POINT('',#18984);
#4381=VERTEX_POINT('',#18985);
#4382=VERTEX_POINT('',#18992);
#4383=VERTEX_POINT('',#18999);
#4384=VERTEX_POINT('',#19001);
#4385=VERTEX_POINT('',#19016);
#4386=VERTEX_POINT('',#19025);
#4387=VERTEX_POINT('',#19026);
#4388=VERTEX_POINT('',#19033);
#4389=VERTEX_POINT('',#19040);
#4390=VERTEX_POINT('',#19042);
#4391=VERTEX_POINT('',#19051);
#4392=VERTEX_POINT('',#19060);
#4393=VERTEX_POINT('',#19061);
#4394=VERTEX_POINT('',#19068);
#4395=VERTEX_POINT('',#19081);
#4396=VERTEX_POINT('',#19083);
#4397=VERTEX_POINT('',#19098);
#4398=VERTEX_POINT('',#19107);
#4399=VERTEX_POINT('',#19108);
#4400=VERTEX_POINT('',#19121);
#4401=VERTEX_POINT('',#19129);
#4402=VERTEX_POINT('',#19131);
#4403=VERTEX_POINT('',#19139);
#4404=VERTEX_POINT('',#19150);
#4405=VERTEX_POINT('',#19158);
#4406=VERTEX_POINT('',#19160);
#4407=VERTEX_POINT('',#19168);
#4408=VERTEX_POINT('',#19179);
#4409=VERTEX_POINT('',#19187);
#4410=VERTEX_POINT('',#19189);
#4411=VERTEX_POINT('',#19197);
#4412=VERTEX_POINT('',#19208);
#4413=VERTEX_POINT('',#19216);
#4414=VERTEX_POINT('',#19218);
#4415=VERTEX_POINT('',#19226);
#4416=VERTEX_POINT('',#19237);
#4417=VERTEX_POINT('',#19245);
#4418=VERTEX_POINT('',#19247);
#4419=VERTEX_POINT('',#19255);
#4420=VERTEX_POINT('',#19266);
#4421=VERTEX_POINT('',#19274);
#4422=VERTEX_POINT('',#19276);
#4423=VERTEX_POINT('',#19284);
#4424=VERTEX_POINT('',#19295);
#4425=VERTEX_POINT('',#19303);
#4426=VERTEX_POINT('',#19305);
#4427=VERTEX_POINT('',#19313);
#4428=VERTEX_POINT('',#19324);
#4429=VERTEX_POINT('',#19332);
#4430=VERTEX_POINT('',#19334);
#4431=VERTEX_POINT('',#19342);
#4432=VERTEX_POINT('',#19353);
#4433=VERTEX_POINT('',#19361);
#4434=VERTEX_POINT('',#19363);
#4435=VERTEX_POINT('',#19371);
#4436=VERTEX_POINT('',#19382);
#4437=VERTEX_POINT('',#19390);
#4438=VERTEX_POINT('',#19392);
#4439=VERTEX_POINT('',#19400);
#4440=VERTEX_POINT('',#19411);
#4441=VERTEX_POINT('',#19419);
#4442=VERTEX_POINT('',#19421);
#4443=VERTEX_POINT('',#19429);
#4444=VERTEX_POINT('',#19440);
#4445=VERTEX_POINT('',#19448);
#4446=VERTEX_POINT('',#19450);
#4447=VERTEX_POINT('',#19458);
#4448=VERTEX_POINT('',#19469);
#4449=VERTEX_POINT('',#19477);
#4450=VERTEX_POINT('',#19479);
#4451=VERTEX_POINT('',#19487);
#4452=VERTEX_POINT('',#19498);
#4453=VERTEX_POINT('',#19506);
#4454=VERTEX_POINT('',#19508);
#4455=VERTEX_POINT('',#19516);
#4456=VERTEX_POINT('',#19527);
#4457=VERTEX_POINT('',#19535);
#4458=VERTEX_POINT('',#19537);
#4459=VERTEX_POINT('',#19545);
#4460=VERTEX_POINT('',#19556);
#4461=VERTEX_POINT('',#19564);
#4462=VERTEX_POINT('',#19566);
#4463=VERTEX_POINT('',#19574);
#4464=VERTEX_POINT('',#19585);
#4465=VERTEX_POINT('',#19593);
#4466=VERTEX_POINT('',#19595);
#4467=VERTEX_POINT('',#19603);
#4468=VERTEX_POINT('',#19614);
#4469=VERTEX_POINT('',#19622);
#4470=VERTEX_POINT('',#19624);
#4471=VERTEX_POINT('',#19632);
#4472=VERTEX_POINT('',#19643);
#4473=VERTEX_POINT('',#19651);
#4474=VERTEX_POINT('',#19653);
#4475=VERTEX_POINT('',#19661);
#4476=VERTEX_POINT('',#19672);
#4477=VERTEX_POINT('',#19680);
#4478=VERTEX_POINT('',#19682);
#4479=VERTEX_POINT('',#19690);
#4480=VERTEX_POINT('',#19701);
#4481=VERTEX_POINT('',#19709);
#4482=VERTEX_POINT('',#19711);
#4483=VERTEX_POINT('',#19719);
#4484=VERTEX_POINT('',#19730);
#4485=VERTEX_POINT('',#19738);
#4486=VERTEX_POINT('',#19740);
#4487=VERTEX_POINT('',#19748);
#4488=VERTEX_POINT('',#19755);
#4489=VERTEX_POINT('',#19758);
#4490=VERTEX_POINT('',#19769);
#4491=VERTEX_POINT('',#19777);
#4492=VERTEX_POINT('',#19779);
#4493=VERTEX_POINT('',#19787);
#4494=VERTEX_POINT('',#19798);
#4495=VERTEX_POINT('',#19806);
#4496=VERTEX_POINT('',#19808);
#4497=VERTEX_POINT('',#19816);
#4498=VERTEX_POINT('',#19827);
#4499=VERTEX_POINT('',#19835);
#4500=VERTEX_POINT('',#19837);
#4501=VERTEX_POINT('',#19845);
#4502=VERTEX_POINT('',#19856);
#4503=VERTEX_POINT('',#19864);
#4504=VERTEX_POINT('',#19866);
#4505=VERTEX_POINT('',#19874);
#4506=VERTEX_POINT('',#19885);
#4507=VERTEX_POINT('',#19893);
#4508=VERTEX_POINT('',#19895);
#4509=VERTEX_POINT('',#19903);
#4510=VERTEX_POINT('',#19914);
#4511=VERTEX_POINT('',#19922);
#4512=VERTEX_POINT('',#19924);
#4513=VERTEX_POINT('',#19932);
#4514=VERTEX_POINT('',#19943);
#4515=VERTEX_POINT('',#19951);
#4516=VERTEX_POINT('',#19953);
#4517=VERTEX_POINT('',#19961);
#4518=VERTEX_POINT('',#19972);
#4519=VERTEX_POINT('',#19980);
#4520=VERTEX_POINT('',#19982);
#4521=VERTEX_POINT('',#19990);
#4522=VERTEX_POINT('',#20001);
#4523=VERTEX_POINT('',#20009);
#4524=VERTEX_POINT('',#20011);
#4525=VERTEX_POINT('',#20019);
#4526=VERTEX_POINT('',#20030);
#4527=VERTEX_POINT('',#20038);
#4528=VERTEX_POINT('',#20040);
#4529=VERTEX_POINT('',#20048);
#4530=VERTEX_POINT('',#20059);
#4531=VERTEX_POINT('',#20067);
#4532=VERTEX_POINT('',#20069);
#4533=VERTEX_POINT('',#20077);
#4534=VERTEX_POINT('',#20088);
#4535=VERTEX_POINT('',#20096);
#4536=VERTEX_POINT('',#20098);
#4537=VERTEX_POINT('',#20106);
#4538=VERTEX_POINT('',#20117);
#4539=VERTEX_POINT('',#20125);
#4540=VERTEX_POINT('',#20127);
#4541=VERTEX_POINT('',#20135);
#4542=VERTEX_POINT('',#20146);
#4543=VERTEX_POINT('',#20154);
#4544=VERTEX_POINT('',#20156);
#4545=VERTEX_POINT('',#20164);
#4546=VERTEX_POINT('',#20175);
#4547=VERTEX_POINT('',#20183);
#4548=VERTEX_POINT('',#20185);
#4549=VERTEX_POINT('',#20193);
#4550=VERTEX_POINT('',#20204);
#4551=VERTEX_POINT('',#20212);
#4552=VERTEX_POINT('',#20214);
#4553=VERTEX_POINT('',#20222);
#4554=VERTEX_POINT('',#20233);
#4555=VERTEX_POINT('',#20241);
#4556=VERTEX_POINT('',#20243);
#4557=VERTEX_POINT('',#20251);
#4558=VERTEX_POINT('',#20262);
#4559=VERTEX_POINT('',#20270);
#4560=VERTEX_POINT('',#20272);
#4561=VERTEX_POINT('',#20280);
#4562=VERTEX_POINT('',#20291);
#4563=VERTEX_POINT('',#20299);
#4564=VERTEX_POINT('',#20301);
#4565=VERTEX_POINT('',#20309);
#4566=VERTEX_POINT('',#20320);
#4567=VERTEX_POINT('',#20328);
#4568=VERTEX_POINT('',#20330);
#4569=VERTEX_POINT('',#20338);
#4570=VERTEX_POINT('',#20349);
#4571=VERTEX_POINT('',#20357);
#4572=VERTEX_POINT('',#20359);
#4573=VERTEX_POINT('',#20367);
#4574=VERTEX_POINT('',#20378);
#4575=VERTEX_POINT('',#20386);
#4576=VERTEX_POINT('',#20396);
#4577=VERTEX_POINT('',#20397);
#4578=VERTEX_POINT('',#20399);
#4579=VERTEX_POINT('',#20401);
#4580=VERTEX_POINT('',#20405);
#4581=VERTEX_POINT('',#20406);
#4582=VERTEX_POINT('',#20419);
#4583=VERTEX_POINT('',#20427);
#4584=VERTEX_POINT('',#20429);
#4585=VERTEX_POINT('',#20437);
#4586=VERTEX_POINT('',#20448);
#4587=VERTEX_POINT('',#20456);
#4588=VERTEX_POINT('',#20458);
#4589=VERTEX_POINT('',#20466);
#4590=VERTEX_POINT('',#20477);
#4591=VERTEX_POINT('',#20485);
#4592=VERTEX_POINT('',#20487);
#4593=VERTEX_POINT('',#20495);
#4594=VERTEX_POINT('',#20506);
#4595=VERTEX_POINT('',#20514);
#4596=VERTEX_POINT('',#20516);
#4597=VERTEX_POINT('',#20524);
#4598=VERTEX_POINT('',#20535);
#4599=VERTEX_POINT('',#20543);
#4600=VERTEX_POINT('',#20545);
#4601=VERTEX_POINT('',#20553);
#4602=VERTEX_POINT('',#20564);
#4603=VERTEX_POINT('',#20572);
#4604=VERTEX_POINT('',#20574);
#4605=VERTEX_POINT('',#20582);
#4606=VERTEX_POINT('',#20593);
#4607=VERTEX_POINT('',#20601);
#4608=VERTEX_POINT('',#20603);
#4609=VERTEX_POINT('',#20611);
#4610=VERTEX_POINT('',#20622);
#4611=VERTEX_POINT('',#20630);
#4612=VERTEX_POINT('',#20632);
#4613=VERTEX_POINT('',#20640);
#4614=VERTEX_POINT('',#20651);
#4615=VERTEX_POINT('',#20659);
#4616=VERTEX_POINT('',#20661);
#4617=VERTEX_POINT('',#20669);
#4618=VERTEX_POINT('',#20680);
#4619=VERTEX_POINT('',#20688);
#4620=VERTEX_POINT('',#20690);
#4621=VERTEX_POINT('',#20698);
#4622=VERTEX_POINT('',#20709);
#4623=VERTEX_POINT('',#20717);
#4624=VERTEX_POINT('',#20719);
#4625=VERTEX_POINT('',#20727);
#4626=VERTEX_POINT('',#20738);
#4627=VERTEX_POINT('',#20746);
#4628=VERTEX_POINT('',#20748);
#4629=VERTEX_POINT('',#20756);
#4630=VERTEX_POINT('',#20767);
#4631=VERTEX_POINT('',#20775);
#4632=VERTEX_POINT('',#20777);
#4633=VERTEX_POINT('',#20785);
#4634=VERTEX_POINT('',#20796);
#4635=VERTEX_POINT('',#20804);
#4636=VERTEX_POINT('',#20806);
#4637=VERTEX_POINT('',#20814);
#4638=VERTEX_POINT('',#20825);
#4639=VERTEX_POINT('',#20833);
#4640=VERTEX_POINT('',#20835);
#4641=VERTEX_POINT('',#20843);
#4642=VERTEX_POINT('',#20854);
#4643=VERTEX_POINT('',#20862);
#4644=VERTEX_POINT('',#20864);
#4645=VERTEX_POINT('',#20872);
#4646=VERTEX_POINT('',#20883);
#4647=VERTEX_POINT('',#20891);
#4648=VERTEX_POINT('',#20893);
#4649=VERTEX_POINT('',#20901);
#4650=VERTEX_POINT('',#20912);
#4651=VERTEX_POINT('',#20920);
#4652=VERTEX_POINT('',#20922);
#4653=VERTEX_POINT('',#20930);
#4654=VERTEX_POINT('',#20941);
#4655=VERTEX_POINT('',#20949);
#4656=VERTEX_POINT('',#20951);
#4657=VERTEX_POINT('',#20959);
#4658=VERTEX_POINT('',#20970);
#4659=VERTEX_POINT('',#20978);
#4660=VERTEX_POINT('',#20980);
#4661=VERTEX_POINT('',#20988);
#4662=VERTEX_POINT('',#20999);
#4663=VERTEX_POINT('',#21007);
#4664=VERTEX_POINT('',#21009);
#4665=VERTEX_POINT('',#21017);
#4666=VERTEX_POINT('',#21028);
#4667=VERTEX_POINT('',#21036);
#4668=VERTEX_POINT('',#21038);
#4669=VERTEX_POINT('',#21046);
#4670=VERTEX_POINT('',#21057);
#4671=VERTEX_POINT('',#21060);
#4672=VERTEX_POINT('',#21067);
#4673=VERTEX_POINT('',#21075);
#4674=VERTEX_POINT('',#21077);
#4675=VERTEX_POINT('',#21085);
#4676=VERTEX_POINT('',#21096);
#4677=VERTEX_POINT('',#21104);
#4678=VERTEX_POINT('',#21106);
#4679=VERTEX_POINT('',#21114);
#4680=VERTEX_POINT('',#21125);
#4681=VERTEX_POINT('',#21133);
#4682=VERTEX_POINT('',#21135);
#4683=VERTEX_POINT('',#21143);
#4684=VERTEX_POINT('',#21154);
#4685=VERTEX_POINT('',#21162);
#4686=VERTEX_POINT('',#21164);
#4687=VERTEX_POINT('',#21172);
#4688=VERTEX_POINT('',#21183);
#4689=VERTEX_POINT('',#21191);
#4690=VERTEX_POINT('',#21193);
#4691=VERTEX_POINT('',#21201);
#4692=VERTEX_POINT('',#21212);
#4693=VERTEX_POINT('',#21220);
#4694=VERTEX_POINT('',#21222);
#4695=VERTEX_POINT('',#21230);
#4696=VERTEX_POINT('',#21241);
#4697=VERTEX_POINT('',#21249);
#4698=VERTEX_POINT('',#21251);
#4699=VERTEX_POINT('',#21259);
#4700=VERTEX_POINT('',#21270);
#4701=VERTEX_POINT('',#21278);
#4702=VERTEX_POINT('',#21280);
#4703=VERTEX_POINT('',#21288);
#4704=VERTEX_POINT('',#21299);
#4705=VERTEX_POINT('',#21307);
#4706=VERTEX_POINT('',#21309);
#4707=VERTEX_POINT('',#21317);
#4708=VERTEX_POINT('',#21328);
#4709=VERTEX_POINT('',#21336);
#4710=VERTEX_POINT('',#21338);
#4711=VERTEX_POINT('',#21346);
#4712=VERTEX_POINT('',#21357);
#4713=VERTEX_POINT('',#21365);
#4714=VERTEX_POINT('',#21367);
#4715=VERTEX_POINT('',#21375);
#4716=VERTEX_POINT('',#21386);
#4717=VERTEX_POINT('',#21394);
#4718=VERTEX_POINT('',#21396);
#4719=VERTEX_POINT('',#21404);
#4720=VERTEX_POINT('',#21415);
#4721=VERTEX_POINT('',#21423);
#4722=VERTEX_POINT('',#21425);
#4723=VERTEX_POINT('',#21433);
#4724=VERTEX_POINT('',#21444);
#4725=VERTEX_POINT('',#21452);
#4726=VERTEX_POINT('',#21454);
#4727=VERTEX_POINT('',#21462);
#4728=VERTEX_POINT('',#21473);
#4729=VERTEX_POINT('',#21481);
#4730=VERTEX_POINT('',#21483);
#4731=VERTEX_POINT('',#21491);
#4732=VERTEX_POINT('',#21502);
#4733=VERTEX_POINT('',#21510);
#4734=VERTEX_POINT('',#21512);
#4735=VERTEX_POINT('',#21520);
#4736=VERTEX_POINT('',#21531);
#4737=VERTEX_POINT('',#21539);
#4738=VERTEX_POINT('',#21541);
#4739=VERTEX_POINT('',#21549);
#4740=VERTEX_POINT('',#21560);
#4741=VERTEX_POINT('',#21568);
#4742=VERTEX_POINT('',#21570);
#4743=VERTEX_POINT('',#21578);
#4744=VERTEX_POINT('',#21589);
#4745=VERTEX_POINT('',#21597);
#4746=VERTEX_POINT('',#21599);
#4747=VERTEX_POINT('',#21607);
#4748=VERTEX_POINT('',#21618);
#4749=VERTEX_POINT('',#21626);
#4750=VERTEX_POINT('',#21628);
#4751=VERTEX_POINT('',#21636);
#4752=VERTEX_POINT('',#21647);
#4753=VERTEX_POINT('',#21655);
#4754=VERTEX_POINT('',#21657);
#4755=VERTEX_POINT('',#21665);
#4756=VERTEX_POINT('',#21676);
#4757=VERTEX_POINT('',#21684);
#4758=VERTEX_POINT('',#22838);
#4759=VERTEX_POINT('',#22840);
#4760=VERTEX_POINT('',#22844);
#4761=VERTEX_POINT('',#22846);
#4762=VERTEX_POINT('',#22890);
#4763=VERTEX_POINT('',#22943);
#4764=VERTEX_POINT('',#22945);
#4765=VERTEX_POINT('',#23222);
#4766=VERTEX_POINT('',#23312);
#4767=VERTEX_POINT('',#23355);
#4768=VERTEX_POINT('',#23394);
#4769=VERTEX_POINT('',#23484);
#4770=VERTEX_POINT('',#23527);
#4771=VERTEX_POINT('',#23566);
#4772=VERTEX_POINT('',#23609);
#4773=VERTEX_POINT('',#23652);
#4774=VERTEX_POINT('',#23691);
#4775=VERTEX_POINT('',#23781);
#4776=VERTEX_POINT('',#23824);
#4777=VERTEX_POINT('',#23863);
#4778=VERTEX_POINT('',#23953);
#4779=VERTEX_POINT('',#23996);
#4780=VERTEX_POINT('',#24035);
#4781=VERTEX_POINT('',#24125);
#4782=VERTEX_POINT('',#24168);
#4783=VERTEX_POINT('',#24207);
#4784=VERTEX_POINT('',#24297);
#4785=VERTEX_POINT('',#24340);
#4786=VERTEX_POINT('',#24379);
#4787=VERTEX_POINT('',#24469);
#4788=VERTEX_POINT('',#24512);
#4789=VERTEX_POINT('',#24551);
#4790=VERTEX_POINT('',#24641);
#4791=VERTEX_POINT('',#24684);
#4792=VERTEX_POINT('',#24723);
#4793=VERTEX_POINT('',#24813);
#4794=VERTEX_POINT('',#24856);
#4795=VERTEX_POINT('',#24895);
#4796=VERTEX_POINT('',#24985);
#4797=VERTEX_POINT('',#25028);
#4798=VERTEX_POINT('',#25067);
#4799=VERTEX_POINT('',#25110);
#4800=VERTEX_POINT('',#25153);
#4801=VERTEX_POINT('',#25192);
#4802=VERTEX_POINT('',#25282);
#4803=VERTEX_POINT('',#25325);
#4804=VERTEX_POINT('',#25364);
#4805=VERTEX_POINT('',#25454);
#4806=VERTEX_POINT('',#25497);
#4807=VERTEX_POINT('',#25536);
#4808=VERTEX_POINT('',#25579);
#4809=VERTEX_POINT('',#25622);
#4810=VERTEX_POINT('',#25661);
#4811=VERTEX_POINT('',#25751);
#4812=VERTEX_POINT('',#25794);
#4813=VERTEX_POINT('',#25833);
#4814=VERTEX_POINT('',#25923);
#4815=VERTEX_POINT('',#25966);
#4816=VERTEX_POINT('',#26005);
#4817=VERTEX_POINT('',#26095);
#4818=VERTEX_POINT('',#26138);
#4819=VERTEX_POINT('',#26177);
#4820=VERTEX_POINT('',#26267);
#4821=VERTEX_POINT('',#26310);
#4822=VERTEX_POINT('',#26349);
#4823=VERTEX_POINT('',#26439);
#4824=VERTEX_POINT('',#26482);
#4825=VERTEX_POINT('',#26521);
#4826=VERTEX_POINT('',#26611);
#4827=VERTEX_POINT('',#26654);
#4828=VERTEX_POINT('',#26693);
#4829=VERTEX_POINT('',#26783);
#4830=VERTEX_POINT('',#26826);
#4831=VERTEX_POINT('',#26865);
#4832=VERTEX_POINT('',#26955);
#4833=VERTEX_POINT('',#26998);
#4834=VERTEX_POINT('',#27037);
#4835=VERTEX_POINT('',#27127);
#4836=VERTEX_POINT('',#27170);
#4837=VERTEX_POINT('',#27209);
#4838=VERTEX_POINT('',#27252);
#4839=VERTEX_POINT('',#27295);
#4840=VERTEX_POINT('',#27334);
#4841=VERTEX_POINT('',#27377);
#4842=VERTEX_POINT('',#27420);
#4843=VERTEX_POINT('',#27459);
#4844=VERTEX_POINT('',#27549);
#4845=VERTEX_POINT('',#27592);
#4846=VERTEX_POINT('',#27631);
#4847=VERTEX_POINT('',#27721);
#4848=VERTEX_POINT('',#27764);
#4849=VERTEX_POINT('',#27803);
#4850=VERTEX_POINT('',#27893);
#4851=VERTEX_POINT('',#27936);
#4852=VERTEX_POINT('',#27975);
#4853=VERTEX_POINT('',#28065);
#4854=VERTEX_POINT('',#28108);
#4855=VERTEX_POINT('',#28147);
#4856=VERTEX_POINT('',#28237);
#4857=VERTEX_POINT('',#28280);
#4858=VERTEX_POINT('',#28319);
#4859=VERTEX_POINT('',#28409);
#4860=VERTEX_POINT('',#28452);
#4861=VERTEX_POINT('',#28491);
#4862=VERTEX_POINT('',#28534);
#4863=VERTEX_POINT('',#28577);
#4864=VERTEX_POINT('',#28616);
#4865=VERTEX_POINT('',#28659);
#4866=VERTEX_POINT('',#28702);
#4867=VERTEX_POINT('',#28741);
#4868=VERTEX_POINT('',#28831);
#4869=VERTEX_POINT('',#28874);
#4870=VERTEX_POINT('',#28913);
#4871=VERTEX_POINT('',#29003);
#4872=VERTEX_POINT('',#29046);
#4873=VERTEX_POINT('',#29085);
#4874=VERTEX_POINT('',#29128);
#4875=VERTEX_POINT('',#29171);
#4876=VERTEX_POINT('',#29210);
#4877=VERTEX_POINT('',#29300);
#4878=VERTEX_POINT('',#29343);
#4879=VERTEX_POINT('',#29382);
#4880=VERTEX_POINT('',#29472);
#4881=VERTEX_POINT('',#29515);
#4882=VERTEX_POINT('',#29554);
#4883=VERTEX_POINT('',#29644);
#4884=VERTEX_POINT('',#29687);
#4885=VERTEX_POINT('',#29726);
#4886=VERTEX_POINT('',#29816);
#4887=VERTEX_POINT('',#29859);
#4888=VERTEX_POINT('',#29898);
#4889=VERTEX_POINT('',#29988);
#4890=VERTEX_POINT('',#30031);
#4891=VERTEX_POINT('',#30070);
#4892=VERTEX_POINT('',#30113);
#4893=VERTEX_POINT('',#30156);
#4894=VERTEX_POINT('',#37223);
#4895=VERTEX_POINT('',#37225);
#4896=VERTEX_POINT('',#37229);
#4897=VERTEX_POINT('',#37231);
#4898=VERTEX_POINT('',#37235);
#4899=VERTEX_POINT('',#37237);
#4900=VERTEX_POINT('',#37241);
#4901=VERTEX_POINT('',#37243);
#4902=VERTEX_POINT('',#37247);
#4903=VERTEX_POINT('',#37249);
#4904=VERTEX_POINT('',#37253);
#4905=VERTEX_POINT('',#37255);
#4906=VERTEX_POINT('',#37259);
#4907=VERTEX_POINT('',#37261);
#4908=VERTEX_POINT('',#37265);
#4909=VERTEX_POINT('',#37267);
#4910=VERTEX_POINT('',#37271);
#4911=VERTEX_POINT('',#37273);
#4912=VERTEX_POINT('',#37277);
#4913=VERTEX_POINT('',#37279);
#4914=VERTEX_POINT('',#37283);
#4915=VERTEX_POINT('',#37285);
#4916=VERTEX_POINT('',#37289);
#4917=VERTEX_POINT('',#37291);
#4918=VERTEX_POINT('',#37295);
#4919=VERTEX_POINT('',#37297);
#4920=VERTEX_POINT('',#37301);
#4921=VERTEX_POINT('',#37302);
#4922=VERTEX_POINT('',#37304);
#4923=VERTEX_POINT('',#37306);
#4924=VERTEX_POINT('',#37308);
#4925=VERTEX_POINT('',#37310);
#4926=VERTEX_POINT('',#37312);
#4927=VERTEX_POINT('',#37314);
#4928=VERTEX_POINT('',#37318);
#4929=VERTEX_POINT('',#37319);
#4930=VERTEX_POINT('',#37321);
#4931=VERTEX_POINT('',#37323);
#4932=VERTEX_POINT('',#37327);
#4933=VERTEX_POINT('',#37328);
#4934=VERTEX_POINT('',#37330);
#4935=VERTEX_POINT('',#37332);
#4936=VERTEX_POINT('',#37336);
#4937=VERTEX_POINT('',#37337);
#4938=VERTEX_POINT('',#37339);
#4939=VERTEX_POINT('',#37341);
#4940=VERTEX_POINT('',#37345);
#4941=VERTEX_POINT('',#37346);
#4942=VERTEX_POINT('',#37348);
#4943=VERTEX_POINT('',#37350);
#4944=VERTEX_POINT('',#37354);
#4945=VERTEX_POINT('',#37358);
#4946=VERTEX_POINT('',#37360);
#4947=VERTEX_POINT('',#37362);
#4948=VERTEX_POINT('',#37366);
#4949=VERTEX_POINT('',#37368);
#4950=VERTEX_POINT('',#37370);
#4951=VERTEX_POINT('',#37372);
#4952=VERTEX_POINT('',#37374);
#4953=VERTEX_POINT('',#37376);
#4954=VERTEX_POINT('',#37380);
#4955=VERTEX_POINT('',#37385);
#4956=VERTEX_POINT('',#37394);
#4957=VERTEX_POINT('',#37396);
#4958=VERTEX_POINT('',#37402);
#4959=VERTEX_POINT('',#37409);
#4960=VERTEX_POINT('',#37416);
#4961=VERTEX_POINT('',#37417);
#4962=VERTEX_POINT('',#37419);
#4963=VERTEX_POINT('',#37421);
#4964=VERTEX_POINT('',#37440);
#4965=VERTEX_POINT('',#37441);
#4966=VERTEX_POINT('',#37443);
#4967=VERTEX_POINT('',#37445);
#4968=VERTEX_POINT('',#37449);
#4969=VERTEX_POINT('',#37450);
#4970=VERTEX_POINT('',#37452);
#4971=VERTEX_POINT('',#37454);
#4972=VERTEX_POINT('',#37458);
#4973=VERTEX_POINT('',#37459);
#4974=VERTEX_POINT('',#37461);
#4975=VERTEX_POINT('',#37463);
#4976=VERTEX_POINT('',#37467);
#4977=VERTEX_POINT('',#37468);
#4978=VERTEX_POINT('',#37470);
#4979=VERTEX_POINT('',#37472);
#4980=VERTEX_POINT('',#37476);
#4981=VERTEX_POINT('',#37477);
#4982=VERTEX_POINT('',#37479);
#4983=VERTEX_POINT('',#37481);
#4984=VERTEX_POINT('',#37485);
#4985=VERTEX_POINT('',#37486);
#4986=VERTEX_POINT('',#37488);
#4987=VERTEX_POINT('',#37490);
#4988=VERTEX_POINT('',#37539);
#4989=VERTEX_POINT('',#37541);
#4990=VERTEX_POINT('',#37545);
#4991=VERTEX_POINT('',#37547);
#4992=VERTEX_POINT('',#37551);
#4993=VERTEX_POINT('',#37553);
#4994=VERTEX_POINT('',#37557);
#4995=VERTEX_POINT('',#37559);
#4996=VERTEX_POINT('',#37563);
#4997=VERTEX_POINT('',#37565);
#4998=VERTEX_POINT('',#37569);
#4999=VERTEX_POINT('',#37571);
#5000=VERTEX_POINT('',#37575);
#5001=VERTEX_POINT('',#37577);
#5002=VERTEX_POINT('',#37581);
#5003=VERTEX_POINT('',#37583);
#5004=VERTEX_POINT('',#37590);
#5005=VERTEX_POINT('',#37592);
#5006=VERTEX_POINT('',#37596);
#5007=VERTEX_POINT('',#37598);
#5008=VERTEX_POINT('',#37602);
#5009=VERTEX_POINT('',#37604);
#5010=VERTEX_POINT('',#37608);
#5011=VERTEX_POINT('',#37610);
#5012=VERTEX_POINT('',#37614);
#5013=VERTEX_POINT('',#37616);
#5014=VERTEX_POINT('',#37620);
#5015=VERTEX_POINT('',#37622);
#5016=VERTEX_POINT('',#37626);
#5017=VERTEX_POINT('',#37628);
#5018=VERTEX_POINT('',#37632);
#5019=VERTEX_POINT('',#37634);
#5020=VERTEX_POINT('',#37641);
#5021=VERTEX_POINT('',#37643);
#5022=VERTEX_POINT('',#37647);
#5023=VERTEX_POINT('',#37649);
#5024=VERTEX_POINT('',#37651);
#5025=VERTEX_POINT('',#37655);
#5026=VERTEX_POINT('',#37659);
#5027=VERTEX_POINT('',#37667);
#5028=VERTEX_POINT('',#37669);
#5029=VERTEX_POINT('',#37673);
#5030=VERTEX_POINT('',#37674);
#5031=VERTEX_POINT('',#37676);
#5032=VERTEX_POINT('',#37678);
#5033=VERTEX_POINT('',#37682);
#5034=VERTEX_POINT('',#37684);
#5035=VERTEX_POINT('',#37688);
#5036=VERTEX_POINT('',#37690);
#5037=VERTEX_POINT('',#37694);
#5038=VERTEX_POINT('',#37696);
#5039=VERTEX_POINT('',#37700);
#5040=VERTEX_POINT('',#37702);
#5041=VERTEX_POINT('',#37713);
#5042=VERTEX_POINT('',#37714);
#5043=VERTEX_POINT('',#37716);
#5044=VERTEX_POINT('',#37718);
#5045=VERTEX_POINT('',#37722);
#5046=VERTEX_POINT('',#37723);
#5047=VERTEX_POINT('',#37725);
#5048=VERTEX_POINT('',#37727);
#5049=VERTEX_POINT('',#37731);
#5050=VERTEX_POINT('',#37732);
#5051=VERTEX_POINT('',#37734);
#5052=VERTEX_POINT('',#37736);
#5053=VERTEX_POINT('',#37740);
#5054=VERTEX_POINT('',#37741);
#5055=VERTEX_POINT('',#37743);
#5056=VERTEX_POINT('',#37745);
#5057=VERTEX_POINT('',#37749);
#5058=VERTEX_POINT('',#37751);
#5059=VERTEX_POINT('',#37755);
#5060=VERTEX_POINT('',#37757);
#5061=VERTEX_POINT('',#37761);
#5062=VERTEX_POINT('',#37762);
#5063=VERTEX_POINT('',#37764);
#5064=VERTEX_POINT('',#37766);
#5065=VERTEX_POINT('',#37770);
#5066=VERTEX_POINT('',#37771);
#5067=VERTEX_POINT('',#37773);
#5068=VERTEX_POINT('',#37775);
#5069=VERTEX_POINT('',#37800);
#5070=VERTEX_POINT('',#37802);
#5071=VERTEX_POINT('',#37806);
#5072=VERTEX_POINT('',#37808);
#5073=EDGE_CURVE('',#3998,#3998,#3473,.T.);
#5074=EDGE_CURVE('',#3998,#3999,#2871,.T.);
#5075=EDGE_CURVE('',#3999,#3999,#3474,.T.);
#5076=EDGE_CURVE('',#4000,#4000,#3475,.T.);
#5077=EDGE_CURVE('',#4000,#4001,#2872,.T.);
#5078=EDGE_CURVE('',#4001,#4001,#3476,.T.);
#5079=EDGE_CURVE('',#4002,#4002,#3477,.T.);
#5080=EDGE_CURVE('',#4002,#4003,#2873,.T.);
#5081=EDGE_CURVE('',#4003,#4003,#3478,.T.);
#5082=EDGE_CURVE('',#4004,#4004,#3479,.T.);
#5083=EDGE_CURVE('',#4004,#4005,#2874,.T.);
#5084=EDGE_CURVE('',#4005,#4005,#3480,.T.);
#5085=EDGE_CURVE('',#4006,#4006,#3481,.T.);
#5086=EDGE_CURVE('',#4006,#4007,#2875,.T.);
#5087=EDGE_CURVE('',#4007,#4007,#3482,.T.);
#5088=EDGE_CURVE('',#4008,#4008,#3483,.T.);
#5089=EDGE_CURVE('',#4008,#4009,#2876,.T.);
#5090=EDGE_CURVE('',#4009,#4009,#3484,.T.);
#5091=EDGE_CURVE('',#4010,#4010,#3485,.T.);
#5092=EDGE_CURVE('',#4010,#4011,#2877,.T.);
#5093=EDGE_CURVE('',#4011,#4011,#3486,.T.);
#5094=EDGE_CURVE('',#4012,#4012,#3487,.T.);
#5095=EDGE_CURVE('',#4012,#4013,#2878,.T.);
#5096=EDGE_CURVE('',#4013,#4013,#3488,.T.);
#5097=EDGE_CURVE('',#4014,#4014,#3489,.T.);
#5098=EDGE_CURVE('',#4014,#4015,#2879,.T.);
#5099=EDGE_CURVE('',#4015,#4015,#3490,.T.);
#5100=EDGE_CURVE('',#4016,#4016,#3491,.T.);
#5101=EDGE_CURVE('',#4016,#4017,#2880,.T.);
#5102=EDGE_CURVE('',#4017,#4017,#3492,.T.);
#5103=EDGE_CURVE('',#4018,#4018,#3493,.T.);
#5104=EDGE_CURVE('',#4018,#4019,#2881,.T.);
#5105=EDGE_CURVE('',#4019,#4019,#3494,.T.);
#5106=EDGE_CURVE('',#4020,#4021,#2882,.T.);
#5107=EDGE_CURVE('',#4022,#4020,#2883,.T.);
#5108=EDGE_CURVE('',#4023,#4022,#2884,.T.);
#5109=EDGE_CURVE('',#4024,#4023,#2885,.T.);
#5110=EDGE_CURVE('',#4025,#4024,#2886,.T.);
#5111=EDGE_CURVE('',#4025,#4026,#2887,.T.);
#5112=EDGE_CURVE('',#4026,#4027,#2888,.T.);
#5113=EDGE_CURVE('',#4027,#4021,#2889,.T.);
#5114=EDGE_CURVE('',#4028,#4029,#2890,.T.);
#5115=EDGE_CURVE('',#4030,#4028,#2891,.T.);
#5116=EDGE_CURVE('',#4031,#4030,#2892,.T.);
#5117=EDGE_CURVE('',#4031,#4029,#2893,.T.);
#5118=EDGE_CURVE('',#4032,#4033,#2894,.T.);
#5119=EDGE_CURVE('',#4032,#4034,#2895,.T.);
#5120=EDGE_CURVE('',#4035,#4034,#2896,.T.);
#5121=EDGE_CURVE('',#4033,#4035,#2897,.T.);
#5122=EDGE_CURVE('',#4036,#4037,#2898,.T.);
#5123=EDGE_CURVE('',#4038,#4036,#2899,.T.);
#5124=EDGE_CURVE('',#4039,#4038,#2900,.T.);
#5125=EDGE_CURVE('',#4039,#4037,#2901,.T.);
#5126=EDGE_CURVE('',#4040,#4041,#2902,.T.);
#5127=EDGE_CURVE('',#4040,#4042,#2903,.T.);
#5128=EDGE_CURVE('',#4043,#4042,#2904,.T.);
#5129=EDGE_CURVE('',#4041,#4043,#2905,.T.);
#5130=EDGE_CURVE('',#4044,#4023,#2906,.T.);
#5131=EDGE_CURVE('',#4044,#4045,#2907,.T.);
#5132=EDGE_CURVE('',#4045,#4046,#2908,.T.);
#5133=EDGE_CURVE('',#4046,#4047,#2909,.T.);
#5134=EDGE_CURVE('',#4033,#4047,#3495,.T.);
#5135=EDGE_CURVE('',#4030,#4035,#3496,.T.);
#5136=EDGE_CURVE('',#4024,#4028,#3497,.T.);
#5137=EDGE_CURVE('',#4047,#4048,#2910,.T.);
#5138=EDGE_CURVE('',#4049,#4046,#2911,.T.);
#5139=EDGE_CURVE('',#4050,#4049,#2912,.T.);
#5140=EDGE_CURVE('',#4051,#4050,#2913,.T.);
#5141=EDGE_CURVE('',#4051,#4052,#2914,.T.);
#5142=EDGE_CURVE('',#4052,#4053,#2915,.T.);
#5143=EDGE_CURVE('',#4053,#4048,#2916,.T.);
#5144=EDGE_CURVE('',#4054,#4049,#2917,.T.);
#5145=EDGE_CURVE('',#4054,#4055,#2918,.T.);
#5146=EDGE_CURVE('',#4055,#4022,#2919,.T.);
#5147=EDGE_CURVE('',#4020,#4041,#3498,.T.);
#5148=EDGE_CURVE('',#4043,#4038,#3499,.T.);
#5149=EDGE_CURVE('',#4036,#4050,#3500,.T.);
#5150=EDGE_CURVE('',#4045,#4054,#2920,.T.);
#5151=EDGE_CURVE('',#4055,#4044,#2921,.T.);
#5152=EDGE_CURVE('',#4029,#4025,#3501,.T.);
#5153=EDGE_CURVE('',#4034,#4031,#3502,.T.);
#5154=EDGE_CURVE('',#4048,#4032,#3503,.T.);
#5155=EDGE_CURVE('',#4056,#4053,#2922,.T.);
#5156=EDGE_CURVE('',#4056,#4057,#2923,.T.);
#5157=EDGE_CURVE('',#4057,#4026,#2924,.T.);
#5158=EDGE_CURVE('',#4057,#4058,#2925,.T.);
#5159=EDGE_CURVE('',#4058,#4027,#2926,.T.);
#5160=EDGE_CURVE('',#4021,#4040,#3504,.T.);
#5161=EDGE_CURVE('',#4058,#4059,#2927,.T.);
#5162=EDGE_CURVE('',#4059,#4052,#2928,.T.);
#5163=EDGE_CURVE('',#4037,#4051,#3505,.T.);
#5164=EDGE_CURVE('',#4042,#4039,#3506,.T.);
#5165=EDGE_CURVE('',#4059,#4056,#2929,.T.);
#5166=EDGE_CURVE('',#4060,#4061,#2930,.T.);
#5167=EDGE_CURVE('',#4061,#4062,#2931,.T.);
#5168=EDGE_CURVE('',#4062,#4063,#2932,.T.);
#5169=EDGE_CURVE('',#4063,#4060,#2933,.T.);
#5170=EDGE_CURVE('',#4045,#4063,#1369,.T.);
#5171=EDGE_CURVE('',#4060,#4044,#1370,.T.);
#5172=EDGE_CURVE('',#4061,#4055,#1371,.T.);
#5173=EDGE_CURVE('',#4054,#4062,#1372,.T.);
#5174=EDGE_CURVE('',#4064,#4065,#2934,.T.);
#5175=EDGE_CURVE('',#4065,#4066,#597,.T.);
#5176=EDGE_CURVE('',#4066,#4067,#2935,.T.);
#5177=EDGE_CURVE('',#4068,#4067,#598,.F.);
#5178=EDGE_CURVE('',#4068,#4069,#2936,.T.);
#5179=EDGE_CURVE('',#4069,#4069,#3507,.T.);
#5180=EDGE_CURVE('',#4064,#4068,#599,.F.);
#5181=EDGE_CURVE('',#4070,#4071,#2937,.T.);
#5182=EDGE_CURVE('',#4071,#4065,#600,.T.);
#5183=EDGE_CURVE('',#4070,#4064,#601,.F.);
#5184=EDGE_CURVE('',#4072,#4073,#2938,.T.);
#5185=EDGE_CURVE('',#4073,#4071,#602,.T.);
#5186=EDGE_CURVE('',#4072,#4070,#603,.F.);
#5187=EDGE_CURVE('',#4074,#4075,#2939,.T.);
#5188=EDGE_CURVE('',#4075,#4073,#604,.T.);
#5189=EDGE_CURVE('',#4076,#4072,#605,.F.);
#5190=EDGE_CURVE('',#4076,#4074,#606,.T.);
#5191=EDGE_CURVE('',#4077,#4078,#2940,.T.);
#5192=EDGE_CURVE('',#4079,#4078,#607,.F.);
#5193=EDGE_CURVE('',#4079,#4075,#608,.T.);
#5194=EDGE_CURVE('',#4074,#4077,#609,.T.);
#5195=EDGE_CURVE('',#4080,#4081,#2941,.T.);
#5196=EDGE_CURVE('',#4078,#4081,#610,.F.);
#5197=EDGE_CURVE('',#4077,#4080,#611,.T.);
#5198=EDGE_CURVE('',#4082,#4082,#3508,.T.);
#5199=EDGE_CURVE('',#4082,#4083,#2942,.T.);
#5200=EDGE_CURVE('',#4084,#4083,#612,.F.);
#5201=EDGE_CURVE('',#4085,#4084,#2943,.T.);
#5202=EDGE_CURVE('',#4085,#4086,#613,.T.);
#5203=EDGE_CURVE('',#4087,#4086,#2944,.T.);
#5204=EDGE_CURVE('',#4083,#4087,#614,.F.);
#5205=EDGE_CURVE('',#4088,#4089,#3509,.T.);
#5206=EDGE_CURVE('',#4089,#4088,#3510,.T.);
#5207=EDGE_CURVE('',#4089,#4090,#2945,.T.);
#5208=EDGE_CURVE('',#4090,#4090,#3511,.T.);
#5209=EDGE_CURVE('',#4091,#4092,#3512,.T.);
#5210=EDGE_CURVE('',#4093,#4091,#2946,.T.);
#5211=EDGE_CURVE('',#4094,#4093,#3513,.T.);
#5212=EDGE_CURVE('',#4094,#4095,#2947,.T.);
#5213=EDGE_CURVE('',#4095,#4095,#3514,.T.);
#5214=EDGE_CURVE('',#4096,#4094,#3515,.T.);
#5215=EDGE_CURVE('',#4092,#4096,#2948,.T.);
#5216=EDGE_CURVE('',#4097,#4097,#3516,.T.);
#5217=EDGE_CURVE('',#4097,#4098,#2949,.T.);
#5218=EDGE_CURVE('',#4098,#4098,#3517,.T.);
#5219=EDGE_CURVE('',#4099,#4099,#3518,.T.);
#5220=EDGE_CURVE('',#4099,#4088,#2950,.T.);
#5221=EDGE_CURVE('',#4081,#4084,#615,.F.);
#5222=EDGE_CURVE('',#4080,#4085,#616,.T.);
#5223=EDGE_CURVE('',#4100,#4087,#2951,.T.);
#5224=EDGE_CURVE('',#4086,#4101,#2952,.T.);
#5225=EDGE_CURVE('',#4101,#4100,#3519,.T.);
#5226=EDGE_CURVE('',#4102,#4076,#2953,.T.);
#5227=EDGE_CURVE('',#4102,#4101,#228,.T.);
#5228=EDGE_CURVE('',#4103,#4102,#3520,.T.);
#5229=EDGE_CURVE('',#4103,#4100,#229,.T.);
#5230=EDGE_CURVE('',#4079,#4103,#2954,.T.);
#5231=EDGE_CURVE('',#4104,#4066,#2955,.T.);
#5232=EDGE_CURVE('',#4105,#4104,#3521,.T.);
#5233=EDGE_CURVE('',#4067,#4105,#2956,.T.);
#5234=EDGE_CURVE('',#4102,#4105,#230,.T.);
#5235=EDGE_CURVE('',#4103,#4104,#231,.T.);
#5236=EDGE_CURVE('',#4106,#4093,#2957,.T.);
#5237=EDGE_CURVE('',#4107,#4106,#2958,.T.);
#5238=EDGE_CURVE('',#4096,#4107,#2959,.T.);
#5239=EDGE_CURVE('',#4108,#4091,#2960,.T.);
#5240=EDGE_CURVE('',#4108,#4106,#2961,.T.);
#5241=EDGE_CURVE('',#4109,#4108,#2962,.T.);
#5242=EDGE_CURVE('',#4109,#4107,#2963,.T.);
#5243=EDGE_CURVE('',#4092,#4109,#2964,.T.);
#5244=EDGE_CURVE('',#4110,#4111,#3522,.T.);
#5245=EDGE_CURVE('',#4111,#4110,#3523,.T.);
#5246=EDGE_CURVE('',#4111,#4112,#2965,.T.);
#5247=EDGE_CURVE('',#4112,#4112,#3524,.T.);
#5248=EDGE_CURVE('',#4113,#4113,#3525,.T.);
#5249=EDGE_CURVE('',#4113,#4114,#2966,.T.);
#5250=EDGE_CURVE('',#4114,#4114,#3526,.T.);
#5251=EDGE_CURVE('',#4115,#4116,#3527,.T.);
#5252=EDGE_CURVE('',#4115,#4117,#2967,.T.);
#5253=EDGE_CURVE('',#4117,#4118,#3528,.T.);
#5254=EDGE_CURVE('',#4116,#4118,#2968,.T.);
#5255=EDGE_CURVE('',#4110,#4119,#2969,.T.);
#5256=EDGE_CURVE('',#4119,#4119,#3529,.T.);
#5257=EDGE_CURVE('',#4120,#4120,#3530,.T.);
#5258=EDGE_CURVE('',#4120,#4121,#2970,.T.);
#5259=EDGE_CURVE('',#4122,#4121,#3531,.T.);
#5260=EDGE_CURVE('',#4123,#4122,#2971,.T.);
#5261=EDGE_CURVE('',#4124,#4123,#3532,.T.);
#5262=EDGE_CURVE('',#4124,#4125,#2972,.T.);
#5263=EDGE_CURVE('',#4121,#4125,#3533,.T.);
#5264=EDGE_CURVE('',#4126,#4127,#2973,.T.);
#5265=EDGE_CURVE('',#4126,#4122,#2974,.T.);
#5266=EDGE_CURVE('',#4127,#4125,#2975,.T.);
#5267=EDGE_CURVE('',#4128,#4117,#2976,.T.);
#5268=EDGE_CURVE('',#4129,#4115,#2977,.T.);
#5269=EDGE_CURVE('',#4129,#4128,#2978,.T.);
#5270=EDGE_CURVE('',#4130,#4118,#2979,.T.);
#5271=EDGE_CURVE('',#4131,#4130,#2980,.T.);
#5272=EDGE_CURVE('',#4131,#4116,#2981,.T.);
#5273=EDGE_CURVE('',#4128,#4130,#2982,.T.);
#5274=EDGE_CURVE('',#4129,#4131,#2983,.T.);
#5275=EDGE_CURVE('',#4132,#4123,#2984,.T.);
#5276=EDGE_CURVE('',#4132,#4133,#2985,.T.);
#5277=EDGE_CURVE('',#4133,#4124,#2986,.T.);
#5278=EDGE_CURVE('',#4132,#4126,#2987,.T.);
#5279=EDGE_CURVE('',#4133,#4127,#2988,.T.);
#5280=EDGE_CURVE('',#4134,#4135,#617,.T.);
#5281=EDGE_CURVE('',#4136,#4135,#618,.T.);
#5282=EDGE_CURVE('',#4137,#4136,#3534,.T.);
#5283=EDGE_CURVE('',#4138,#4137,#619,.T.);
#5284=EDGE_CURVE('',#4138,#4139,#620,.T.);
#5285=EDGE_CURVE('',#4134,#4139,#3535,.T.);
#5286=EDGE_CURVE('',#4140,#4141,#621,.T.);
#5287=EDGE_CURVE('',#4142,#4141,#622,.T.);
#5288=EDGE_CURVE('',#4143,#4142,#3536,.T.);
#5289=EDGE_CURVE('',#4144,#4143,#623,.T.);
#5290=EDGE_CURVE('',#4144,#4145,#624,.T.);
#5291=EDGE_CURVE('',#4140,#4145,#3537,.T.);
#5292=EDGE_CURVE('',#4146,#4147,#625,.T.);
#5293=EDGE_CURVE('',#4148,#4147,#626,.T.);
#5294=EDGE_CURVE('',#4149,#4148,#3538,.T.);
#5295=EDGE_CURVE('',#4150,#4149,#627,.T.);
#5296=EDGE_CURVE('',#4150,#4151,#628,.T.);
#5297=EDGE_CURVE('',#4146,#4151,#3539,.T.);
#5298=EDGE_CURVE('',#4152,#4153,#629,.T.);
#5299=EDGE_CURVE('',#4154,#4153,#630,.T.);
#5300=EDGE_CURVE('',#4155,#4154,#3540,.T.);
#5301=EDGE_CURVE('',#4156,#4155,#631,.T.);
#5302=EDGE_CURVE('',#4156,#4157,#632,.T.);
#5303=EDGE_CURVE('',#4152,#4157,#3541,.T.);
#5304=EDGE_CURVE('',#4158,#4159,#633,.T.);
#5305=EDGE_CURVE('',#4160,#4159,#634,.T.);
#5306=EDGE_CURVE('',#4161,#4160,#3542,.T.);
#5307=EDGE_CURVE('',#4162,#4161,#635,.T.);
#5308=EDGE_CURVE('',#4162,#4163,#636,.T.);
#5309=EDGE_CURVE('',#4158,#4163,#3543,.T.);
#5310=EDGE_CURVE('',#4164,#4165,#637,.T.);
#5311=EDGE_CURVE('',#4166,#4165,#638,.T.);
#5312=EDGE_CURVE('',#4167,#4166,#3544,.T.);
#5313=EDGE_CURVE('',#4168,#4167,#639,.T.);
#5314=EDGE_CURVE('',#4168,#4169,#640,.T.);
#5315=EDGE_CURVE('',#4164,#4169,#3545,.T.);
#5316=EDGE_CURVE('',#4170,#4171,#641,.T.);
#5317=EDGE_CURVE('',#4172,#4171,#642,.T.);
#5318=EDGE_CURVE('',#4173,#4172,#3546,.T.);
#5319=EDGE_CURVE('',#4174,#4173,#643,.T.);
#5320=EDGE_CURVE('',#4174,#4175,#644,.T.);
#5321=EDGE_CURVE('',#4170,#4175,#3547,.T.);
#5322=EDGE_CURVE('',#4176,#4177,#645,.T.);
#5323=EDGE_CURVE('',#4178,#4177,#646,.T.);
#5324=EDGE_CURVE('',#4179,#4178,#3548,.T.);
#5325=EDGE_CURVE('',#4180,#4179,#647,.T.);
#5326=EDGE_CURVE('',#4180,#4181,#648,.T.);
#5327=EDGE_CURVE('',#4176,#4181,#3549,.T.);
#5328=EDGE_CURVE('',#4182,#4183,#649,.T.);
#5329=EDGE_CURVE('',#4184,#4183,#650,.T.);
#5330=EDGE_CURVE('',#4185,#4184,#3550,.T.);
#5331=EDGE_CURVE('',#4186,#4185,#651,.T.);
#5332=EDGE_CURVE('',#4186,#4187,#652,.T.);
#5333=EDGE_CURVE('',#4182,#4187,#3551,.T.);
#5334=EDGE_CURVE('',#4188,#4189,#653,.T.);
#5335=EDGE_CURVE('',#4190,#4189,#654,.T.);
#5336=EDGE_CURVE('',#4191,#4190,#3552,.T.);
#5337=EDGE_CURVE('',#4192,#4191,#655,.T.);
#5338=EDGE_CURVE('',#4192,#4193,#656,.T.);
#5339=EDGE_CURVE('',#4188,#4193,#3553,.T.);
#5340=EDGE_CURVE('',#4194,#4195,#657,.T.);
#5341=EDGE_CURVE('',#4196,#4195,#658,.T.);
#5342=EDGE_CURVE('',#4197,#4196,#3554,.T.);
#5343=EDGE_CURVE('',#4198,#4197,#659,.T.);
#5344=EDGE_CURVE('',#4198,#4199,#660,.T.);
#5345=EDGE_CURVE('',#4194,#4199,#3555,.T.);
#5346=EDGE_CURVE('',#4200,#4201,#661,.T.);
#5347=EDGE_CURVE('',#4202,#4201,#662,.T.);
#5348=EDGE_CURVE('',#4203,#4202,#3556,.T.);
#5349=EDGE_CURVE('',#4204,#4203,#663,.T.);
#5350=EDGE_CURVE('',#4204,#4205,#664,.T.);
#5351=EDGE_CURVE('',#4200,#4205,#3557,.T.);
#5352=EDGE_CURVE('',#4206,#4207,#665,.T.);
#5353=EDGE_CURVE('',#4208,#4207,#666,.T.);
#5354=EDGE_CURVE('',#4209,#4208,#3558,.T.);
#5355=EDGE_CURVE('',#4210,#4209,#667,.T.);
#5356=EDGE_CURVE('',#4210,#4211,#668,.T.);
#5357=EDGE_CURVE('',#4206,#4211,#3559,.T.);
#5358=EDGE_CURVE('',#4212,#4213,#669,.T.);
#5359=EDGE_CURVE('',#4214,#4213,#670,.T.);
#5360=EDGE_CURVE('',#4215,#4214,#3560,.T.);
#5361=EDGE_CURVE('',#4216,#4215,#671,.T.);
#5362=EDGE_CURVE('',#4216,#4217,#672,.T.);
#5363=EDGE_CURVE('',#4212,#4217,#3561,.T.);
#5364=EDGE_CURVE('',#4218,#4219,#673,.T.);
#5365=EDGE_CURVE('',#4220,#4219,#674,.T.);
#5366=EDGE_CURVE('',#4221,#4220,#3562,.T.);
#5367=EDGE_CURVE('',#4222,#4221,#675,.T.);
#5368=EDGE_CURVE('',#4222,#4223,#676,.T.);
#5369=EDGE_CURVE('',#4218,#4223,#3563,.T.);
#5370=EDGE_CURVE('',#4224,#4225,#677,.T.);
#5371=EDGE_CURVE('',#4226,#4225,#678,.T.);
#5372=EDGE_CURVE('',#4227,#4226,#3564,.T.);
#5373=EDGE_CURVE('',#4228,#4227,#679,.T.);
#5374=EDGE_CURVE('',#4228,#4229,#680,.T.);
#5375=EDGE_CURVE('',#4224,#4229,#3565,.T.);
#5376=EDGE_CURVE('',#4230,#4231,#681,.T.);
#5377=EDGE_CURVE('',#4232,#4231,#682,.T.);
#5378=EDGE_CURVE('',#4233,#4232,#3566,.T.);
#5379=EDGE_CURVE('',#4234,#4233,#683,.T.);
#5380=EDGE_CURVE('',#4234,#4235,#684,.T.);
#5381=EDGE_CURVE('',#4230,#4235,#3567,.T.);
#5382=EDGE_CURVE('',#4236,#4237,#685,.T.);
#5383=EDGE_CURVE('',#4238,#4237,#686,.T.);
#5384=EDGE_CURVE('',#4239,#4238,#3568,.T.);
#5385=EDGE_CURVE('',#4240,#4239,#687,.T.);
#5386=EDGE_CURVE('',#4240,#4241,#688,.T.);
#5387=EDGE_CURVE('',#4236,#4241,#3569,.T.);
#5388=EDGE_CURVE('',#4242,#4243,#689,.T.);
#5389=EDGE_CURVE('',#4244,#4243,#690,.T.);
#5390=EDGE_CURVE('',#4245,#4244,#3570,.T.);
#5391=EDGE_CURVE('',#4246,#4245,#691,.T.);
#5392=EDGE_CURVE('',#4246,#4247,#692,.T.);
#5393=EDGE_CURVE('',#4242,#4247,#3571,.T.);
#5394=EDGE_CURVE('',#4248,#4249,#693,.T.);
#5395=EDGE_CURVE('',#4250,#4249,#694,.T.);
#5396=EDGE_CURVE('',#4251,#4250,#3572,.T.);
#5397=EDGE_CURVE('',#4252,#4251,#695,.T.);
#5398=EDGE_CURVE('',#4252,#4253,#696,.T.);
#5399=EDGE_CURVE('',#4248,#4253,#3573,.T.);
#5400=EDGE_CURVE('',#4254,#4255,#697,.T.);
#5401=EDGE_CURVE('',#4256,#4255,#698,.T.);
#5402=EDGE_CURVE('',#4257,#4256,#3574,.T.);
#5403=EDGE_CURVE('',#4258,#4257,#699,.T.);
#5404=EDGE_CURVE('',#4258,#4259,#700,.T.);
#5405=EDGE_CURVE('',#4254,#4259,#3575,.T.);
#5406=EDGE_CURVE('',#4260,#4261,#701,.T.);
#5407=EDGE_CURVE('',#4262,#4261,#702,.T.);
#5408=EDGE_CURVE('',#4263,#4262,#3576,.T.);
#5409=EDGE_CURVE('',#4264,#4263,#703,.T.);
#5410=EDGE_CURVE('',#4264,#4265,#704,.T.);
#5411=EDGE_CURVE('',#4260,#4265,#3577,.T.);
#5412=EDGE_CURVE('',#4266,#4267,#705,.T.);
#5413=EDGE_CURVE('',#4268,#4267,#706,.T.);
#5414=EDGE_CURVE('',#4269,#4268,#3578,.T.);
#5415=EDGE_CURVE('',#4270,#4269,#707,.T.);
#5416=EDGE_CURVE('',#4270,#4271,#708,.T.);
#5417=EDGE_CURVE('',#4266,#4271,#3579,.T.);
#5418=EDGE_CURVE('',#4272,#4273,#709,.T.);
#5419=EDGE_CURVE('',#4274,#4273,#710,.T.);
#5420=EDGE_CURVE('',#4275,#4274,#3580,.T.);
#5421=EDGE_CURVE('',#4276,#4275,#711,.T.);
#5422=EDGE_CURVE('',#4276,#4277,#712,.T.);
#5423=EDGE_CURVE('',#4272,#4277,#3581,.T.);
#5424=EDGE_CURVE('',#4278,#4279,#713,.T.);
#5425=EDGE_CURVE('',#4280,#4279,#714,.T.);
#5426=EDGE_CURVE('',#4281,#4280,#3582,.T.);
#5427=EDGE_CURVE('',#4282,#4281,#715,.T.);
#5428=EDGE_CURVE('',#4282,#4283,#716,.T.);
#5429=EDGE_CURVE('',#4278,#4283,#3583,.T.);
#5430=EDGE_CURVE('',#4284,#4285,#717,.T.);
#5431=EDGE_CURVE('',#4286,#4285,#718,.T.);
#5432=EDGE_CURVE('',#4287,#4286,#3584,.T.);
#5433=EDGE_CURVE('',#4288,#4287,#719,.T.);
#5434=EDGE_CURVE('',#4288,#4289,#720,.T.);
#5435=EDGE_CURVE('',#4284,#4289,#3585,.T.);
#5436=EDGE_CURVE('',#4290,#4291,#721,.T.);
#5437=EDGE_CURVE('',#4292,#4291,#722,.T.);
#5438=EDGE_CURVE('',#4293,#4292,#3586,.T.);
#5439=EDGE_CURVE('',#4294,#4293,#723,.T.);
#5440=EDGE_CURVE('',#4294,#4295,#724,.T.);
#5441=EDGE_CURVE('',#4290,#4295,#3587,.T.);
#5442=EDGE_CURVE('',#4296,#4297,#725,.T.);
#5443=EDGE_CURVE('',#4298,#4297,#726,.T.);
#5444=EDGE_CURVE('',#4299,#4298,#3588,.T.);
#5445=EDGE_CURVE('',#4300,#4299,#727,.T.);
#5446=EDGE_CURVE('',#4300,#4301,#728,.T.);
#5447=EDGE_CURVE('',#4296,#4301,#3589,.T.);
#5448=EDGE_CURVE('',#4302,#4303,#729,.T.);
#5449=EDGE_CURVE('',#4304,#4303,#730,.T.);
#5450=EDGE_CURVE('',#4305,#4304,#3590,.T.);
#5451=EDGE_CURVE('',#4306,#4305,#731,.T.);
#5452=EDGE_CURVE('',#4306,#4307,#732,.T.);
#5453=EDGE_CURVE('',#4302,#4307,#3591,.T.);
#5454=EDGE_CURVE('',#4308,#4309,#733,.T.);
#5455=EDGE_CURVE('',#4310,#4309,#734,.T.);
#5456=EDGE_CURVE('',#4311,#4310,#3592,.T.);
#5457=EDGE_CURVE('',#4312,#4311,#735,.T.);
#5458=EDGE_CURVE('',#4312,#4313,#736,.T.);
#5459=EDGE_CURVE('',#4308,#4313,#3593,.T.);
#5460=EDGE_CURVE('',#4314,#4315,#737,.T.);
#5461=EDGE_CURVE('',#4316,#4315,#738,.T.);
#5462=EDGE_CURVE('',#4317,#4316,#3594,.T.);
#5463=EDGE_CURVE('',#4318,#4317,#739,.T.);
#5464=EDGE_CURVE('',#4318,#4319,#740,.T.);
#5465=EDGE_CURVE('',#4314,#4319,#3595,.T.);
#5466=EDGE_CURVE('',#4320,#4321,#741,.T.);
#5467=EDGE_CURVE('',#4322,#4321,#742,.T.);
#5468=EDGE_CURVE('',#4323,#4322,#3596,.T.);
#5469=EDGE_CURVE('',#4324,#4323,#743,.T.);
#5470=EDGE_CURVE('',#4324,#4325,#744,.T.);
#5471=EDGE_CURVE('',#4320,#4325,#3597,.T.);
#5472=EDGE_CURVE('',#4326,#4327,#745,.T.);
#5473=EDGE_CURVE('',#4328,#4327,#746,.T.);
#5474=EDGE_CURVE('',#4329,#4328,#3598,.T.);
#5475=EDGE_CURVE('',#4330,#4329,#747,.T.);
#5476=EDGE_CURVE('',#4330,#4331,#748,.T.);
#5477=EDGE_CURVE('',#4326,#4331,#3599,.T.);
#5478=EDGE_CURVE('',#4332,#4333,#749,.T.);
#5479=EDGE_CURVE('',#4334,#4333,#750,.T.);
#5480=EDGE_CURVE('',#4335,#4334,#3600,.T.);
#5481=EDGE_CURVE('',#4336,#4335,#751,.T.);
#5482=EDGE_CURVE('',#4336,#4337,#752,.T.);
#5483=EDGE_CURVE('',#4332,#4337,#3601,.T.);
#5484=EDGE_CURVE('',#4338,#4339,#753,.T.);
#5485=EDGE_CURVE('',#4340,#4339,#754,.T.);
#5486=EDGE_CURVE('',#4341,#4340,#3602,.T.);
#5487=EDGE_CURVE('',#4342,#4341,#755,.T.);
#5488=EDGE_CURVE('',#4342,#4343,#756,.T.);
#5489=EDGE_CURVE('',#4338,#4343,#3603,.T.);
#5490=EDGE_CURVE('',#4344,#4345,#757,.T.);
#5491=EDGE_CURVE('',#4346,#4345,#758,.T.);
#5492=EDGE_CURVE('',#4347,#4346,#3604,.T.);
#5493=EDGE_CURVE('',#4348,#4347,#759,.T.);
#5494=EDGE_CURVE('',#4348,#4349,#760,.T.);
#5495=EDGE_CURVE('',#4344,#4349,#3605,.T.);
#5496=EDGE_CURVE('',#4350,#4351,#761,.T.);
#5497=EDGE_CURVE('',#4352,#4351,#762,.T.);
#5498=EDGE_CURVE('',#4353,#4352,#3606,.T.);
#5499=EDGE_CURVE('',#4354,#4353,#763,.T.);
#5500=EDGE_CURVE('',#4354,#4355,#764,.T.);
#5501=EDGE_CURVE('',#4350,#4355,#3607,.T.);
#5502=EDGE_CURVE('',#4356,#4357,#765,.T.);
#5503=EDGE_CURVE('',#4358,#4357,#766,.T.);
#5504=EDGE_CURVE('',#4359,#4358,#3608,.T.);
#5505=EDGE_CURVE('',#4360,#4359,#767,.T.);
#5506=EDGE_CURVE('',#4360,#4361,#768,.T.);
#5507=EDGE_CURVE('',#4356,#4361,#3609,.T.);
#5508=EDGE_CURVE('',#4362,#4363,#769,.T.);
#5509=EDGE_CURVE('',#4364,#4363,#770,.T.);
#5510=EDGE_CURVE('',#4365,#4364,#3610,.T.);
#5511=EDGE_CURVE('',#4366,#4365,#771,.T.);
#5512=EDGE_CURVE('',#4366,#4367,#772,.T.);
#5513=EDGE_CURVE('',#4362,#4367,#3611,.T.);
#5514=EDGE_CURVE('',#4368,#4369,#773,.T.);
#5515=EDGE_CURVE('',#4370,#4369,#774,.T.);
#5516=EDGE_CURVE('',#4371,#4370,#3612,.T.);
#5517=EDGE_CURVE('',#4372,#4371,#775,.T.);
#5518=EDGE_CURVE('',#4372,#4373,#776,.T.);
#5519=EDGE_CURVE('',#4368,#4373,#3613,.T.);
#5520=EDGE_CURVE('',#4374,#4375,#777,.T.);
#5521=EDGE_CURVE('',#4376,#4375,#778,.T.);
#5522=EDGE_CURVE('',#4377,#4376,#3614,.T.);
#5523=EDGE_CURVE('',#4378,#4377,#779,.T.);
#5524=EDGE_CURVE('',#4378,#4379,#780,.T.);
#5525=EDGE_CURVE('',#4374,#4379,#3615,.T.);
#5526=EDGE_CURVE('',#4380,#4381,#781,.T.);
#5527=EDGE_CURVE('',#4382,#4381,#782,.T.);
#5528=EDGE_CURVE('',#4383,#4382,#3616,.T.);
#5529=EDGE_CURVE('',#4384,#4383,#783,.T.);
#5530=EDGE_CURVE('',#4384,#4385,#784,.T.);
#5531=EDGE_CURVE('',#4380,#4385,#3617,.T.);
#5532=EDGE_CURVE('',#4386,#4387,#785,.T.);
#5533=EDGE_CURVE('',#4388,#4387,#786,.T.);
#5534=EDGE_CURVE('',#4389,#4388,#3618,.T.);
#5535=EDGE_CURVE('',#4390,#4389,#787,.T.);
#5536=EDGE_CURVE('',#4390,#4391,#788,.T.);
#5537=EDGE_CURVE('',#4386,#4391,#3619,.T.);
#5538=EDGE_CURVE('',#4392,#4393,#789,.T.);
#5539=EDGE_CURVE('',#4394,#4393,#790,.T.);
#5540=EDGE_CURVE('',#4395,#4394,#3620,.T.);
#5541=EDGE_CURVE('',#4396,#4395,#791,.T.);
#5542=EDGE_CURVE('',#4396,#4397,#792,.T.);
#5543=EDGE_CURVE('',#4392,#4397,#3621,.T.);
#5544=EDGE_CURVE('',#4398,#4399,#793,.T.);
#5545=EDGE_CURVE('',#4400,#4398,#794,.T.);
#5546=EDGE_CURVE('',#4401,#4400,#3622,.T.);
#5547=EDGE_CURVE('',#4402,#4401,#795,.T.);
#5548=EDGE_CURVE('',#4403,#4402,#796,.T.);
#5549=EDGE_CURVE('',#4404,#4403,#797,.T.);
#5550=EDGE_CURVE('',#4405,#4404,#3623,.T.);
#5551=EDGE_CURVE('',#4406,#4405,#798,.T.);
#5552=EDGE_CURVE('',#4407,#4406,#799,.T.);
#5553=EDGE_CURVE('',#4408,#4407,#800,.T.);
#5554=EDGE_CURVE('',#4409,#4408,#3624,.T.);
#5555=EDGE_CURVE('',#4410,#4409,#801,.T.);
#5556=EDGE_CURVE('',#4411,#4410,#802,.T.);
#5557=EDGE_CURVE('',#4412,#4411,#803,.T.);
#5558=EDGE_CURVE('',#4413,#4412,#3625,.T.);
#5559=EDGE_CURVE('',#4414,#4413,#804,.T.);
#5560=EDGE_CURVE('',#4415,#4414,#805,.T.);
#5561=EDGE_CURVE('',#4416,#4415,#806,.T.);
#5562=EDGE_CURVE('',#4417,#4416,#3626,.T.);
#5563=EDGE_CURVE('',#4418,#4417,#807,.T.);
#5564=EDGE_CURVE('',#4419,#4418,#808,.T.);
#5565=EDGE_CURVE('',#4420,#4419,#809,.T.);
#5566=EDGE_CURVE('',#4421,#4420,#3627,.T.);
#5567=EDGE_CURVE('',#4422,#4421,#810,.T.);
#5568=EDGE_CURVE('',#4423,#4422,#811,.T.);
#5569=EDGE_CURVE('',#4424,#4423,#812,.T.);
#5570=EDGE_CURVE('',#4425,#4424,#3628,.T.);
#5571=EDGE_CURVE('',#4426,#4425,#813,.T.);
#5572=EDGE_CURVE('',#4427,#4426,#814,.T.);
#5573=EDGE_CURVE('',#4428,#4427,#815,.T.);
#5574=EDGE_CURVE('',#4429,#4428,#3629,.T.);
#5575=EDGE_CURVE('',#4430,#4429,#816,.T.);
#5576=EDGE_CURVE('',#4431,#4430,#817,.T.);
#5577=EDGE_CURVE('',#4432,#4431,#818,.T.);
#5578=EDGE_CURVE('',#4433,#4432,#3630,.T.);
#5579=EDGE_CURVE('',#4434,#4433,#819,.T.);
#5580=EDGE_CURVE('',#4435,#4434,#820,.T.);
#5581=EDGE_CURVE('',#4436,#4435,#821,.T.);
#5582=EDGE_CURVE('',#4437,#4436,#3631,.T.);
#5583=EDGE_CURVE('',#4438,#4437,#822,.T.);
#5584=EDGE_CURVE('',#4439,#4438,#823,.T.);
#5585=EDGE_CURVE('',#4440,#4439,#824,.T.);
#5586=EDGE_CURVE('',#4441,#4440,#3632,.T.);
#5587=EDGE_CURVE('',#4442,#4441,#825,.T.);
#5588=EDGE_CURVE('',#4443,#4442,#826,.T.);
#5589=EDGE_CURVE('',#4444,#4443,#827,.T.);
#5590=EDGE_CURVE('',#4445,#4444,#3633,.T.);
#5591=EDGE_CURVE('',#4446,#4445,#828,.T.);
#5592=EDGE_CURVE('',#4447,#4446,#829,.T.);
#5593=EDGE_CURVE('',#4448,#4447,#830,.T.);
#5594=EDGE_CURVE('',#4449,#4448,#3634,.T.);
#5595=EDGE_CURVE('',#4450,#4449,#831,.T.);
#5596=EDGE_CURVE('',#4451,#4450,#832,.T.);
#5597=EDGE_CURVE('',#4452,#4451,#833,.T.);
#5598=EDGE_CURVE('',#4453,#4452,#3635,.T.);
#5599=EDGE_CURVE('',#4454,#4453,#834,.T.);
#5600=EDGE_CURVE('',#4455,#4454,#835,.T.);
#5601=EDGE_CURVE('',#4456,#4455,#836,.T.);
#5602=EDGE_CURVE('',#4457,#4456,#3636,.T.);
#5603=EDGE_CURVE('',#4458,#4457,#837,.T.);
#5604=EDGE_CURVE('',#4459,#4458,#838,.T.);
#5605=EDGE_CURVE('',#4460,#4459,#839,.T.);
#5606=EDGE_CURVE('',#4461,#4460,#3637,.T.);
#5607=EDGE_CURVE('',#4462,#4461,#840,.T.);
#5608=EDGE_CURVE('',#4463,#4462,#841,.T.);
#5609=EDGE_CURVE('',#4464,#4463,#842,.T.);
#5610=EDGE_CURVE('',#4465,#4464,#3638,.T.);
#5611=EDGE_CURVE('',#4466,#4465,#843,.T.);
#5612=EDGE_CURVE('',#4467,#4466,#844,.T.);
#5613=EDGE_CURVE('',#4468,#4467,#845,.T.);
#5614=EDGE_CURVE('',#4469,#4468,#3639,.T.);
#5615=EDGE_CURVE('',#4470,#4469,#846,.T.);
#5616=EDGE_CURVE('',#4471,#4470,#847,.T.);
#5617=EDGE_CURVE('',#4472,#4471,#848,.T.);
#5618=EDGE_CURVE('',#4473,#4472,#3640,.T.);
#5619=EDGE_CURVE('',#4474,#4473,#849,.T.);
#5620=EDGE_CURVE('',#4475,#4474,#850,.T.);
#5621=EDGE_CURVE('',#4476,#4475,#851,.T.);
#5622=EDGE_CURVE('',#4477,#4476,#3641,.T.);
#5623=EDGE_CURVE('',#4478,#4477,#852,.T.);
#5624=EDGE_CURVE('',#4479,#4478,#853,.T.);
#5625=EDGE_CURVE('',#4480,#4479,#854,.T.);
#5626=EDGE_CURVE('',#4481,#4480,#3642,.T.);
#5627=EDGE_CURVE('',#4482,#4481,#855,.T.);
#5628=EDGE_CURVE('',#4483,#4482,#856,.T.);
#5629=EDGE_CURVE('',#4484,#4483,#857,.T.);
#5630=EDGE_CURVE('',#4485,#4484,#3643,.T.);
#5631=EDGE_CURVE('',#4486,#4485,#858,.T.);
#5632=EDGE_CURVE('',#4487,#4486,#859,.F.);
#5633=EDGE_CURVE('',#4487,#4488,#2989,.T.);
#5634=EDGE_CURVE('',#4488,#4488,#3644,.T.);
#5635=EDGE_CURVE('',#4489,#4487,#860,.F.);
#5636=EDGE_CURVE('',#4490,#4489,#861,.T.);
#5637=EDGE_CURVE('',#4491,#4490,#3645,.T.);
#5638=EDGE_CURVE('',#4492,#4491,#862,.T.);
#5639=EDGE_CURVE('',#4493,#4492,#863,.T.);
#5640=EDGE_CURVE('',#4494,#4493,#864,.T.);
#5641=EDGE_CURVE('',#4495,#4494,#3646,.T.);
#5642=EDGE_CURVE('',#4496,#4495,#865,.T.);
#5643=EDGE_CURVE('',#4497,#4496,#866,.T.);
#5644=EDGE_CURVE('',#4498,#4497,#867,.T.);
#5645=EDGE_CURVE('',#4499,#4498,#3647,.T.);
#5646=EDGE_CURVE('',#4500,#4499,#868,.T.);
#5647=EDGE_CURVE('',#4501,#4500,#869,.T.);
#5648=EDGE_CURVE('',#4502,#4501,#870,.T.);
#5649=EDGE_CURVE('',#4503,#4502,#3648,.T.);
#5650=EDGE_CURVE('',#4504,#4503,#871,.T.);
#5651=EDGE_CURVE('',#4505,#4504,#872,.T.);
#5652=EDGE_CURVE('',#4506,#4505,#873,.T.);
#5653=EDGE_CURVE('',#4507,#4506,#3649,.T.);
#5654=EDGE_CURVE('',#4508,#4507,#874,.T.);
#5655=EDGE_CURVE('',#4509,#4508,#875,.T.);
#5656=EDGE_CURVE('',#4510,#4509,#876,.T.);
#5657=EDGE_CURVE('',#4511,#4510,#3650,.T.);
#5658=EDGE_CURVE('',#4512,#4511,#877,.T.);
#5659=EDGE_CURVE('',#4513,#4512,#878,.T.);
#5660=EDGE_CURVE('',#4514,#4513,#879,.T.);
#5661=EDGE_CURVE('',#4515,#4514,#3651,.T.);
#5662=EDGE_CURVE('',#4516,#4515,#880,.T.);
#5663=EDGE_CURVE('',#4517,#4516,#881,.T.);
#5664=EDGE_CURVE('',#4518,#4517,#882,.T.);
#5665=EDGE_CURVE('',#4519,#4518,#3652,.T.);
#5666=EDGE_CURVE('',#4520,#4519,#883,.T.);
#5667=EDGE_CURVE('',#4521,#4520,#884,.T.);
#5668=EDGE_CURVE('',#4522,#4521,#885,.T.);
#5669=EDGE_CURVE('',#4523,#4522,#3653,.T.);
#5670=EDGE_CURVE('',#4524,#4523,#886,.T.);
#5671=EDGE_CURVE('',#4525,#4524,#887,.T.);
#5672=EDGE_CURVE('',#4526,#4525,#888,.T.);
#5673=EDGE_CURVE('',#4527,#4526,#3654,.T.);
#5674=EDGE_CURVE('',#4528,#4527,#889,.T.);
#5675=EDGE_CURVE('',#4529,#4528,#890,.T.);
#5676=EDGE_CURVE('',#4530,#4529,#891,.T.);
#5677=EDGE_CURVE('',#4531,#4530,#3655,.T.);
#5678=EDGE_CURVE('',#4532,#4531,#892,.T.);
#5679=EDGE_CURVE('',#4533,#4532,#893,.T.);
#5680=EDGE_CURVE('',#4534,#4533,#894,.T.);
#5681=EDGE_CURVE('',#4535,#4534,#3656,.T.);
#5682=EDGE_CURVE('',#4536,#4535,#895,.T.);
#5683=EDGE_CURVE('',#4537,#4536,#896,.T.);
#5684=EDGE_CURVE('',#4538,#4537,#897,.T.);
#5685=EDGE_CURVE('',#4539,#4538,#3657,.T.);
#5686=EDGE_CURVE('',#4540,#4539,#898,.T.);
#5687=EDGE_CURVE('',#4541,#4540,#899,.T.);
#5688=EDGE_CURVE('',#4542,#4541,#900,.T.);
#5689=EDGE_CURVE('',#4543,#4542,#3658,.T.);
#5690=EDGE_CURVE('',#4544,#4543,#901,.T.);
#5691=EDGE_CURVE('',#4545,#4544,#902,.T.);
#5692=EDGE_CURVE('',#4546,#4545,#903,.T.);
#5693=EDGE_CURVE('',#4547,#4546,#3659,.T.);
#5694=EDGE_CURVE('',#4548,#4547,#904,.T.);
#5695=EDGE_CURVE('',#4549,#4548,#905,.T.);
#5696=EDGE_CURVE('',#4550,#4549,#906,.T.);
#5697=EDGE_CURVE('',#4551,#4550,#3660,.T.);
#5698=EDGE_CURVE('',#4552,#4551,#907,.T.);
#5699=EDGE_CURVE('',#4553,#4552,#908,.T.);
#5700=EDGE_CURVE('',#4554,#4553,#909,.T.);
#5701=EDGE_CURVE('',#4555,#4554,#3661,.T.);
#5702=EDGE_CURVE('',#4556,#4555,#910,.T.);
#5703=EDGE_CURVE('',#4557,#4556,#911,.T.);
#5704=EDGE_CURVE('',#4558,#4557,#912,.T.);
#5705=EDGE_CURVE('',#4559,#4558,#3662,.T.);
#5706=EDGE_CURVE('',#4560,#4559,#913,.T.);
#5707=EDGE_CURVE('',#4561,#4560,#914,.T.);
#5708=EDGE_CURVE('',#4562,#4561,#915,.T.);
#5709=EDGE_CURVE('',#4563,#4562,#3663,.T.);
#5710=EDGE_CURVE('',#4564,#4563,#916,.T.);
#5711=EDGE_CURVE('',#4565,#4564,#917,.T.);
#5712=EDGE_CURVE('',#4566,#4565,#918,.T.);
#5713=EDGE_CURVE('',#4567,#4566,#3664,.T.);
#5714=EDGE_CURVE('',#4568,#4567,#919,.T.);
#5715=EDGE_CURVE('',#4569,#4568,#920,.T.);
#5716=EDGE_CURVE('',#4570,#4569,#921,.T.);
#5717=EDGE_CURVE('',#4571,#4570,#3665,.T.);
#5718=EDGE_CURVE('',#4572,#4571,#922,.T.);
#5719=EDGE_CURVE('',#4573,#4572,#923,.T.);
#5720=EDGE_CURVE('',#4574,#4573,#924,.T.);
#5721=EDGE_CURVE('',#4575,#4574,#3666,.T.);
#5722=EDGE_CURVE('',#4399,#4575,#925,.T.);
#5723=EDGE_CURVE('',#4576,#4577,#3667,.T.);
#5724=EDGE_CURVE('',#4577,#4578,#2990,.T.);
#5725=EDGE_CURVE('',#4579,#4578,#3668,.T.);
#5726=EDGE_CURVE('',#4576,#4579,#2991,.T.);
#5727=EDGE_CURVE('',#4580,#4581,#926,.F.);
#5728=EDGE_CURVE('',#4581,#4582,#927,.T.);
#5729=EDGE_CURVE('',#4583,#4582,#3669,.T.);
#5730=EDGE_CURVE('',#4583,#4584,#928,.T.);
#5731=EDGE_CURVE('',#4584,#4585,#929,.T.);
#5732=EDGE_CURVE('',#4585,#4586,#930,.T.);
#5733=EDGE_CURVE('',#4587,#4586,#3670,.T.);
#5734=EDGE_CURVE('',#4587,#4588,#931,.T.);
#5735=EDGE_CURVE('',#4588,#4589,#932,.T.);
#5736=EDGE_CURVE('',#4589,#4590,#933,.T.);
#5737=EDGE_CURVE('',#4591,#4590,#3671,.T.);
#5738=EDGE_CURVE('',#4591,#4592,#934,.T.);
#5739=EDGE_CURVE('',#4592,#4593,#935,.T.);
#5740=EDGE_CURVE('',#4593,#4594,#936,.T.);
#5741=EDGE_CURVE('',#4595,#4594,#3672,.T.);
#5742=EDGE_CURVE('',#4595,#4596,#937,.T.);
#5743=EDGE_CURVE('',#4596,#4597,#938,.T.);
#5744=EDGE_CURVE('',#4597,#4598,#939,.T.);
#5745=EDGE_CURVE('',#4599,#4598,#3673,.T.);
#5746=EDGE_CURVE('',#4599,#4600,#940,.T.);
#5747=EDGE_CURVE('',#4600,#4601,#941,.T.);
#5748=EDGE_CURVE('',#4601,#4602,#942,.T.);
#5749=EDGE_CURVE('',#4603,#4602,#3674,.T.);
#5750=EDGE_CURVE('',#4603,#4604,#943,.T.);
#5751=EDGE_CURVE('',#4604,#4605,#944,.T.);
#5752=EDGE_CURVE('',#4605,#4606,#945,.T.);
#5753=EDGE_CURVE('',#4607,#4606,#3675,.T.);
#5754=EDGE_CURVE('',#4607,#4608,#946,.T.);
#5755=EDGE_CURVE('',#4608,#4609,#947,.T.);
#5756=EDGE_CURVE('',#4609,#4610,#948,.T.);
#5757=EDGE_CURVE('',#4611,#4610,#3676,.T.);
#5758=EDGE_CURVE('',#4611,#4612,#949,.T.);
#5759=EDGE_CURVE('',#4612,#4613,#950,.T.);
#5760=EDGE_CURVE('',#4613,#4614,#951,.T.);
#5761=EDGE_CURVE('',#4615,#4614,#3677,.T.);
#5762=EDGE_CURVE('',#4615,#4616,#952,.T.);
#5763=EDGE_CURVE('',#4616,#4617,#953,.T.);
#5764=EDGE_CURVE('',#4617,#4618,#954,.T.);
#5765=EDGE_CURVE('',#4619,#4618,#3678,.T.);
#5766=EDGE_CURVE('',#4619,#4620,#955,.T.);
#5767=EDGE_CURVE('',#4620,#4621,#956,.T.);
#5768=EDGE_CURVE('',#4621,#4622,#957,.T.);
#5769=EDGE_CURVE('',#4623,#4622,#3679,.T.);
#5770=EDGE_CURVE('',#4623,#4624,#958,.T.);
#5771=EDGE_CURVE('',#4624,#4625,#959,.T.);
#5772=EDGE_CURVE('',#4625,#4626,#960,.T.);
#5773=EDGE_CURVE('',#4627,#4626,#3680,.T.);
#5774=EDGE_CURVE('',#4627,#4628,#961,.T.);
#5775=EDGE_CURVE('',#4628,#4629,#962,.T.);
#5776=EDGE_CURVE('',#4629,#4630,#963,.T.);
#5777=EDGE_CURVE('',#4631,#4630,#3681,.T.);
#5778=EDGE_CURVE('',#4631,#4632,#964,.T.);
#5779=EDGE_CURVE('',#4632,#4633,#965,.T.);
#5780=EDGE_CURVE('',#4633,#4634,#966,.T.);
#5781=EDGE_CURVE('',#4635,#4634,#3682,.T.);
#5782=EDGE_CURVE('',#4635,#4636,#967,.T.);
#5783=EDGE_CURVE('',#4636,#4637,#968,.T.);
#5784=EDGE_CURVE('',#4637,#4638,#969,.T.);
#5785=EDGE_CURVE('',#4639,#4638,#3683,.T.);
#5786=EDGE_CURVE('',#4639,#4640,#970,.T.);
#5787=EDGE_CURVE('',#4640,#4641,#971,.T.);
#5788=EDGE_CURVE('',#4641,#4642,#972,.T.);
#5789=EDGE_CURVE('',#4643,#4642,#3684,.T.);
#5790=EDGE_CURVE('',#4643,#4644,#973,.T.);
#5791=EDGE_CURVE('',#4644,#4645,#974,.T.);
#5792=EDGE_CURVE('',#4645,#4646,#975,.T.);
#5793=EDGE_CURVE('',#4647,#4646,#3685,.T.);
#5794=EDGE_CURVE('',#4647,#4648,#976,.T.);
#5795=EDGE_CURVE('',#4648,#4649,#977,.T.);
#5796=EDGE_CURVE('',#4649,#4650,#978,.T.);
#5797=EDGE_CURVE('',#4651,#4650,#3686,.T.);
#5798=EDGE_CURVE('',#4651,#4652,#979,.T.);
#5799=EDGE_CURVE('',#4652,#4653,#980,.T.);
#5800=EDGE_CURVE('',#4653,#4654,#981,.T.);
#5801=EDGE_CURVE('',#4655,#4654,#3687,.T.);
#5802=EDGE_CURVE('',#4655,#4656,#982,.T.);
#5803=EDGE_CURVE('',#4656,#4657,#983,.T.);
#5804=EDGE_CURVE('',#4657,#4658,#984,.T.);
#5805=EDGE_CURVE('',#4659,#4658,#3688,.T.);
#5806=EDGE_CURVE('',#4659,#4660,#985,.T.);
#5807=EDGE_CURVE('',#4660,#4661,#986,.T.);
#5808=EDGE_CURVE('',#4661,#4662,#987,.T.);
#5809=EDGE_CURVE('',#4663,#4662,#3689,.T.);
#5810=EDGE_CURVE('',#4663,#4664,#988,.T.);
#5811=EDGE_CURVE('',#4664,#4665,#989,.T.);
#5812=EDGE_CURVE('',#4665,#4666,#990,.T.);
#5813=EDGE_CURVE('',#4667,#4666,#3690,.T.);
#5814=EDGE_CURVE('',#4667,#4668,#991,.T.);
#5815=EDGE_CURVE('',#4668,#4669,#992,.T.);
#5816=EDGE_CURVE('',#4669,#4670,#2992,.T.);
#5817=EDGE_CURVE('',#4670,#4670,#3691,.T.);
#5818=EDGE_CURVE('',#4669,#4671,#993,.T.);
#5819=EDGE_CURVE('',#4671,#4672,#994,.T.);
#5820=EDGE_CURVE('',#4673,#4672,#3692,.T.);
#5821=EDGE_CURVE('',#4673,#4674,#995,.T.);
#5822=EDGE_CURVE('',#4674,#4675,#996,.T.);
#5823=EDGE_CURVE('',#4675,#4676,#997,.T.);
#5824=EDGE_CURVE('',#4677,#4676,#3693,.T.);
#5825=EDGE_CURVE('',#4677,#4678,#998,.T.);
#5826=EDGE_CURVE('',#4678,#4679,#999,.T.);
#5827=EDGE_CURVE('',#4679,#4680,#1000,.T.);
#5828=EDGE_CURVE('',#4681,#4680,#3694,.T.);
#5829=EDGE_CURVE('',#4681,#4682,#1001,.T.);
#5830=EDGE_CURVE('',#4682,#4683,#1002,.T.);
#5831=EDGE_CURVE('',#4683,#4684,#1003,.T.);
#5832=EDGE_CURVE('',#4685,#4684,#3695,.T.);
#5833=EDGE_CURVE('',#4685,#4686,#1004,.T.);
#5834=EDGE_CURVE('',#4686,#4687,#1005,.T.);
#5835=EDGE_CURVE('',#4687,#4688,#1006,.T.);
#5836=EDGE_CURVE('',#4689,#4688,#3696,.T.);
#5837=EDGE_CURVE('',#4689,#4690,#1007,.T.);
#5838=EDGE_CURVE('',#4690,#4691,#1008,.T.);
#5839=EDGE_CURVE('',#4691,#4692,#1009,.T.);
#5840=EDGE_CURVE('',#4693,#4692,#3697,.T.);
#5841=EDGE_CURVE('',#4693,#4694,#1010,.T.);
#5842=EDGE_CURVE('',#4694,#4695,#1011,.T.);
#5843=EDGE_CURVE('',#4695,#4696,#1012,.T.);
#5844=EDGE_CURVE('',#4697,#4696,#3698,.T.);
#5845=EDGE_CURVE('',#4697,#4698,#1013,.T.);
#5846=EDGE_CURVE('',#4698,#4699,#1014,.T.);
#5847=EDGE_CURVE('',#4699,#4700,#1015,.T.);
#5848=EDGE_CURVE('',#4701,#4700,#3699,.T.);
#5849=EDGE_CURVE('',#4701,#4702,#1016,.T.);
#5850=EDGE_CURVE('',#4702,#4703,#1017,.T.);
#5851=EDGE_CURVE('',#4703,#4704,#1018,.T.);
#5852=EDGE_CURVE('',#4705,#4704,#3700,.T.);
#5853=EDGE_CURVE('',#4705,#4706,#1019,.T.);
#5854=EDGE_CURVE('',#4706,#4707,#1020,.T.);
#5855=EDGE_CURVE('',#4707,#4708,#1021,.T.);
#5856=EDGE_CURVE('',#4709,#4708,#3701,.T.);
#5857=EDGE_CURVE('',#4709,#4710,#1022,.T.);
#5858=EDGE_CURVE('',#4710,#4711,#1023,.T.);
#5859=EDGE_CURVE('',#4711,#4712,#1024,.T.);
#5860=EDGE_CURVE('',#4713,#4712,#3702,.T.);
#5861=EDGE_CURVE('',#4713,#4714,#1025,.T.);
#5862=EDGE_CURVE('',#4714,#4715,#1026,.T.);
#5863=EDGE_CURVE('',#4715,#4716,#1027,.T.);
#5864=EDGE_CURVE('',#4717,#4716,#3703,.T.);
#5865=EDGE_CURVE('',#4717,#4718,#1028,.T.);
#5866=EDGE_CURVE('',#4718,#4719,#1029,.T.);
#5867=EDGE_CURVE('',#4719,#4720,#1030,.T.);
#5868=EDGE_CURVE('',#4721,#4720,#3704,.T.);
#5869=EDGE_CURVE('',#4721,#4722,#1031,.T.);
#5870=EDGE_CURVE('',#4722,#4723,#1032,.T.);
#5871=EDGE_CURVE('',#4723,#4724,#1033,.T.);
#5872=EDGE_CURVE('',#4725,#4724,#3705,.T.);
#5873=EDGE_CURVE('',#4725,#4726,#1034,.T.);
#5874=EDGE_CURVE('',#4726,#4727,#1035,.T.);
#5875=EDGE_CURVE('',#4727,#4728,#1036,.T.);
#5876=EDGE_CURVE('',#4729,#4728,#3706,.T.);
#5877=EDGE_CURVE('',#4729,#4730,#1037,.T.);
#5878=EDGE_CURVE('',#4730,#4731,#1038,.T.);
#5879=EDGE_CURVE('',#4731,#4732,#1039,.T.);
#5880=EDGE_CURVE('',#4733,#4732,#3707,.T.);
#5881=EDGE_CURVE('',#4733,#4734,#1040,.T.);
#5882=EDGE_CURVE('',#4734,#4735,#1041,.T.);
#5883=EDGE_CURVE('',#4735,#4736,#1042,.T.);
#5884=EDGE_CURVE('',#4737,#4736,#3708,.T.);
#5885=EDGE_CURVE('',#4737,#4738,#1043,.T.);
#5886=EDGE_CURVE('',#4738,#4739,#1044,.T.);
#5887=EDGE_CURVE('',#4739,#4740,#1045,.T.);
#5888=EDGE_CURVE('',#4741,#4740,#3709,.T.);
#5889=EDGE_CURVE('',#4741,#4742,#1046,.T.);
#5890=EDGE_CURVE('',#4742,#4743,#1047,.T.);
#5891=EDGE_CURVE('',#4743,#4744,#1048,.T.);
#5892=EDGE_CURVE('',#4745,#4744,#3710,.T.);
#5893=EDGE_CURVE('',#4745,#4746,#1049,.T.);
#5894=EDGE_CURVE('',#4746,#4747,#1050,.T.);
#5895=EDGE_CURVE('',#4747,#4748,#1051,.T.);
#5896=EDGE_CURVE('',#4749,#4748,#3711,.T.);
#5897=EDGE_CURVE('',#4749,#4750,#1052,.T.);
#5898=EDGE_CURVE('',#4750,#4751,#1053,.T.);
#5899=EDGE_CURVE('',#4751,#4752,#1054,.T.);
#5900=EDGE_CURVE('',#4753,#4752,#3712,.T.);
#5901=EDGE_CURVE('',#4753,#4754,#1055,.T.);
#5902=EDGE_CURVE('',#4754,#4755,#1056,.T.);
#5903=EDGE_CURVE('',#4755,#4756,#1057,.T.);
#5904=EDGE_CURVE('',#4757,#4756,#3713,.T.);
#5905=EDGE_CURVE('',#4757,#4580,#1058,.T.);
#5906=EDGE_CURVE('',#4619,#4394,#1059,.T.);
#5907=EDGE_CURVE('',#4395,#4618,#1060,.T.);
#5908=EDGE_CURVE('',#4389,#4622,#1061,.T.);
#5909=EDGE_CURVE('',#4623,#4388,#1062,.T.);
#5910=EDGE_CURVE('',#4615,#4382,#1063,.T.);
#5911=EDGE_CURVE('',#4383,#4614,#1064,.T.);
#5912=EDGE_CURVE('',#4611,#4376,#1065,.T.);
#5913=EDGE_CURVE('',#4377,#4610,#1066,.T.);
#5914=EDGE_CURVE('',#4607,#4370,#1067,.T.);
#5915=EDGE_CURVE('',#4371,#4606,#1068,.T.);
#5916=EDGE_CURVE('',#4603,#4364,#1069,.T.);
#5917=EDGE_CURVE('',#4365,#4602,#1070,.T.);
#5918=EDGE_CURVE('',#4599,#4358,#1071,.T.);
#5919=EDGE_CURVE('',#4359,#4598,#1072,.T.);
#5920=EDGE_CURVE('',#4595,#4352,#1073,.T.);
#5921=EDGE_CURVE('',#4353,#4594,#1074,.T.);
#5922=EDGE_CURVE('',#4591,#4346,#1075,.T.);
#5923=EDGE_CURVE('',#4347,#4590,#1076,.T.);
#5924=EDGE_CURVE('',#4587,#4340,#1077,.T.);
#5925=EDGE_CURVE('',#4341,#4586,#1078,.T.);
#5926=EDGE_CURVE('',#4583,#4334,#1079,.T.);
#5927=EDGE_CURVE('',#4335,#4582,#1080,.T.);
#5928=EDGE_CURVE('',#4757,#4328,#1081,.T.);
#5929=EDGE_CURVE('',#4329,#4756,#1082,.T.);
#5930=EDGE_CURVE('',#4753,#4322,#1083,.T.);
#5931=EDGE_CURVE('',#4323,#4752,#1084,.T.);
#5932=EDGE_CURVE('',#4749,#4316,#1085,.T.);
#5933=EDGE_CURVE('',#4317,#4748,#1086,.T.);
#5934=EDGE_CURVE('',#4745,#4310,#1087,.T.);
#5935=EDGE_CURVE('',#4311,#4744,#1088,.T.);
#5936=EDGE_CURVE('',#4741,#4304,#1089,.T.);
#5937=EDGE_CURVE('',#4305,#4740,#1090,.T.);
#5938=EDGE_CURVE('',#4737,#4298,#1091,.T.);
#5939=EDGE_CURVE('',#4299,#4736,#1092,.T.);
#5940=EDGE_CURVE('',#4733,#4292,#1093,.T.);
#5941=EDGE_CURVE('',#4293,#4732,#1094,.T.);
#5942=EDGE_CURVE('',#4729,#4286,#1095,.T.);
#5943=EDGE_CURVE('',#4287,#4728,#1096,.T.);
#5944=EDGE_CURVE('',#4725,#4280,#1097,.T.);
#5945=EDGE_CURVE('',#4281,#4724,#1098,.T.);
#5946=EDGE_CURVE('',#4721,#4274,#1099,.T.);
#5947=EDGE_CURVE('',#4275,#4720,#1100,.T.);
#5948=EDGE_CURVE('',#4717,#4268,#1101,.T.);
#5949=EDGE_CURVE('',#4269,#4716,#1102,.T.);
#5950=EDGE_CURVE('',#4713,#4262,#1103,.T.);
#5951=EDGE_CURVE('',#4263,#4712,#1104,.T.);
#5952=EDGE_CURVE('',#4709,#4256,#1105,.T.);
#5953=EDGE_CURVE('',#4257,#4708,#1106,.T.);
#5954=EDGE_CURVE('',#4705,#4250,#1107,.T.);
#5955=EDGE_CURVE('',#4251,#4704,#1108,.T.);
#5956=EDGE_CURVE('',#4701,#4244,#1109,.T.);
#5957=EDGE_CURVE('',#4245,#4700,#1110,.T.);
#5958=EDGE_CURVE('',#4697,#4238,#1111,.T.);
#5959=EDGE_CURVE('',#4239,#4696,#1112,.T.);
#5960=EDGE_CURVE('',#4693,#4232,#1113,.T.);
#5961=EDGE_CURVE('',#4233,#4692,#1114,.T.);
#5962=EDGE_CURVE('',#4689,#4226,#1115,.T.);
#5963=EDGE_CURVE('',#4227,#4688,#1116,.T.);
#5964=EDGE_CURVE('',#4685,#4220,#1117,.T.);
#5965=EDGE_CURVE('',#4221,#4684,#1118,.T.);
#5966=EDGE_CURVE('',#4681,#4214,#1119,.T.);
#5967=EDGE_CURVE('',#4215,#4680,#1120,.T.);
#5968=EDGE_CURVE('',#4677,#4208,#1121,.T.);
#5969=EDGE_CURVE('',#4209,#4676,#1122,.T.);
#5970=EDGE_CURVE('',#4673,#4202,#1123,.T.);
#5971=EDGE_CURVE('',#4203,#4672,#1124,.T.);
#5972=EDGE_CURVE('',#4667,#4196,#1125,.T.);
#5973=EDGE_CURVE('',#4197,#4666,#1126,.T.);
#5974=EDGE_CURVE('',#4663,#4190,#1127,.T.);
#5975=EDGE_CURVE('',#4191,#4662,#1128,.T.);
#5976=EDGE_CURVE('',#4659,#4184,#1129,.T.);
#5977=EDGE_CURVE('',#4185,#4658,#1130,.T.);
#5978=EDGE_CURVE('',#4655,#4178,#1131,.T.);
#5979=EDGE_CURVE('',#4179,#4654,#1132,.T.);
#5980=EDGE_CURVE('',#4651,#4172,#1133,.T.);
#5981=EDGE_CURVE('',#4173,#4650,#1134,.T.);
#5982=EDGE_CURVE('',#4647,#4166,#1135,.T.);
#5983=EDGE_CURVE('',#4167,#4646,#1136,.T.);
#5984=EDGE_CURVE('',#4643,#4160,#1137,.T.);
#5985=EDGE_CURVE('',#4161,#4642,#1138,.T.);
#5986=EDGE_CURVE('',#4639,#4154,#1139,.T.);
#5987=EDGE_CURVE('',#4155,#4638,#1140,.T.);
#5988=EDGE_CURVE('',#4635,#4148,#1141,.T.);
#5989=EDGE_CURVE('',#4149,#4634,#1142,.T.);
#5990=EDGE_CURVE('',#4631,#4142,#1143,.T.);
#5991=EDGE_CURVE('',#4143,#4630,#1144,.T.);
#5992=EDGE_CURVE('',#4627,#4136,#1145,.T.);
#5993=EDGE_CURVE('',#4137,#4626,#1146,.T.);
#5994=EDGE_CURVE('',#4391,#4445,#1147,.T.);
#5995=EDGE_CURVE('',#4444,#4386,#1148,.T.);
#5996=EDGE_CURVE('',#4448,#4392,#1149,.T.);
#5997=EDGE_CURVE('',#4397,#4449,#1150,.T.);
#5998=EDGE_CURVE('',#4452,#4380,#1151,.T.);
#5999=EDGE_CURVE('',#4385,#4453,#1152,.T.);
#6000=EDGE_CURVE('',#4456,#4374,#1153,.T.);
#6001=EDGE_CURVE('',#4379,#4457,#1154,.T.);
#6002=EDGE_CURVE('',#4460,#4368,#1155,.T.);
#6003=EDGE_CURVE('',#4373,#4461,#1156,.T.);
#6004=EDGE_CURVE('',#4464,#4362,#1157,.T.);
#6005=EDGE_CURVE('',#4367,#4465,#1158,.T.);
#6006=EDGE_CURVE('',#4472,#4350,#1159,.T.);
#6007=EDGE_CURVE('',#4355,#4473,#1160,.T.);
#6008=EDGE_CURVE('',#4468,#4356,#1161,.T.);
#6009=EDGE_CURVE('',#4361,#4469,#1162,.T.);
#6010=EDGE_CURVE('',#4476,#4344,#1163,.T.);
#6011=EDGE_CURVE('',#4349,#4477,#1164,.T.);
#6012=EDGE_CURVE('',#4480,#4338,#1165,.T.);
#6013=EDGE_CURVE('',#4343,#4481,#1166,.T.);
#6014=EDGE_CURVE('',#4484,#4332,#1167,.T.);
#6015=EDGE_CURVE('',#4337,#4485,#1168,.T.);
#6016=EDGE_CURVE('',#4490,#4326,#1169,.T.);
#6017=EDGE_CURVE('',#4331,#4491,#1170,.T.);
#6018=EDGE_CURVE('',#4494,#4320,#1171,.T.);
#6019=EDGE_CURVE('',#4325,#4495,#1172,.T.);
#6020=EDGE_CURVE('',#4498,#4314,#1173,.T.);
#6021=EDGE_CURVE('',#4319,#4499,#1174,.T.);
#6022=EDGE_CURVE('',#4502,#4308,#1175,.T.);
#6023=EDGE_CURVE('',#4313,#4503,#1176,.T.);
#6024=EDGE_CURVE('',#4506,#4302,#1177,.T.);
#6025=EDGE_CURVE('',#4307,#4507,#1178,.T.);
#6026=EDGE_CURVE('',#4510,#4296,#1179,.T.);
#6027=EDGE_CURVE('',#4301,#4511,#1180,.T.);
#6028=EDGE_CURVE('',#4514,#4290,#1181,.T.);
#6029=EDGE_CURVE('',#4295,#4515,#1182,.T.);
#6030=EDGE_CURVE('',#4518,#4284,#1183,.T.);
#6031=EDGE_CURVE('',#4289,#4519,#1184,.T.);
#6032=EDGE_CURVE('',#4522,#4278,#1185,.T.);
#6033=EDGE_CURVE('',#4283,#4523,#1186,.T.);
#6034=EDGE_CURVE('',#4526,#4272,#1187,.T.);
#6035=EDGE_CURVE('',#4277,#4527,#1188,.T.);
#6036=EDGE_CURVE('',#4530,#4266,#1189,.T.);
#6037=EDGE_CURVE('',#4271,#4531,#1190,.T.);
#6038=EDGE_CURVE('',#4534,#4260,#1191,.T.);
#6039=EDGE_CURVE('',#4265,#4535,#1192,.T.);
#6040=EDGE_CURVE('',#4538,#4254,#1193,.T.);
#6041=EDGE_CURVE('',#4259,#4539,#1194,.T.);
#6042=EDGE_CURVE('',#4542,#4248,#1195,.T.);
#6043=EDGE_CURVE('',#4253,#4543,#1196,.T.);
#6044=EDGE_CURVE('',#4546,#4242,#1197,.T.);
#6045=EDGE_CURVE('',#4247,#4547,#1198,.T.);
#6046=EDGE_CURVE('',#4550,#4236,#1199,.T.);
#6047=EDGE_CURVE('',#4241,#4551,#1200,.T.);
#6048=EDGE_CURVE('',#4554,#4230,#1201,.T.);
#6049=EDGE_CURVE('',#4235,#4555,#1202,.T.);
#6050=EDGE_CURVE('',#4562,#4218,#1203,.T.);
#6051=EDGE_CURVE('',#4223,#4563,#1204,.T.);
#6052=EDGE_CURVE('',#4558,#4224,#1205,.T.);
#6053=EDGE_CURVE('',#4229,#4559,#1206,.T.);
#6054=EDGE_CURVE('',#4566,#4212,#1207,.T.);
#6055=EDGE_CURVE('',#4217,#4567,#1208,.T.);
#6056=EDGE_CURVE('',#4570,#4206,#1209,.T.);
#6057=EDGE_CURVE('',#4211,#4571,#1210,.T.);
#6058=EDGE_CURVE('',#4574,#4200,#1211,.T.);
#6059=EDGE_CURVE('',#4205,#4575,#1212,.T.);
#6060=EDGE_CURVE('',#4400,#4194,#1213,.T.);
#6061=EDGE_CURVE('',#4199,#4401,#1214,.T.);
#6062=EDGE_CURVE('',#4404,#4188,#1215,.T.);
#6063=EDGE_CURVE('',#4193,#4405,#1216,.T.);
#6064=EDGE_CURVE('',#4408,#4182,#1217,.T.);
#6065=EDGE_CURVE('',#4187,#4409,#1218,.T.);
#6066=EDGE_CURVE('',#4412,#4176,#1219,.T.);
#6067=EDGE_CURVE('',#4181,#4413,#1220,.T.);
#6068=EDGE_CURVE('',#4416,#4170,#1221,.T.);
#6069=EDGE_CURVE('',#4175,#4417,#1222,.T.);
#6070=EDGE_CURVE('',#4420,#4164,#1223,.T.);
#6071=EDGE_CURVE('',#4169,#4421,#1224,.T.);
#6072=EDGE_CURVE('',#4424,#4158,#1225,.T.);
#6073=EDGE_CURVE('',#4163,#4425,#1226,.T.);
#6074=EDGE_CURVE('',#4428,#4152,#1227,.T.);
#6075=EDGE_CURVE('',#4157,#4429,#1228,.T.);
#6076=EDGE_CURVE('',#4432,#4146,#1229,.T.);
#6077=EDGE_CURVE('',#4151,#4433,#1230,.T.);
#6078=EDGE_CURVE('',#4436,#4140,#1231,.T.);
#6079=EDGE_CURVE('',#4145,#4437,#1232,.T.);
#6080=EDGE_CURVE('',#4440,#4134,#1233,.T.);
#6081=EDGE_CURVE('',#4139,#4441,#1234,.T.);
#6082=EDGE_CURVE('',#4758,#4576,#2993,.T.);
#6083=EDGE_CURVE('',#4758,#4759,#2994,.T.);
#6084=EDGE_CURVE('',#4759,#4577,#2995,.T.);
#6085=EDGE_CURVE('',#4760,#4579,#2996,.T.);
#6086=EDGE_CURVE('',#4761,#4578,#2997,.T.);
#6087=EDGE_CURVE('',#4760,#4761,#2998,.T.);
#6088=EDGE_CURVE('',#4758,#4760,#2999,.T.);
#6089=EDGE_CURVE('',#4759,#4761,#3000,.T.);
#6090=EDGE_CURVE('',#4762,#4442,#1235,.T.);
#6091=EDGE_CURVE('',#4763,#4762,#3714,.T.);
#6092=EDGE_CURVE('',#4764,#4763,#3715,.T.);
#6093=EDGE_CURVE('',#4764,#4443,#232,.T.);
#6094=EDGE_CURVE('',#4387,#4764,#3716,.T.);
#6095=EDGE_CURVE('',#4762,#4138,#3717,.T.);
#6096=EDGE_CURVE('',#4764,#4624,#1236,.T.);
#6097=EDGE_CURVE('',#4762,#4625,#233,.T.);
#6098=EDGE_CURVE('',#4765,#4144,#3718,.T.);
#6099=EDGE_CURVE('',#4765,#4438,#1237,.T.);
#6100=EDGE_CURVE('',#4766,#4439,#234,.T.);
#6101=EDGE_CURVE('',#4135,#4766,#3719,.T.);
#6102=EDGE_CURVE('',#4767,#4765,#3720,.T.);
#6103=EDGE_CURVE('',#4766,#4767,#3721,.T.);
#6104=EDGE_CURVE('',#4768,#4150,#3722,.T.);
#6105=EDGE_CURVE('',#4768,#4434,#1238,.T.);
#6106=EDGE_CURVE('',#4769,#4435,#235,.T.);
#6107=EDGE_CURVE('',#4141,#4769,#3723,.T.);
#6108=EDGE_CURVE('',#4770,#4768,#3724,.T.);
#6109=EDGE_CURVE('',#4769,#4770,#3725,.T.);
#6110=EDGE_CURVE('',#4771,#4156,#3726,.T.);
#6111=EDGE_CURVE('',#4771,#4430,#236,.T.);
#6112=EDGE_CURVE('',#4772,#4431,#237,.T.);
#6113=EDGE_CURVE('',#4147,#4772,#3727,.T.);
#6114=EDGE_CURVE('',#4773,#4771,#3728,.T.);
#6115=EDGE_CURVE('',#4772,#4773,#3729,.T.);
#6116=EDGE_CURVE('',#4774,#4162,#3730,.T.);
#6117=EDGE_CURVE('',#4774,#4426,#1239,.T.);
#6118=EDGE_CURVE('',#4775,#4427,#238,.T.);
#6119=EDGE_CURVE('',#4153,#4775,#3731,.T.);
#6120=EDGE_CURVE('',#4776,#4774,#3732,.T.);
#6121=EDGE_CURVE('',#4775,#4776,#3733,.T.);
#6122=EDGE_CURVE('',#4777,#4168,#3734,.T.);
#6123=EDGE_CURVE('',#4777,#4422,#1240,.T.);
#6124=EDGE_CURVE('',#4778,#4423,#239,.T.);
#6125=EDGE_CURVE('',#4159,#4778,#3735,.T.);
#6126=EDGE_CURVE('',#4779,#4777,#3736,.T.);
#6127=EDGE_CURVE('',#4778,#4779,#3737,.T.);
#6128=EDGE_CURVE('',#4780,#4174,#3738,.T.);
#6129=EDGE_CURVE('',#4780,#4418,#1241,.T.);
#6130=EDGE_CURVE('',#4781,#4419,#240,.T.);
#6131=EDGE_CURVE('',#4165,#4781,#3739,.T.);
#6132=EDGE_CURVE('',#4782,#4780,#3740,.T.);
#6133=EDGE_CURVE('',#4781,#4782,#3741,.T.);
#6134=EDGE_CURVE('',#4783,#4180,#3742,.T.);
#6135=EDGE_CURVE('',#4783,#4414,#1242,.T.);
#6136=EDGE_CURVE('',#4784,#4415,#241,.T.);
#6137=EDGE_CURVE('',#4171,#4784,#3743,.T.);
#6138=EDGE_CURVE('',#4785,#4783,#3744,.T.);
#6139=EDGE_CURVE('',#4784,#4785,#3745,.T.);
#6140=EDGE_CURVE('',#4786,#4186,#3746,.T.);
#6141=EDGE_CURVE('',#4786,#4410,#1243,.T.);
#6142=EDGE_CURVE('',#4787,#4411,#242,.T.);
#6143=EDGE_CURVE('',#4177,#4787,#3747,.T.);
#6144=EDGE_CURVE('',#4788,#4786,#3748,.T.);
#6145=EDGE_CURVE('',#4787,#4788,#3749,.T.);
#6146=EDGE_CURVE('',#4789,#4192,#3750,.T.);
#6147=EDGE_CURVE('',#4789,#4406,#1244,.T.);
#6148=EDGE_CURVE('',#4790,#4407,#243,.T.);
#6149=EDGE_CURVE('',#4183,#4790,#3751,.T.);
#6150=EDGE_CURVE('',#4791,#4789,#3752,.T.);
#6151=EDGE_CURVE('',#4790,#4791,#3753,.T.);
#6152=EDGE_CURVE('',#4792,#4198,#3754,.T.);
#6153=EDGE_CURVE('',#4792,#4402,#1245,.T.);
#6154=EDGE_CURVE('',#4793,#4403,#244,.T.);
#6155=EDGE_CURVE('',#4189,#4793,#3755,.T.);
#6156=EDGE_CURVE('',#4794,#4792,#3756,.T.);
#6157=EDGE_CURVE('',#4793,#4794,#3757,.T.);
#6158=EDGE_CURVE('',#4795,#4204,#3758,.T.);
#6159=EDGE_CURVE('',#4795,#4399,#1246,.T.);
#6160=EDGE_CURVE('',#4796,#4398,#245,.T.);
#6161=EDGE_CURVE('',#4195,#4796,#3759,.T.);
#6162=EDGE_CURVE('',#4797,#4795,#3760,.T.);
#6163=EDGE_CURVE('',#4796,#4797,#3761,.T.);
#6164=EDGE_CURVE('',#4798,#4210,#3762,.T.);
#6165=EDGE_CURVE('',#4798,#4572,#246,.T.);
#6166=EDGE_CURVE('',#4799,#4573,#247,.T.);
#6167=EDGE_CURVE('',#4201,#4799,#3763,.T.);
#6168=EDGE_CURVE('',#4800,#4798,#3764,.T.);
#6169=EDGE_CURVE('',#4799,#4800,#3765,.T.);
#6170=EDGE_CURVE('',#4801,#4216,#3766,.T.);
#6171=EDGE_CURVE('',#4801,#4568,#1247,.T.);
#6172=EDGE_CURVE('',#4802,#4569,#248,.T.);
#6173=EDGE_CURVE('',#4207,#4802,#3767,.T.);
#6174=EDGE_CURVE('',#4803,#4801,#3768,.T.);
#6175=EDGE_CURVE('',#4802,#4803,#3769,.T.);
#6176=EDGE_CURVE('',#4804,#4222,#3770,.T.);
#6177=EDGE_CURVE('',#4804,#4564,#1248,.T.);
#6178=EDGE_CURVE('',#4805,#4565,#249,.T.);
#6179=EDGE_CURVE('',#4213,#4805,#3771,.T.);
#6180=EDGE_CURVE('',#4806,#4804,#3772,.T.);
#6181=EDGE_CURVE('',#4805,#4806,#3773,.T.);
#6182=EDGE_CURVE('',#4807,#4561,#250,.T.);
#6183=EDGE_CURVE('',#4219,#4807,#3774,.T.);
#6184=EDGE_CURVE('',#4808,#4228,#3775,.T.);
#6185=EDGE_CURVE('',#4808,#4560,#251,.T.);
#6186=EDGE_CURVE('',#4809,#4808,#3776,.T.);
#6187=EDGE_CURVE('',#4807,#4809,#3777,.T.);
#6188=EDGE_CURVE('',#4810,#4234,#3778,.T.);
#6189=EDGE_CURVE('',#4810,#4556,#1249,.T.);
#6190=EDGE_CURVE('',#4811,#4557,#252,.T.);
#6191=EDGE_CURVE('',#4225,#4811,#3779,.T.);
#6192=EDGE_CURVE('',#4812,#4810,#3780,.T.);
#6193=EDGE_CURVE('',#4811,#4812,#3781,.T.);
#6194=EDGE_CURVE('',#4813,#4240,#3782,.T.);
#6195=EDGE_CURVE('',#4813,#4552,#1250,.T.);
#6196=EDGE_CURVE('',#4814,#4553,#253,.T.);
#6197=EDGE_CURVE('',#4231,#4814,#3783,.T.);
#6198=EDGE_CURVE('',#4815,#4813,#3784,.T.);
#6199=EDGE_CURVE('',#4814,#4815,#3785,.T.);
#6200=EDGE_CURVE('',#4816,#4246,#3786,.T.);
#6201=EDGE_CURVE('',#4816,#4548,#1251,.T.);
#6202=EDGE_CURVE('',#4817,#4549,#254,.T.);
#6203=EDGE_CURVE('',#4237,#4817,#3787,.T.);
#6204=EDGE_CURVE('',#4818,#4816,#3788,.T.);
#6205=EDGE_CURVE('',#4817,#4818,#3789,.T.);
#6206=EDGE_CURVE('',#4819,#4252,#3790,.T.);
#6207=EDGE_CURVE('',#4819,#4544,#1252,.T.);
#6208=EDGE_CURVE('',#4820,#4545,#255,.T.);
#6209=EDGE_CURVE('',#4243,#4820,#3791,.T.);
#6210=EDGE_CURVE('',#4821,#4819,#3792,.T.);
#6211=EDGE_CURVE('',#4820,#4821,#3793,.T.);
#6212=EDGE_CURVE('',#4822,#4258,#3794,.T.);
#6213=EDGE_CURVE('',#4822,#4540,#1253,.T.);
#6214=EDGE_CURVE('',#4823,#4541,#256,.T.);
#6215=EDGE_CURVE('',#4249,#4823,#3795,.T.);
#6216=EDGE_CURVE('',#4824,#4822,#3796,.T.);
#6217=EDGE_CURVE('',#4823,#4824,#3797,.T.);
#6218=EDGE_CURVE('',#4825,#4264,#3798,.T.);
#6219=EDGE_CURVE('',#4825,#4536,#1254,.T.);
#6220=EDGE_CURVE('',#4826,#4537,#257,.T.);
#6221=EDGE_CURVE('',#4255,#4826,#3799,.T.);
#6222=EDGE_CURVE('',#4827,#4825,#3800,.T.);
#6223=EDGE_CURVE('',#4826,#4827,#3801,.T.);
#6224=EDGE_CURVE('',#4828,#4270,#3802,.T.);
#6225=EDGE_CURVE('',#4828,#4532,#1255,.T.);
#6226=EDGE_CURVE('',#4829,#4533,#258,.T.);
#6227=EDGE_CURVE('',#4261,#4829,#3803,.T.);
#6228=EDGE_CURVE('',#4830,#4828,#3804,.T.);
#6229=EDGE_CURVE('',#4829,#4830,#3805,.T.);
#6230=EDGE_CURVE('',#4831,#4276,#3806,.T.);
#6231=EDGE_CURVE('',#4831,#4528,#1256,.T.);
#6232=EDGE_CURVE('',#4832,#4529,#259,.T.);
#6233=EDGE_CURVE('',#4267,#4832,#3807,.T.);
#6234=EDGE_CURVE('',#4833,#4831,#3808,.T.);
#6235=EDGE_CURVE('',#4832,#4833,#3809,.T.);
#6236=EDGE_CURVE('',#4834,#4282,#3810,.T.);
#6237=EDGE_CURVE('',#4834,#4524,#1257,.T.);
#6238=EDGE_CURVE('',#4835,#4525,#260,.T.);
#6239=EDGE_CURVE('',#4273,#4835,#3811,.T.);
#6240=EDGE_CURVE('',#4836,#4834,#3812,.T.);
#6241=EDGE_CURVE('',#4835,#4836,#3813,.T.);
#6242=EDGE_CURVE('',#4837,#4288,#3814,.T.);
#6243=EDGE_CURVE('',#4837,#4520,#261,.T.);
#6244=EDGE_CURVE('',#4838,#4521,#262,.T.);
#6245=EDGE_CURVE('',#4279,#4838,#3815,.T.);
#6246=EDGE_CURVE('',#4839,#4837,#3816,.T.);
#6247=EDGE_CURVE('',#4838,#4839,#3817,.T.);
#6248=EDGE_CURVE('',#4840,#4294,#3818,.T.);
#6249=EDGE_CURVE('',#4840,#4516,#263,.T.);
#6250=EDGE_CURVE('',#4841,#4517,#264,.T.);
#6251=EDGE_CURVE('',#4285,#4841,#3819,.T.);
#6252=EDGE_CURVE('',#4842,#4840,#3820,.T.);
#6253=EDGE_CURVE('',#4841,#4842,#3821,.T.);
#6254=EDGE_CURVE('',#4843,#4300,#3822,.T.);
#6255=EDGE_CURVE('',#4843,#4512,#1258,.T.);
#6256=EDGE_CURVE('',#4844,#4513,#265,.T.);
#6257=EDGE_CURVE('',#4291,#4844,#3823,.T.);
#6258=EDGE_CURVE('',#4845,#4843,#3824,.T.);
#6259=EDGE_CURVE('',#4844,#4845,#3825,.T.);
#6260=EDGE_CURVE('',#4846,#4306,#3826,.T.);
#6261=EDGE_CURVE('',#4846,#4508,#1259,.T.);
#6262=EDGE_CURVE('',#4847,#4509,#266,.T.);
#6263=EDGE_CURVE('',#4297,#4847,#3827,.T.);
#6264=EDGE_CURVE('',#4848,#4846,#3828,.T.);
#6265=EDGE_CURVE('',#4847,#4848,#3829,.T.);
#6266=EDGE_CURVE('',#4849,#4312,#3830,.T.);
#6267=EDGE_CURVE('',#4849,#4504,#1260,.T.);
#6268=EDGE_CURVE('',#4850,#4505,#267,.T.);
#6269=EDGE_CURVE('',#4303,#4850,#3831,.T.);
#6270=EDGE_CURVE('',#4851,#4849,#3832,.T.);
#6271=EDGE_CURVE('',#4850,#4851,#3833,.T.);
#6272=EDGE_CURVE('',#4852,#4318,#3834,.T.);
#6273=EDGE_CURVE('',#4852,#4500,#1261,.T.);
#6274=EDGE_CURVE('',#4853,#4501,#268,.T.);
#6275=EDGE_CURVE('',#4309,#4853,#3835,.T.);
#6276=EDGE_CURVE('',#4854,#4852,#3836,.T.);
#6277=EDGE_CURVE('',#4853,#4854,#3837,.T.);
#6278=EDGE_CURVE('',#4855,#4324,#3838,.T.);
#6279=EDGE_CURVE('',#4855,#4496,#1262,.T.);
#6280=EDGE_CURVE('',#4856,#4497,#269,.T.);
#6281=EDGE_CURVE('',#4315,#4856,#3839,.T.);
#6282=EDGE_CURVE('',#4857,#4855,#3840,.T.);
#6283=EDGE_CURVE('',#4856,#4857,#3841,.T.);
#6284=EDGE_CURVE('',#4858,#4330,#3842,.T.);
#6285=EDGE_CURVE('',#4858,#4492,#1263,.T.);
#6286=EDGE_CURVE('',#4859,#4493,#270,.T.);
#6287=EDGE_CURVE('',#4321,#4859,#3843,.T.);
#6288=EDGE_CURVE('',#4860,#4858,#3844,.T.);
#6289=EDGE_CURVE('',#4859,#4860,#3845,.T.);
#6290=EDGE_CURVE('',#4861,#4336,#3846,.T.);
#6291=EDGE_CURVE('',#4861,#4486,#271,.T.);
#6292=EDGE_CURVE('',#4862,#4489,#272,.T.);
#6293=EDGE_CURVE('',#4327,#4862,#3847,.T.);
#6294=EDGE_CURVE('',#4863,#4861,#3848,.T.);
#6295=EDGE_CURVE('',#4862,#4863,#3849,.T.);
#6296=EDGE_CURVE('',#4864,#4342,#3850,.T.);
#6297=EDGE_CURVE('',#4864,#4482,#273,.T.);
#6298=EDGE_CURVE('',#4865,#4483,#274,.T.);
#6299=EDGE_CURVE('',#4333,#4865,#3851,.T.);
#6300=EDGE_CURVE('',#4866,#4864,#3852,.T.);
#6301=EDGE_CURVE('',#4865,#4866,#3853,.T.);
#6302=EDGE_CURVE('',#4867,#4348,#3854,.T.);
#6303=EDGE_CURVE('',#4867,#4478,#1264,.T.);
#6304=EDGE_CURVE('',#4868,#4479,#275,.T.);
#6305=EDGE_CURVE('',#4339,#4868,#3855,.T.);
#6306=EDGE_CURVE('',#4869,#4867,#3856,.T.);
#6307=EDGE_CURVE('',#4868,#4869,#3857,.T.);
#6308=EDGE_CURVE('',#4870,#4354,#3858,.T.);
#6309=EDGE_CURVE('',#4870,#4474,#1265,.T.);
#6310=EDGE_CURVE('',#4871,#4475,#276,.T.);
#6311=EDGE_CURVE('',#4345,#4871,#3859,.T.);
#6312=EDGE_CURVE('',#4872,#4870,#3860,.T.);
#6313=EDGE_CURVE('',#4871,#4872,#3861,.T.);
#6314=EDGE_CURVE('',#4873,#4471,#277,.T.);
#6315=EDGE_CURVE('',#4351,#4873,#3862,.T.);
#6316=EDGE_CURVE('',#4874,#4360,#3863,.T.);
#6317=EDGE_CURVE('',#4874,#4470,#278,.T.);
#6318=EDGE_CURVE('',#4875,#4874,#3864,.T.);
#6319=EDGE_CURVE('',#4873,#4875,#3865,.T.);
#6320=EDGE_CURVE('',#4876,#4366,#3866,.T.);
#6321=EDGE_CURVE('',#4876,#4466,#1266,.T.);
#6322=EDGE_CURVE('',#4877,#4467,#279,.T.);
#6323=EDGE_CURVE('',#4357,#4877,#3867,.T.);
#6324=EDGE_CURVE('',#4878,#4876,#3868,.T.);
#6325=EDGE_CURVE('',#4877,#4878,#3869,.T.);
#6326=EDGE_CURVE('',#4879,#4372,#3870,.T.);
#6327=EDGE_CURVE('',#4879,#4462,#1267,.T.);
#6328=EDGE_CURVE('',#4880,#4463,#280,.T.);
#6329=EDGE_CURVE('',#4363,#4880,#3871,.T.);
#6330=EDGE_CURVE('',#4881,#4879,#3872,.T.);
#6331=EDGE_CURVE('',#4880,#4881,#3873,.T.);
#6332=EDGE_CURVE('',#4882,#4378,#3874,.T.);
#6333=EDGE_CURVE('',#4882,#4458,#1268,.T.);
#6334=EDGE_CURVE('',#4883,#4459,#281,.T.);
#6335=EDGE_CURVE('',#4369,#4883,#3875,.T.);
#6336=EDGE_CURVE('',#4884,#4882,#3876,.T.);
#6337=EDGE_CURVE('',#4883,#4884,#3877,.T.);
#6338=EDGE_CURVE('',#4885,#4384,#3878,.T.);
#6339=EDGE_CURVE('',#4885,#4454,#1269,.T.);
#6340=EDGE_CURVE('',#4886,#4455,#282,.T.);
#6341=EDGE_CURVE('',#4375,#4886,#3879,.T.);
#6342=EDGE_CURVE('',#4887,#4885,#3880,.T.);
#6343=EDGE_CURVE('',#4886,#4887,#3881,.T.);
#6344=EDGE_CURVE('',#4888,#4396,#3882,.T.);
#6345=EDGE_CURVE('',#4888,#4450,#1270,.T.);
#6346=EDGE_CURVE('',#4889,#4451,#283,.T.);
#6347=EDGE_CURVE('',#4381,#4889,#3883,.T.);
#6348=EDGE_CURVE('',#4890,#4888,#3884,.T.);
#6349=EDGE_CURVE('',#4889,#4890,#3885,.T.);
#6350=EDGE_CURVE('',#4891,#4390,#3886,.T.);
#6351=EDGE_CURVE('',#4891,#4446,#284,.T.);
#6352=EDGE_CURVE('',#4892,#4447,#285,.T.);
#6353=EDGE_CURVE('',#4393,#4892,#3887,.T.);
#6354=EDGE_CURVE('',#4893,#4891,#3888,.T.);
#6355=EDGE_CURVE('',#4892,#4893,#3889,.T.);
#6356=EDGE_CURVE('',#4766,#4628,#1271,.T.);
#6357=EDGE_CURVE('',#4765,#4629,#286,.T.);
#6358=EDGE_CURVE('',#4769,#4632,#1272,.T.);
#6359=EDGE_CURVE('',#4768,#4633,#287,.T.);
#6360=EDGE_CURVE('',#4772,#4636,#1273,.T.);
#6361=EDGE_CURVE('',#4771,#4637,#1274,.T.);
#6362=EDGE_CURVE('',#4775,#4640,#1275,.T.);
#6363=EDGE_CURVE('',#4774,#4641,#288,.T.);
#6364=EDGE_CURVE('',#4778,#4644,#1276,.T.);
#6365=EDGE_CURVE('',#4777,#4645,#289,.T.);
#6366=EDGE_CURVE('',#4781,#4648,#1277,.T.);
#6367=EDGE_CURVE('',#4780,#4649,#290,.T.);
#6368=EDGE_CURVE('',#4784,#4652,#1278,.T.);
#6369=EDGE_CURVE('',#4783,#4653,#291,.T.);
#6370=EDGE_CURVE('',#4787,#4656,#1279,.T.);
#6371=EDGE_CURVE('',#4786,#4657,#292,.T.);
#6372=EDGE_CURVE('',#4790,#4660,#1280,.T.);
#6373=EDGE_CURVE('',#4789,#4661,#293,.T.);
#6374=EDGE_CURVE('',#4793,#4664,#1281,.T.);
#6375=EDGE_CURVE('',#4792,#4665,#294,.T.);
#6376=EDGE_CURVE('',#4796,#4668,#1282,.T.);
#6377=EDGE_CURVE('',#4795,#4671,#295,.T.);
#6378=EDGE_CURVE('',#4799,#4674,#1283,.T.);
#6379=EDGE_CURVE('',#4798,#4675,#1284,.T.);
#6380=EDGE_CURVE('',#4802,#4678,#1285,.T.);
#6381=EDGE_CURVE('',#4801,#4679,#296,.T.);
#6382=EDGE_CURVE('',#4805,#4682,#1286,.T.);
#6383=EDGE_CURVE('',#4804,#4683,#297,.T.);
#6384=EDGE_CURVE('',#4808,#4687,#298,.T.);
#6385=EDGE_CURVE('',#4807,#4686,#1287,.T.);
#6386=EDGE_CURVE('',#4811,#4690,#1288,.T.);
#6387=EDGE_CURVE('',#4810,#4691,#299,.T.);
#6388=EDGE_CURVE('',#4814,#4694,#1289,.T.);
#6389=EDGE_CURVE('',#4813,#4695,#300,.T.);
#6390=EDGE_CURVE('',#4817,#4698,#1290,.T.);
#6391=EDGE_CURVE('',#4816,#4699,#301,.T.);
#6392=EDGE_CURVE('',#4820,#4702,#1291,.T.);
#6393=EDGE_CURVE('',#4819,#4703,#302,.T.);
#6394=EDGE_CURVE('',#4823,#4706,#1292,.T.);
#6395=EDGE_CURVE('',#4822,#4707,#303,.T.);
#6396=EDGE_CURVE('',#4826,#4710,#1293,.T.);
#6397=EDGE_CURVE('',#4825,#4711,#304,.T.);
#6398=EDGE_CURVE('',#4829,#4714,#1294,.T.);
#6399=EDGE_CURVE('',#4828,#4715,#305,.T.);
#6400=EDGE_CURVE('',#4832,#4718,#1295,.T.);
#6401=EDGE_CURVE('',#4831,#4719,#306,.T.);
#6402=EDGE_CURVE('',#4835,#4722,#1296,.T.);
#6403=EDGE_CURVE('',#4834,#4723,#307,.T.);
#6404=EDGE_CURVE('',#4838,#4726,#1297,.T.);
#6405=EDGE_CURVE('',#4837,#4727,#1298,.T.);
#6406=EDGE_CURVE('',#4841,#4730,#1299,.T.);
#6407=EDGE_CURVE('',#4840,#4731,#1300,.T.);
#6408=EDGE_CURVE('',#4844,#4734,#1301,.T.);
#6409=EDGE_CURVE('',#4843,#4735,#308,.T.);
#6410=EDGE_CURVE('',#4847,#4738,#1302,.T.);
#6411=EDGE_CURVE('',#4846,#4739,#309,.T.);
#6412=EDGE_CURVE('',#4850,#4742,#1303,.T.);
#6413=EDGE_CURVE('',#4849,#4743,#310,.T.);
#6414=EDGE_CURVE('',#4853,#4746,#1304,.T.);
#6415=EDGE_CURVE('',#4852,#4747,#311,.T.);
#6416=EDGE_CURVE('',#4856,#4750,#1305,.T.);
#6417=EDGE_CURVE('',#4855,#4751,#312,.T.);
#6418=EDGE_CURVE('',#4859,#4754,#1306,.T.);
#6419=EDGE_CURVE('',#4858,#4755,#313,.T.);
#6420=EDGE_CURVE('',#4862,#4580,#1307,.T.);
#6421=EDGE_CURVE('',#4861,#4581,#1308,.T.);
#6422=EDGE_CURVE('',#4865,#4584,#1309,.T.);
#6423=EDGE_CURVE('',#4864,#4585,#1310,.T.);
#6424=EDGE_CURVE('',#4868,#4588,#1311,.T.);
#6425=EDGE_CURVE('',#4867,#4589,#314,.T.);
#6426=EDGE_CURVE('',#4871,#4592,#1312,.T.);
#6427=EDGE_CURVE('',#4870,#4593,#315,.T.);
#6428=EDGE_CURVE('',#4874,#4597,#316,.T.);
#6429=EDGE_CURVE('',#4873,#4596,#1313,.T.);
#6430=EDGE_CURVE('',#4877,#4600,#1314,.T.);
#6431=EDGE_CURVE('',#4876,#4601,#317,.T.);
#6432=EDGE_CURVE('',#4880,#4604,#1315,.T.);
#6433=EDGE_CURVE('',#4879,#4605,#318,.T.);
#6434=EDGE_CURVE('',#4883,#4608,#1316,.T.);
#6435=EDGE_CURVE('',#4882,#4609,#319,.T.);
#6436=EDGE_CURVE('',#4886,#4612,#1317,.T.);
#6437=EDGE_CURVE('',#4885,#4613,#320,.T.);
#6438=EDGE_CURVE('',#4889,#4616,#1318,.T.);
#6439=EDGE_CURVE('',#4888,#4617,#321,.T.);
#6440=EDGE_CURVE('',#4892,#4620,#1319,.T.);
#6441=EDGE_CURVE('',#4891,#4621,#1320,.T.);
#6442=EDGE_CURVE('',#4894,#4894,#3890,.T.);
#6443=EDGE_CURVE('',#4894,#4895,#3001,.T.);
#6444=EDGE_CURVE('',#4895,#4895,#3891,.T.);
#6445=EDGE_CURVE('',#4896,#4896,#3892,.T.);
#6446=EDGE_CURVE('',#4896,#4897,#3002,.T.);
#6447=EDGE_CURVE('',#4897,#4897,#3893,.T.);
#6448=EDGE_CURVE('',#4898,#4898,#3894,.T.);
#6449=EDGE_CURVE('',#4898,#4899,#3003,.T.);
#6450=EDGE_CURVE('',#4899,#4899,#3895,.T.);
#6451=EDGE_CURVE('',#4900,#4900,#3896,.T.);
#6452=EDGE_CURVE('',#4900,#4901,#3004,.T.);
#6453=EDGE_CURVE('',#4901,#4901,#3897,.T.);
#6454=EDGE_CURVE('',#4902,#4902,#3898,.T.);
#6455=EDGE_CURVE('',#4902,#4903,#3005,.T.);
#6456=EDGE_CURVE('',#4903,#4903,#3899,.T.);
#6457=EDGE_CURVE('',#4904,#4904,#3900,.T.);
#6458=EDGE_CURVE('',#4904,#4905,#3006,.T.);
#6459=EDGE_CURVE('',#4905,#4905,#3901,.T.);
#6460=EDGE_CURVE('',#4906,#4906,#3902,.T.);
#6461=EDGE_CURVE('',#4906,#4907,#3007,.T.);
#6462=EDGE_CURVE('',#4907,#4907,#3903,.T.);
#6463=EDGE_CURVE('',#4908,#4908,#3904,.T.);
#6464=EDGE_CURVE('',#4908,#4909,#3008,.T.);
#6465=EDGE_CURVE('',#4909,#4909,#3905,.T.);
#6466=EDGE_CURVE('',#4910,#4910,#3906,.T.);
#6467=EDGE_CURVE('',#4910,#4911,#3009,.T.);
#6468=EDGE_CURVE('',#4911,#4911,#3907,.T.);
#6469=EDGE_CURVE('',#4912,#4912,#3908,.T.);
#6470=EDGE_CURVE('',#4912,#4913,#3010,.T.);
#6471=EDGE_CURVE('',#4913,#4913,#3909,.T.);
#6472=EDGE_CURVE('',#4914,#4914,#3910,.T.);
#6473=EDGE_CURVE('',#4914,#4915,#3011,.T.);
#6474=EDGE_CURVE('',#4915,#4915,#3911,.T.);
#6475=EDGE_CURVE('',#4916,#4916,#3912,.T.);
#6476=EDGE_CURVE('',#4916,#4917,#3012,.T.);
#6477=EDGE_CURVE('',#4917,#4917,#3913,.T.);
#6478=EDGE_CURVE('',#4918,#4918,#3914,.T.);
#6479=EDGE_CURVE('',#4918,#4919,#3013,.T.);
#6480=EDGE_CURVE('',#4919,#4919,#3915,.T.);
#6481=EDGE_CURVE('',#4920,#4921,#3014,.T.);
#6482=EDGE_CURVE('',#4922,#4921,#3015,.T.);
#6483=EDGE_CURVE('',#4923,#4922,#3016,.T.);
#6484=EDGE_CURVE('',#4924,#4923,#3017,.T.);
#6485=EDGE_CURVE('',#4924,#4925,#3018,.T.);
#6486=EDGE_CURVE('',#4925,#4926,#3019,.T.);
#6487=EDGE_CURVE('',#4926,#4927,#3020,.T.);
#6488=EDGE_CURVE('',#4927,#4920,#3021,.T.);
#6489=EDGE_CURVE('',#4928,#4929,#3022,.T.);
#6490=EDGE_CURVE('',#4930,#4929,#3023,.T.);
#6491=EDGE_CURVE('',#4930,#4931,#3024,.T.);
#6492=EDGE_CURVE('',#4931,#4928,#3025,.T.);
#6493=EDGE_CURVE('',#4932,#4933,#3026,.T.);
#6494=EDGE_CURVE('',#4933,#4934,#3027,.T.);
#6495=EDGE_CURVE('',#4934,#4935,#3028,.T.);
#6496=EDGE_CURVE('',#4932,#4935,#3029,.T.);
#6497=EDGE_CURVE('',#4936,#4937,#3030,.T.);
#6498=EDGE_CURVE('',#4938,#4937,#3031,.T.);
#6499=EDGE_CURVE('',#4938,#4939,#3032,.T.);
#6500=EDGE_CURVE('',#4939,#4936,#3033,.T.);
#6501=EDGE_CURVE('',#4940,#4941,#3034,.T.);
#6502=EDGE_CURVE('',#4941,#4942,#3035,.T.);
#6503=EDGE_CURVE('',#4942,#4943,#3036,.T.);
#6504=EDGE_CURVE('',#4940,#4943,#3037,.T.);
#6505=EDGE_CURVE('',#4944,#4926,#3038,.T.);
#6506=EDGE_CURVE('',#4925,#4928,#3916,.T.);
#6507=EDGE_CURVE('',#4931,#4934,#3917,.T.);
#6508=EDGE_CURVE('',#4933,#4945,#3918,.T.);
#6509=EDGE_CURVE('',#4946,#4945,#3039,.T.);
#6510=EDGE_CURVE('',#4947,#4946,#3040,.T.);
#6511=EDGE_CURVE('',#4944,#4947,#3041,.T.);
#6512=EDGE_CURVE('',#4945,#4948,#3042,.T.);
#6513=EDGE_CURVE('',#4949,#4948,#3043,.T.);
#6514=EDGE_CURVE('',#4950,#4949,#3044,.T.);
#6515=EDGE_CURVE('',#4951,#4950,#3045,.T.);
#6516=EDGE_CURVE('',#4951,#4952,#3046,.T.);
#6517=EDGE_CURVE('',#4952,#4953,#3047,.T.);
#6518=EDGE_CURVE('',#4953,#4946,#3048,.T.);
#6519=EDGE_CURVE('',#4954,#4953,#3049,.T.);
#6520=EDGE_CURVE('',#4936,#4952,#3919,.T.);
#6521=EDGE_CURVE('',#4942,#4939,#3920,.T.);
#6522=EDGE_CURVE('',#4920,#4941,#3921,.T.);
#6523=EDGE_CURVE('',#4955,#4927,#3050,.T.);
#6524=EDGE_CURVE('',#4954,#4955,#3051,.T.);
#6525=EDGE_CURVE('',#4947,#4954,#3052,.T.);
#6526=EDGE_CURVE('',#4955,#4944,#3053,.T.);
#6527=EDGE_CURVE('',#4929,#4924,#3922,.T.);
#6528=EDGE_CURVE('',#4956,#4923,#3054,.T.);
#6529=EDGE_CURVE('',#4957,#4956,#3055,.T.);
#6530=EDGE_CURVE('',#4957,#4949,#3056,.T.);
#6531=EDGE_CURVE('',#4948,#4932,#3923,.T.);
#6532=EDGE_CURVE('',#4935,#4930,#3924,.T.);
#6533=EDGE_CURVE('',#4958,#4922,#3057,.T.);
#6534=EDGE_CURVE('',#4956,#4958,#3058,.T.);
#6535=EDGE_CURVE('',#4921,#4940,#3925,.T.);
#6536=EDGE_CURVE('',#4943,#4938,#3926,.T.);
#6537=EDGE_CURVE('',#4937,#4951,#3927,.T.);
#6538=EDGE_CURVE('',#4959,#4950,#3059,.T.);
#6539=EDGE_CURVE('',#4958,#4959,#3060,.T.);
#6540=EDGE_CURVE('',#4959,#4957,#3061,.T.);
#6541=EDGE_CURVE('',#4960,#4961,#3062,.T.);
#6542=EDGE_CURVE('',#4962,#4960,#3063,.T.);
#6543=EDGE_CURVE('',#4963,#4962,#3064,.T.);
#6544=EDGE_CURVE('',#4961,#4963,#3065,.T.);
#6545=EDGE_CURVE('',#4947,#4962,#1373,.T.);
#6546=EDGE_CURVE('',#4960,#4944,#1374,.T.);
#6547=EDGE_CURVE('',#4961,#4955,#1375,.T.);
#6548=EDGE_CURVE('',#4954,#4963,#1376,.T.);
#6549=EDGE_CURVE('',#4964,#4965,#3066,.T.);
#6550=EDGE_CURVE('',#4965,#4966,#3067,.T.);
#6551=EDGE_CURVE('',#4966,#4967,#3068,.T.);
#6552=EDGE_CURVE('',#4967,#4964,#3069,.T.);
#6553=EDGE_CURVE('',#4968,#4969,#3070,.T.);
#6554=EDGE_CURVE('',#4969,#4970,#3071,.T.);
#6555=EDGE_CURVE('',#4970,#4971,#3072,.T.);
#6556=EDGE_CURVE('',#4971,#4968,#3073,.T.);
#6557=EDGE_CURVE('',#4972,#4973,#3074,.T.);
#6558=EDGE_CURVE('',#4973,#4974,#3075,.T.);
#6559=EDGE_CURVE('',#4974,#4975,#3076,.T.);
#6560=EDGE_CURVE('',#4975,#4972,#3077,.T.);
#6561=EDGE_CURVE('',#4976,#4977,#3078,.T.);
#6562=EDGE_CURVE('',#4977,#4978,#3079,.T.);
#6563=EDGE_CURVE('',#4978,#4979,#3080,.T.);
#6564=EDGE_CURVE('',#4979,#4976,#3081,.T.);
#6565=EDGE_CURVE('',#4980,#4981,#3082,.T.);
#6566=EDGE_CURVE('',#4981,#4982,#3083,.T.);
#6567=EDGE_CURVE('',#4982,#4983,#3084,.T.);
#6568=EDGE_CURVE('',#4983,#4980,#3085,.T.);
#6569=EDGE_CURVE('',#4984,#4985,#3086,.T.);
#6570=EDGE_CURVE('',#4985,#4986,#3087,.T.);
#6571=EDGE_CURVE('',#4986,#4987,#3088,.T.);
#6572=EDGE_CURVE('',#4987,#4984,#3089,.T.);
#6573=EDGE_CURVE('',#4965,#4986,#3928,.T.);
#6574=EDGE_CURVE('',#4987,#4964,#3929,.T.);
#6575=EDGE_CURVE('',#4965,#4970,#3930,.T.);
#6576=EDGE_CURVE('',#4970,#4986,#3931,.T.);
#6577=EDGE_CURVE('',#4987,#4979,#3932,.T.);
#6578=EDGE_CURVE('',#4979,#4964,#3933,.T.);
#6579=EDGE_CURVE('',#4971,#4985,#3934,.T.);
#6580=EDGE_CURVE('',#4966,#4969,#3935,.T.);
#6581=EDGE_CURVE('',#4967,#4980,#3936,.T.);
#6582=EDGE_CURVE('',#4981,#4966,#3937,.T.);
#6583=EDGE_CURVE('',#4976,#4967,#3938,.T.);
#6584=EDGE_CURVE('',#4984,#4978,#3939,.T.);
#6585=EDGE_CURVE('',#4985,#4974,#3940,.T.);
#6586=EDGE_CURVE('',#4975,#4984,#3941,.T.);
#6587=EDGE_CURVE('',#4971,#4974,#3942,.T.);
#6588=EDGE_CURVE('',#4981,#4969,#3943,.T.);
#6589=EDGE_CURVE('',#4976,#4980,#3944,.T.);
#6590=EDGE_CURVE('',#4975,#4978,#3945,.T.);
#6591=EDGE_CURVE('',#4968,#4973,#3946,.T.);
#6592=EDGE_CURVE('',#4982,#4968,#3947,.T.);
#6593=EDGE_CURVE('',#4977,#4983,#3948,.T.);
#6594=EDGE_CURVE('',#4972,#4977,#3949,.T.);
#6595=EDGE_CURVE('',#4982,#4973,#3950,.T.);
#6596=EDGE_CURVE('',#4972,#4983,#3951,.T.);
#6597=EDGE_CURVE('',#4988,#4988,#3952,.T.);
#6598=EDGE_CURVE('',#4988,#4989,#3090,.T.);
#6599=EDGE_CURVE('',#4989,#4989,#3953,.T.);
#6600=EDGE_CURVE('',#4990,#4990,#3954,.T.);
#6601=EDGE_CURVE('',#4990,#4991,#3091,.T.);
#6602=EDGE_CURVE('',#4991,#4991,#3955,.T.);
#6603=EDGE_CURVE('',#4992,#4992,#3956,.T.);
#6604=EDGE_CURVE('',#4992,#4993,#3092,.T.);
#6605=EDGE_CURVE('',#4993,#4993,#3957,.T.);
#6606=EDGE_CURVE('',#4994,#4994,#3958,.T.);
#6607=EDGE_CURVE('',#4994,#4995,#3093,.T.);
#6608=EDGE_CURVE('',#4995,#4995,#3959,.T.);
#6609=EDGE_CURVE('',#4996,#4996,#3960,.T.);
#6610=EDGE_CURVE('',#4996,#4997,#3094,.T.);
#6611=EDGE_CURVE('',#4997,#4997,#3961,.T.);
#6612=EDGE_CURVE('',#4998,#4998,#3962,.T.);
#6613=EDGE_CURVE('',#4998,#4999,#3095,.T.);
#6614=EDGE_CURVE('',#4999,#4999,#3963,.T.);
#6615=EDGE_CURVE('',#5000,#5000,#3964,.T.);
#6616=EDGE_CURVE('',#5000,#5001,#3096,.T.);
#6617=EDGE_CURVE('',#5001,#5001,#3965,.T.);
#6618=EDGE_CURVE('',#5002,#5002,#3966,.T.);
#6619=EDGE_CURVE('',#5002,#5003,#3097,.T.);
#6620=EDGE_CURVE('',#5003,#5003,#3967,.T.);
#6621=EDGE_CURVE('',#5004,#5004,#3968,.T.);
#6622=EDGE_CURVE('',#5004,#5005,#3098,.T.);
#6623=EDGE_CURVE('',#5005,#5005,#3969,.T.);
#6624=EDGE_CURVE('',#5006,#5006,#3970,.T.);
#6625=EDGE_CURVE('',#5006,#5007,#3099,.T.);
#6626=EDGE_CURVE('',#5007,#5007,#3971,.T.);
#6627=EDGE_CURVE('',#5008,#5008,#3972,.T.);
#6628=EDGE_CURVE('',#5008,#5009,#3100,.T.);
#6629=EDGE_CURVE('',#5009,#5009,#3973,.T.);
#6630=EDGE_CURVE('',#5010,#5010,#3974,.T.);
#6631=EDGE_CURVE('',#5010,#5011,#3101,.T.);
#6632=EDGE_CURVE('',#5011,#5011,#3975,.T.);
#6633=EDGE_CURVE('',#5012,#5012,#3976,.T.);
#6634=EDGE_CURVE('',#5012,#5013,#3102,.T.);
#6635=EDGE_CURVE('',#5013,#5013,#3977,.T.);
#6636=EDGE_CURVE('',#5014,#5014,#3978,.T.);
#6637=EDGE_CURVE('',#5014,#5015,#3103,.T.);
#6638=EDGE_CURVE('',#5015,#5015,#3979,.T.);
#6639=EDGE_CURVE('',#5016,#5016,#3980,.T.);
#6640=EDGE_CURVE('',#5016,#5017,#3104,.T.);
#6641=EDGE_CURVE('',#5017,#5017,#3981,.T.);
#6642=EDGE_CURVE('',#5018,#5018,#3982,.T.);
#6643=EDGE_CURVE('',#5018,#5019,#3105,.T.);
#6644=EDGE_CURVE('',#5019,#5019,#3983,.T.);
#6645=EDGE_CURVE('',#5020,#5020,#3984,.T.);
#6646=EDGE_CURVE('',#5020,#5021,#3106,.T.);
#6647=EDGE_CURVE('',#5021,#5021,#3985,.T.);
#6648=EDGE_CURVE('',#5022,#5022,#3986,.T.);
#6649=EDGE_CURVE('',#5022,#5023,#3987,.T.);
#6650=EDGE_CURVE('',#5024,#5023,#3988,.T.);
#6651=EDGE_CURVE('',#5023,#5024,#3989,.T.);
#6652=EDGE_CURVE('',#5025,#5025,#3990,.T.);
#6653=EDGE_CURVE('',#5025,#5024,#3107,.T.);
#6654=EDGE_CURVE('',#5026,#5026,#3991,.T.);
#6655=EDGE_CURVE('',#5026,#5020,#3108,.T.);
#6656=EDGE_CURVE('',#5027,#5027,#3992,.T.);
#6657=EDGE_CURVE('',#5027,#5028,#3109,.T.);
#6658=EDGE_CURVE('',#5028,#5028,#3993,.T.);
#6659=EDGE_CURVE('',#5029,#5030,#3110,.T.);
#6660=EDGE_CURVE('',#5031,#5029,#3111,.T.);
#6661=EDGE_CURVE('',#5031,#5032,#3112,.T.);
#6662=EDGE_CURVE('',#5032,#5030,#3113,.T.);
#6663=EDGE_CURVE('',#5033,#5029,#3114,.T.);
#6664=EDGE_CURVE('',#5034,#5033,#3115,.T.);
#6665=EDGE_CURVE('',#5034,#5031,#3116,.T.);
#6666=EDGE_CURVE('',#5035,#5033,#3117,.T.);
#6667=EDGE_CURVE('',#5036,#5035,#3118,.T.);
#6668=EDGE_CURVE('',#5036,#5034,#3119,.T.);
#6669=EDGE_CURVE('',#5037,#5035,#3120,.T.);
#6670=EDGE_CURVE('',#5038,#5037,#3121,.T.);
#6671=EDGE_CURVE('',#5038,#5036,#3122,.T.);
#6672=EDGE_CURVE('',#5039,#5037,#3123,.T.);
#6673=EDGE_CURVE('',#5040,#5039,#3124,.T.);
#6674=EDGE_CURVE('',#5040,#5038,#3125,.T.);
#6675=EDGE_CURVE('',#5030,#5039,#3126,.T.);
#6676=EDGE_CURVE('',#5032,#5040,#3127,.T.);
#6677=EDGE_CURVE('',#5041,#5042,#3128,.T.);
#6678=EDGE_CURVE('',#5042,#5043,#3129,.T.);
#6679=EDGE_CURVE('',#5044,#5043,#3130,.T.);
#6680=EDGE_CURVE('',#5044,#5041,#3131,.T.);
#6681=EDGE_CURVE('',#5045,#5046,#3132,.T.);
#6682=EDGE_CURVE('',#5045,#5047,#3133,.T.);
#6683=EDGE_CURVE('',#5047,#5048,#3134,.T.);
#6684=EDGE_CURVE('',#5048,#5046,#3135,.T.);
#6685=EDGE_CURVE('',#5049,#5050,#3136,.T.);
#6686=EDGE_CURVE('',#5049,#5051,#3137,.T.);
#6687=EDGE_CURVE('',#5051,#5052,#3138,.T.);
#6688=EDGE_CURVE('',#5052,#5050,#3139,.T.);
#6689=EDGE_CURVE('',#5053,#5054,#3140,.T.);
#6690=EDGE_CURVE('',#5054,#5055,#3141,.T.);
#6691=EDGE_CURVE('',#5056,#5055,#3142,.T.);
#6692=EDGE_CURVE('',#5053,#5056,#3143,.T.);
#6693=EDGE_CURVE('',#5057,#5056,#3144,.T.);
#6694=EDGE_CURVE('',#5058,#5057,#3145,.T.);
#6695=EDGE_CURVE('',#5058,#5053,#3146,.T.);
#6696=EDGE_CURVE('',#5059,#5057,#3147,.T.);
#6697=EDGE_CURVE('',#5059,#5060,#3148,.T.);
#6698=EDGE_CURVE('',#5060,#5058,#3149,.T.);
#6699=EDGE_CURVE('',#5061,#5062,#3150,.T.);
#6700=EDGE_CURVE('',#5062,#5063,#3151,.T.);
#6701=EDGE_CURVE('',#5064,#5063,#3152,.T.);
#6702=EDGE_CURVE('',#5064,#5061,#3153,.T.);
#6703=EDGE_CURVE('',#5065,#5066,#3154,.T.);
#6704=EDGE_CURVE('',#5066,#5067,#3155,.T.);
#6705=EDGE_CURVE('',#5068,#5067,#3156,.T.);
#6706=EDGE_CURVE('',#5068,#5065,#3157,.T.);
#6707=EDGE_CURVE('',#5051,#5054,#3158,.T.);
#6708=EDGE_CURVE('',#5060,#5062,#3159,.T.);
#6709=EDGE_CURVE('',#5061,#5066,#3160,.T.);
#6710=EDGE_CURVE('',#5065,#5042,#3161,.T.);
#6711=EDGE_CURVE('',#5041,#5048,#3162,.T.);
#6712=EDGE_CURVE('',#5047,#5052,#3163,.T.);
#6713=EDGE_CURVE('',#5055,#5049,#3164,.T.);
#6714=EDGE_CURVE('',#5050,#5045,#3165,.T.);
#6715=EDGE_CURVE('',#5046,#5044,#3166,.T.);
#6716=EDGE_CURVE('',#5043,#5068,#3167,.T.);
#6717=EDGE_CURVE('',#5067,#5064,#3168,.T.);
#6718=EDGE_CURVE('',#5063,#5059,#3169,.T.);
#6719=EDGE_CURVE('',#5069,#5069,#3994,.T.);
#6720=EDGE_CURVE('',#5069,#5070,#3170,.T.);
#6721=EDGE_CURVE('',#5070,#5070,#3995,.T.);
#6722=EDGE_CURVE('',#5071,#5071,#3996,.T.);
#6723=EDGE_CURVE('',#5071,#5072,#3171,.T.);
#6724=EDGE_CURVE('',#5072,#5072,#3997,.T.);
#6725=ORIENTED_EDGE('',*,*,#5073,.T.);
#6726=ORIENTED_EDGE('',*,*,#5074,.T.);
#6727=ORIENTED_EDGE('',*,*,#5075,.T.);
#6728=ORIENTED_EDGE('',*,*,#5074,.F.);
#6729=ORIENTED_EDGE('',*,*,#5076,.T.);
#6730=ORIENTED_EDGE('',*,*,#5077,.T.);
#6731=ORIENTED_EDGE('',*,*,#5078,.T.);
#6732=ORIENTED_EDGE('',*,*,#5077,.F.);
#6733=ORIENTED_EDGE('',*,*,#5079,.F.);
#6734=ORIENTED_EDGE('',*,*,#5080,.T.);
#6735=ORIENTED_EDGE('',*,*,#5081,.T.);
#6736=ORIENTED_EDGE('',*,*,#5080,.F.);
#6737=ORIENTED_EDGE('',*,*,#5082,.F.);
#6738=ORIENTED_EDGE('',*,*,#5083,.T.);
#6739=ORIENTED_EDGE('',*,*,#5084,.T.);
#6740=ORIENTED_EDGE('',*,*,#5083,.F.);
#6741=ORIENTED_EDGE('',*,*,#5085,.F.);
#6742=ORIENTED_EDGE('',*,*,#5086,.T.);
#6743=ORIENTED_EDGE('',*,*,#5087,.T.);
#6744=ORIENTED_EDGE('',*,*,#5086,.F.);
#6745=ORIENTED_EDGE('',*,*,#5088,.F.);
#6746=ORIENTED_EDGE('',*,*,#5089,.T.);
#6747=ORIENTED_EDGE('',*,*,#5090,.T.);
#6748=ORIENTED_EDGE('',*,*,#5089,.F.);
#6749=ORIENTED_EDGE('',*,*,#5091,.F.);
#6750=ORIENTED_EDGE('',*,*,#5092,.T.);
#6751=ORIENTED_EDGE('',*,*,#5093,.T.);
#6752=ORIENTED_EDGE('',*,*,#5092,.F.);
#6753=ORIENTED_EDGE('',*,*,#5094,.F.);
#6754=ORIENTED_EDGE('',*,*,#5095,.T.);
#6755=ORIENTED_EDGE('',*,*,#5096,.T.);
#6756=ORIENTED_EDGE('',*,*,#5095,.F.);
#6757=ORIENTED_EDGE('',*,*,#5097,.F.);
#6758=ORIENTED_EDGE('',*,*,#5098,.T.);
#6759=ORIENTED_EDGE('',*,*,#5099,.T.);
#6760=ORIENTED_EDGE('',*,*,#5098,.F.);
#6761=ORIENTED_EDGE('',*,*,#5100,.F.);
#6762=ORIENTED_EDGE('',*,*,#5101,.T.);
#6763=ORIENTED_EDGE('',*,*,#5102,.T.);
#6764=ORIENTED_EDGE('',*,*,#5101,.F.);
#6765=ORIENTED_EDGE('',*,*,#5103,.F.);
#6766=ORIENTED_EDGE('',*,*,#5104,.T.);
#6767=ORIENTED_EDGE('',*,*,#5105,.T.);
#6768=ORIENTED_EDGE('',*,*,#5104,.F.);
#6769=ORIENTED_EDGE('',*,*,#5106,.F.);
#6770=ORIENTED_EDGE('',*,*,#5107,.F.);
#6771=ORIENTED_EDGE('',*,*,#5108,.F.);
#6772=ORIENTED_EDGE('',*,*,#5109,.F.);
#6773=ORIENTED_EDGE('',*,*,#5110,.F.);
#6774=ORIENTED_EDGE('',*,*,#5111,.T.);
#6775=ORIENTED_EDGE('',*,*,#5112,.T.);
#6776=ORIENTED_EDGE('',*,*,#5113,.T.);
#6777=ORIENTED_EDGE('',*,*,#5114,.F.);
#6778=ORIENTED_EDGE('',*,*,#5115,.F.);
#6779=ORIENTED_EDGE('',*,*,#5116,.F.);
#6780=ORIENTED_EDGE('',*,*,#5117,.T.);
#6781=ORIENTED_EDGE('',*,*,#5118,.F.);
#6782=ORIENTED_EDGE('',*,*,#5119,.T.);
#6783=ORIENTED_EDGE('',*,*,#5120,.F.);
#6784=ORIENTED_EDGE('',*,*,#5121,.F.);
#6785=ORIENTED_EDGE('',*,*,#5122,.F.);
#6786=ORIENTED_EDGE('',*,*,#5123,.F.);
#6787=ORIENTED_EDGE('',*,*,#5124,.F.);
#6788=ORIENTED_EDGE('',*,*,#5125,.T.);
#6789=ORIENTED_EDGE('',*,*,#5126,.F.);
#6790=ORIENTED_EDGE('',*,*,#5127,.T.);
#6791=ORIENTED_EDGE('',*,*,#5128,.F.);
#6792=ORIENTED_EDGE('',*,*,#5129,.F.);
#6793=ORIENTED_EDGE('',*,*,#5130,.F.);
#6794=ORIENTED_EDGE('',*,*,#5131,.T.);
#6795=ORIENTED_EDGE('',*,*,#5132,.T.);
#6796=ORIENTED_EDGE('',*,*,#5133,.T.);
#6797=ORIENTED_EDGE('',*,*,#5134,.F.);
#6798=ORIENTED_EDGE('',*,*,#5121,.T.);
#6799=ORIENTED_EDGE('',*,*,#5135,.F.);
#6800=ORIENTED_EDGE('',*,*,#5115,.T.);
#6801=ORIENTED_EDGE('',*,*,#5136,.F.);
#6802=ORIENTED_EDGE('',*,*,#5109,.T.);
#6803=ORIENTED_EDGE('',*,*,#5078,.F.);
#6804=ORIENTED_EDGE('',*,*,#5075,.F.);
#6805=ORIENTED_EDGE('',*,*,#5137,.F.);
#6806=ORIENTED_EDGE('',*,*,#5133,.F.);
#6807=ORIENTED_EDGE('',*,*,#5138,.F.);
#6808=ORIENTED_EDGE('',*,*,#5139,.F.);
#6809=ORIENTED_EDGE('',*,*,#5140,.F.);
#6810=ORIENTED_EDGE('',*,*,#5141,.T.);
#6811=ORIENTED_EDGE('',*,*,#5142,.T.);
#6812=ORIENTED_EDGE('',*,*,#5143,.T.);
#6813=ORIENTED_EDGE('',*,*,#5144,.F.);
#6814=ORIENTED_EDGE('',*,*,#5145,.T.);
#6815=ORIENTED_EDGE('',*,*,#5146,.T.);
#6816=ORIENTED_EDGE('',*,*,#5107,.T.);
#6817=ORIENTED_EDGE('',*,*,#5147,.T.);
#6818=ORIENTED_EDGE('',*,*,#5129,.T.);
#6819=ORIENTED_EDGE('',*,*,#5148,.T.);
#6820=ORIENTED_EDGE('',*,*,#5123,.T.);
#6821=ORIENTED_EDGE('',*,*,#5149,.T.);
#6822=ORIENTED_EDGE('',*,*,#5139,.T.);
#6823=ORIENTED_EDGE('',*,*,#5079,.T.);
#6824=ORIENTED_EDGE('',*,*,#5082,.T.);
#6825=ORIENTED_EDGE('',*,*,#5132,.F.);
#6826=ORIENTED_EDGE('',*,*,#5150,.T.);
#6827=ORIENTED_EDGE('',*,*,#5144,.T.);
#6828=ORIENTED_EDGE('',*,*,#5138,.T.);
#6829=ORIENTED_EDGE('',*,*,#5146,.F.);
#6830=ORIENTED_EDGE('',*,*,#5151,.T.);
#6831=ORIENTED_EDGE('',*,*,#5130,.T.);
#6832=ORIENTED_EDGE('',*,*,#5108,.T.);
#6833=ORIENTED_EDGE('',*,*,#5152,.F.);
#6834=ORIENTED_EDGE('',*,*,#5117,.F.);
#6835=ORIENTED_EDGE('',*,*,#5153,.F.);
#6836=ORIENTED_EDGE('',*,*,#5119,.F.);
#6837=ORIENTED_EDGE('',*,*,#5154,.F.);
#6838=ORIENTED_EDGE('',*,*,#5143,.F.);
#6839=ORIENTED_EDGE('',*,*,#5155,.F.);
#6840=ORIENTED_EDGE('',*,*,#5156,.T.);
#6841=ORIENTED_EDGE('',*,*,#5157,.T.);
#6842=ORIENTED_EDGE('',*,*,#5111,.F.);
#6843=ORIENTED_EDGE('',*,*,#5073,.F.);
#6844=ORIENTED_EDGE('',*,*,#5076,.F.);
#6845=ORIENTED_EDGE('',*,*,#5112,.F.);
#6846=ORIENTED_EDGE('',*,*,#5157,.F.);
#6847=ORIENTED_EDGE('',*,*,#5158,.T.);
#6848=ORIENTED_EDGE('',*,*,#5159,.T.);
#6849=ORIENTED_EDGE('',*,*,#5160,.F.);
#6850=ORIENTED_EDGE('',*,*,#5113,.F.);
#6851=ORIENTED_EDGE('',*,*,#5159,.F.);
#6852=ORIENTED_EDGE('',*,*,#5161,.T.);
#6853=ORIENTED_EDGE('',*,*,#5162,.T.);
#6854=ORIENTED_EDGE('',*,*,#5141,.F.);
#6855=ORIENTED_EDGE('',*,*,#5163,.F.);
#6856=ORIENTED_EDGE('',*,*,#5125,.F.);
#6857=ORIENTED_EDGE('',*,*,#5164,.F.);
#6858=ORIENTED_EDGE('',*,*,#5127,.F.);
#6859=ORIENTED_EDGE('',*,*,#5081,.F.);
#6860=ORIENTED_EDGE('',*,*,#5084,.F.);
#6861=ORIENTED_EDGE('',*,*,#5142,.F.);
#6862=ORIENTED_EDGE('',*,*,#5162,.F.);
#6863=ORIENTED_EDGE('',*,*,#5165,.T.);
#6864=ORIENTED_EDGE('',*,*,#5155,.T.);
#6865=ORIENTED_EDGE('',*,*,#5156,.F.);
#6866=ORIENTED_EDGE('',*,*,#5165,.F.);
#6867=ORIENTED_EDGE('',*,*,#5161,.F.);
#6868=ORIENTED_EDGE('',*,*,#5158,.F.);
#6869=ORIENTED_EDGE('',*,*,#5085,.T.);
#6870=ORIENTED_EDGE('',*,*,#5088,.T.);
#6871=ORIENTED_EDGE('',*,*,#5091,.T.);
#6872=ORIENTED_EDGE('',*,*,#5094,.T.);
#6873=ORIENTED_EDGE('',*,*,#5097,.T.);
#6874=ORIENTED_EDGE('',*,*,#5100,.T.);
#6875=ORIENTED_EDGE('',*,*,#5103,.T.);
#6876=ORIENTED_EDGE('',*,*,#5166,.T.);
#6877=ORIENTED_EDGE('',*,*,#5167,.T.);
#6878=ORIENTED_EDGE('',*,*,#5168,.T.);
#6879=ORIENTED_EDGE('',*,*,#5169,.T.);
#6880=ORIENTED_EDGE('',*,*,#5087,.F.);
#6881=ORIENTED_EDGE('',*,*,#5090,.F.);
#6882=ORIENTED_EDGE('',*,*,#5093,.F.);
#6883=ORIENTED_EDGE('',*,*,#5096,.F.);
#6884=ORIENTED_EDGE('',*,*,#5099,.F.);
#6885=ORIENTED_EDGE('',*,*,#5102,.F.);
#6886=ORIENTED_EDGE('',*,*,#5105,.F.);
#6887=ORIENTED_EDGE('',*,*,#5128,.T.);
#6888=ORIENTED_EDGE('',*,*,#5164,.T.);
#6889=ORIENTED_EDGE('',*,*,#5124,.T.);
#6890=ORIENTED_EDGE('',*,*,#5148,.F.);
#6891=ORIENTED_EDGE('',*,*,#5122,.T.);
#6892=ORIENTED_EDGE('',*,*,#5163,.T.);
#6893=ORIENTED_EDGE('',*,*,#5140,.T.);
#6894=ORIENTED_EDGE('',*,*,#5149,.F.);
#6895=ORIENTED_EDGE('',*,*,#5106,.T.);
#6896=ORIENTED_EDGE('',*,*,#5160,.T.);
#6897=ORIENTED_EDGE('',*,*,#5126,.T.);
#6898=ORIENTED_EDGE('',*,*,#5147,.F.);
#6899=ORIENTED_EDGE('',*,*,#5116,.T.);
#6900=ORIENTED_EDGE('',*,*,#5135,.T.);
#6901=ORIENTED_EDGE('',*,*,#5120,.T.);
#6902=ORIENTED_EDGE('',*,*,#5153,.T.);
#6903=ORIENTED_EDGE('',*,*,#5118,.T.);
#6904=ORIENTED_EDGE('',*,*,#5134,.T.);
#6905=ORIENTED_EDGE('',*,*,#5137,.T.);
#6906=ORIENTED_EDGE('',*,*,#5154,.T.);
#6907=ORIENTED_EDGE('',*,*,#5110,.T.);
#6908=ORIENTED_EDGE('',*,*,#5136,.T.);
#6909=ORIENTED_EDGE('',*,*,#5114,.T.);
#6910=ORIENTED_EDGE('',*,*,#5152,.T.);
#6911=ORIENTED_EDGE('',*,*,#5170,.F.);
#6912=ORIENTED_EDGE('',*,*,#5131,.F.);
#6913=ORIENTED_EDGE('',*,*,#5171,.F.);
#6914=ORIENTED_EDGE('',*,*,#5169,.F.);
#6915=ORIENTED_EDGE('',*,*,#5171,.T.);
#6916=ORIENTED_EDGE('',*,*,#5151,.F.);
#6917=ORIENTED_EDGE('',*,*,#5172,.F.);
#6918=ORIENTED_EDGE('',*,*,#5166,.F.);
#6919=ORIENTED_EDGE('',*,*,#5170,.T.);
#6920=ORIENTED_EDGE('',*,*,#5168,.F.);
#6921=ORIENTED_EDGE('',*,*,#5173,.F.);
#6922=ORIENTED_EDGE('',*,*,#5150,.F.);
#6923=ORIENTED_EDGE('',*,*,#5172,.T.);
#6924=ORIENTED_EDGE('',*,*,#5145,.F.);
#6925=ORIENTED_EDGE('',*,*,#5173,.T.);
#6926=ORIENTED_EDGE('',*,*,#5167,.F.);
#6927=ORIENTED_EDGE('',*,*,#5174,.T.);
#6928=ORIENTED_EDGE('',*,*,#5175,.T.);
#6929=ORIENTED_EDGE('',*,*,#5176,.T.);
#6930=ORIENTED_EDGE('',*,*,#5177,.F.);
#6931=ORIENTED_EDGE('',*,*,#5178,.T.);
#6932=ORIENTED_EDGE('',*,*,#5179,.T.);
#6933=ORIENTED_EDGE('',*,*,#5178,.F.);
#6934=ORIENTED_EDGE('',*,*,#5180,.F.);
#6935=ORIENTED_EDGE('',*,*,#5181,.T.);
#6936=ORIENTED_EDGE('',*,*,#5182,.T.);
#6937=ORIENTED_EDGE('',*,*,#5174,.F.);
#6938=ORIENTED_EDGE('',*,*,#5183,.F.);
#6939=ORIENTED_EDGE('',*,*,#5184,.T.);
#6940=ORIENTED_EDGE('',*,*,#5185,.T.);
#6941=ORIENTED_EDGE('',*,*,#5181,.F.);
#6942=ORIENTED_EDGE('',*,*,#5186,.F.);
#6943=ORIENTED_EDGE('',*,*,#5187,.T.);
#6944=ORIENTED_EDGE('',*,*,#5188,.T.);
#6945=ORIENTED_EDGE('',*,*,#5184,.F.);
#6946=ORIENTED_EDGE('',*,*,#5189,.F.);
#6947=ORIENTED_EDGE('',*,*,#5190,.T.);
#6948=ORIENTED_EDGE('',*,*,#5191,.T.);
#6949=ORIENTED_EDGE('',*,*,#5192,.F.);
#6950=ORIENTED_EDGE('',*,*,#5193,.T.);
#6951=ORIENTED_EDGE('',*,*,#5187,.F.);
#6952=ORIENTED_EDGE('',*,*,#5194,.T.);
#6953=ORIENTED_EDGE('',*,*,#5195,.T.);
#6954=ORIENTED_EDGE('',*,*,#5196,.F.);
#6955=ORIENTED_EDGE('',*,*,#5191,.F.);
#6956=ORIENTED_EDGE('',*,*,#5197,.T.);
#6957=ORIENTED_EDGE('',*,*,#5198,.F.);
#6958=ORIENTED_EDGE('',*,*,#5199,.T.);
#6959=ORIENTED_EDGE('',*,*,#5200,.F.);
#6960=ORIENTED_EDGE('',*,*,#5201,.F.);
#6961=ORIENTED_EDGE('',*,*,#5202,.T.);
#6962=ORIENTED_EDGE('',*,*,#5203,.F.);
#6963=ORIENTED_EDGE('',*,*,#5204,.F.);
#6964=ORIENTED_EDGE('',*,*,#5199,.F.);
#6965=ORIENTED_EDGE('',*,*,#5205,.F.);
#6966=ORIENTED_EDGE('',*,*,#5206,.F.);
#6967=ORIENTED_EDGE('',*,*,#5207,.T.);
#6968=ORIENTED_EDGE('',*,*,#5208,.F.);
#6969=ORIENTED_EDGE('',*,*,#5207,.F.);
#6970=ORIENTED_EDGE('',*,*,#5209,.F.);
#6971=ORIENTED_EDGE('',*,*,#5210,.F.);
#6972=ORIENTED_EDGE('',*,*,#5211,.F.);
#6973=ORIENTED_EDGE('',*,*,#5212,.T.);
#6974=ORIENTED_EDGE('',*,*,#5213,.T.);
#6975=ORIENTED_EDGE('',*,*,#5212,.F.);
#6976=ORIENTED_EDGE('',*,*,#5214,.F.);
#6977=ORIENTED_EDGE('',*,*,#5215,.F.);
#6978=ORIENTED_EDGE('',*,*,#5216,.F.);
#6979=ORIENTED_EDGE('',*,*,#5217,.T.);
#6980=ORIENTED_EDGE('',*,*,#5218,.T.);
#6981=ORIENTED_EDGE('',*,*,#5217,.F.);
#6982=ORIENTED_EDGE('',*,*,#5219,.F.);
#6983=ORIENTED_EDGE('',*,*,#5220,.T.);
#6984=ORIENTED_EDGE('',*,*,#5205,.T.);
#6985=ORIENTED_EDGE('',*,*,#5206,.T.);
#6986=ORIENTED_EDGE('',*,*,#5220,.F.);
#6987=ORIENTED_EDGE('',*,*,#5201,.T.);
#6988=ORIENTED_EDGE('',*,*,#5221,.F.);
#6989=ORIENTED_EDGE('',*,*,#5195,.F.);
#6990=ORIENTED_EDGE('',*,*,#5222,.T.);
#6991=ORIENTED_EDGE('',*,*,#5179,.F.);
#6992=ORIENTED_EDGE('',*,*,#5219,.T.);
#6993=ORIENTED_EDGE('',*,*,#5198,.T.);
#6994=ORIENTED_EDGE('',*,*,#5218,.F.);
#6995=ORIENTED_EDGE('',*,*,#5216,.T.);
#6996=ORIENTED_EDGE('',*,*,#5213,.F.);
#6997=ORIENTED_EDGE('',*,*,#5223,.T.);
#6998=ORIENTED_EDGE('',*,*,#5203,.T.);
#6999=ORIENTED_EDGE('',*,*,#5224,.T.);
#7000=ORIENTED_EDGE('',*,*,#5225,.T.);
#7001=ORIENTED_EDGE('',*,*,#5226,.F.);
#7002=ORIENTED_EDGE('',*,*,#5227,.T.);
#7003=ORIENTED_EDGE('',*,*,#5224,.F.);
#7004=ORIENTED_EDGE('',*,*,#5202,.F.);
#7005=ORIENTED_EDGE('',*,*,#5222,.F.);
#7006=ORIENTED_EDGE('',*,*,#5197,.F.);
#7007=ORIENTED_EDGE('',*,*,#5194,.F.);
#7008=ORIENTED_EDGE('',*,*,#5190,.F.);
#7009=ORIENTED_EDGE('',*,*,#5228,.F.);
#7010=ORIENTED_EDGE('',*,*,#5229,.T.);
#7011=ORIENTED_EDGE('',*,*,#5225,.F.);
#7012=ORIENTED_EDGE('',*,*,#5227,.F.);
#7013=ORIENTED_EDGE('',*,*,#5230,.F.);
#7014=ORIENTED_EDGE('',*,*,#5192,.T.);
#7015=ORIENTED_EDGE('',*,*,#5196,.T.);
#7016=ORIENTED_EDGE('',*,*,#5221,.T.);
#7017=ORIENTED_EDGE('',*,*,#5200,.T.);
#7018=ORIENTED_EDGE('',*,*,#5204,.T.);
#7019=ORIENTED_EDGE('',*,*,#5223,.F.);
#7020=ORIENTED_EDGE('',*,*,#5229,.F.);
#7021=ORIENTED_EDGE('',*,*,#5176,.F.);
#7022=ORIENTED_EDGE('',*,*,#5231,.F.);
#7023=ORIENTED_EDGE('',*,*,#5232,.F.);
#7024=ORIENTED_EDGE('',*,*,#5233,.F.);
#7025=ORIENTED_EDGE('',*,*,#5226,.T.);
#7026=ORIENTED_EDGE('',*,*,#5189,.T.);
#7027=ORIENTED_EDGE('',*,*,#5186,.T.);
#7028=ORIENTED_EDGE('',*,*,#5183,.T.);
#7029=ORIENTED_EDGE('',*,*,#5180,.T.);
#7030=ORIENTED_EDGE('',*,*,#5177,.T.);
#7031=ORIENTED_EDGE('',*,*,#5233,.T.);
#7032=ORIENTED_EDGE('',*,*,#5234,.F.);
#7033=ORIENTED_EDGE('',*,*,#5228,.T.);
#7034=ORIENTED_EDGE('',*,*,#5234,.T.);
#7035=ORIENTED_EDGE('',*,*,#5232,.T.);
#7036=ORIENTED_EDGE('',*,*,#5235,.F.);
#7037=ORIENTED_EDGE('',*,*,#5230,.T.);
#7038=ORIENTED_EDGE('',*,*,#5235,.T.);
#7039=ORIENTED_EDGE('',*,*,#5231,.T.);
#7040=ORIENTED_EDGE('',*,*,#5175,.F.);
#7041=ORIENTED_EDGE('',*,*,#5182,.F.);
#7042=ORIENTED_EDGE('',*,*,#5185,.F.);
#7043=ORIENTED_EDGE('',*,*,#5188,.F.);
#7044=ORIENTED_EDGE('',*,*,#5193,.F.);
#7045=ORIENTED_EDGE('',*,*,#5236,.F.);
#7046=ORIENTED_EDGE('',*,*,#5237,.F.);
#7047=ORIENTED_EDGE('',*,*,#5238,.F.);
#7048=ORIENTED_EDGE('',*,*,#5214,.T.);
#7049=ORIENTED_EDGE('',*,*,#5211,.T.);
#7050=ORIENTED_EDGE('',*,*,#5210,.T.);
#7051=ORIENTED_EDGE('',*,*,#5239,.F.);
#7052=ORIENTED_EDGE('',*,*,#5240,.T.);
#7053=ORIENTED_EDGE('',*,*,#5236,.T.);
#7054=ORIENTED_EDGE('',*,*,#5237,.T.);
#7055=ORIENTED_EDGE('',*,*,#5240,.F.);
#7056=ORIENTED_EDGE('',*,*,#5241,.F.);
#7057=ORIENTED_EDGE('',*,*,#5242,.T.);
#7058=ORIENTED_EDGE('',*,*,#5215,.T.);
#7059=ORIENTED_EDGE('',*,*,#5238,.T.);
#7060=ORIENTED_EDGE('',*,*,#5242,.F.);
#7061=ORIENTED_EDGE('',*,*,#5243,.F.);
#7062=ORIENTED_EDGE('',*,*,#5209,.T.);
#7063=ORIENTED_EDGE('',*,*,#5243,.T.);
#7064=ORIENTED_EDGE('',*,*,#5241,.T.);
#7065=ORIENTED_EDGE('',*,*,#5239,.T.);
#7066=ORIENTED_EDGE('',*,*,#5208,.T.);
#7067=ORIENTED_EDGE('',*,*,#5244,.F.);
#7068=ORIENTED_EDGE('',*,*,#5245,.F.);
#7069=ORIENTED_EDGE('',*,*,#5246,.T.);
#7070=ORIENTED_EDGE('',*,*,#5247,.F.);
#7071=ORIENTED_EDGE('',*,*,#5246,.F.);
#7072=ORIENTED_EDGE('',*,*,#5248,.T.);
#7073=ORIENTED_EDGE('',*,*,#5249,.T.);
#7074=ORIENTED_EDGE('',*,*,#5250,.F.);
#7075=ORIENTED_EDGE('',*,*,#5249,.F.);
#7076=ORIENTED_EDGE('',*,*,#5251,.F.);
#7077=ORIENTED_EDGE('',*,*,#5252,.T.);
#7078=ORIENTED_EDGE('',*,*,#5253,.T.);
#7079=ORIENTED_EDGE('',*,*,#5254,.F.);
#7080=ORIENTED_EDGE('',*,*,#5244,.T.);
#7081=ORIENTED_EDGE('',*,*,#5245,.T.);
#7082=ORIENTED_EDGE('',*,*,#5255,.T.);
#7083=ORIENTED_EDGE('',*,*,#5256,.T.);
#7084=ORIENTED_EDGE('',*,*,#5255,.F.);
#7085=ORIENTED_EDGE('',*,*,#5257,.T.);
#7086=ORIENTED_EDGE('',*,*,#5258,.T.);
#7087=ORIENTED_EDGE('',*,*,#5259,.F.);
#7088=ORIENTED_EDGE('',*,*,#5260,.F.);
#7089=ORIENTED_EDGE('',*,*,#5261,.F.);
#7090=ORIENTED_EDGE('',*,*,#5262,.T.);
#7091=ORIENTED_EDGE('',*,*,#5263,.F.);
#7092=ORIENTED_EDGE('',*,*,#5258,.F.);
#7093=ORIENTED_EDGE('',*,*,#5264,.F.);
#7094=ORIENTED_EDGE('',*,*,#5265,.T.);
#7095=ORIENTED_EDGE('',*,*,#5259,.T.);
#7096=ORIENTED_EDGE('',*,*,#5263,.T.);
#7097=ORIENTED_EDGE('',*,*,#5266,.F.);
#7098=ORIENTED_EDGE('',*,*,#5247,.T.);
#7099=ORIENTED_EDGE('',*,*,#5267,.T.);
#7100=ORIENTED_EDGE('',*,*,#5252,.F.);
#7101=ORIENTED_EDGE('',*,*,#5268,.F.);
#7102=ORIENTED_EDGE('',*,*,#5269,.T.);
#7103=ORIENTED_EDGE('',*,*,#5270,.F.);
#7104=ORIENTED_EDGE('',*,*,#5271,.F.);
#7105=ORIENTED_EDGE('',*,*,#5272,.T.);
#7106=ORIENTED_EDGE('',*,*,#5254,.T.);
#7107=ORIENTED_EDGE('',*,*,#5273,.F.);
#7108=ORIENTED_EDGE('',*,*,#5269,.F.);
#7109=ORIENTED_EDGE('',*,*,#5274,.T.);
#7110=ORIENTED_EDGE('',*,*,#5271,.T.);
#7111=ORIENTED_EDGE('',*,*,#5268,.T.);
#7112=ORIENTED_EDGE('',*,*,#5251,.T.);
#7113=ORIENTED_EDGE('',*,*,#5272,.F.);
#7114=ORIENTED_EDGE('',*,*,#5274,.F.);
#7115=ORIENTED_EDGE('',*,*,#5248,.F.);
#7116=ORIENTED_EDGE('',*,*,#5267,.F.);
#7117=ORIENTED_EDGE('',*,*,#5273,.T.);
#7118=ORIENTED_EDGE('',*,*,#5270,.T.);
#7119=ORIENTED_EDGE('',*,*,#5253,.F.);
#7120=ORIENTED_EDGE('',*,*,#5256,.F.);
#7121=ORIENTED_EDGE('',*,*,#5250,.T.);
#7122=ORIENTED_EDGE('',*,*,#5257,.F.);
#7123=ORIENTED_EDGE('',*,*,#5261,.T.);
#7124=ORIENTED_EDGE('',*,*,#5275,.F.);
#7125=ORIENTED_EDGE('',*,*,#5276,.T.);
#7126=ORIENTED_EDGE('',*,*,#5277,.T.);
#7127=ORIENTED_EDGE('',*,*,#5260,.T.);
#7128=ORIENTED_EDGE('',*,*,#5265,.F.);
#7129=ORIENTED_EDGE('',*,*,#5278,.F.);
#7130=ORIENTED_EDGE('',*,*,#5275,.T.);
#7131=ORIENTED_EDGE('',*,*,#5277,.F.);
#7132=ORIENTED_EDGE('',*,*,#5279,.T.);
#7133=ORIENTED_EDGE('',*,*,#5266,.T.);
#7134=ORIENTED_EDGE('',*,*,#5262,.F.);
#7135=ORIENTED_EDGE('',*,*,#5264,.T.);
#7136=ORIENTED_EDGE('',*,*,#5279,.F.);
#7137=ORIENTED_EDGE('',*,*,#5276,.F.);
#7138=ORIENTED_EDGE('',*,*,#5278,.T.);
#7139=ORIENTED_EDGE('',*,*,#5280,.T.);
#7140=ORIENTED_EDGE('',*,*,#5281,.F.);
#7141=ORIENTED_EDGE('',*,*,#5282,.F.);
#7142=ORIENTED_EDGE('',*,*,#5283,.F.);
#7143=ORIENTED_EDGE('',*,*,#5284,.T.);
#7144=ORIENTED_EDGE('',*,*,#5285,.F.);
#7145=ORIENTED_EDGE('',*,*,#5286,.T.);
#7146=ORIENTED_EDGE('',*,*,#5287,.F.);
#7147=ORIENTED_EDGE('',*,*,#5288,.F.);
#7148=ORIENTED_EDGE('',*,*,#5289,.F.);
#7149=ORIENTED_EDGE('',*,*,#5290,.T.);
#7150=ORIENTED_EDGE('',*,*,#5291,.F.);
#7151=ORIENTED_EDGE('',*,*,#5292,.T.);
#7152=ORIENTED_EDGE('',*,*,#5293,.F.);
#7153=ORIENTED_EDGE('',*,*,#5294,.F.);
#7154=ORIENTED_EDGE('',*,*,#5295,.F.);
#7155=ORIENTED_EDGE('',*,*,#5296,.T.);
#7156=ORIENTED_EDGE('',*,*,#5297,.F.);
#7157=ORIENTED_EDGE('',*,*,#5298,.T.);
#7158=ORIENTED_EDGE('',*,*,#5299,.F.);
#7159=ORIENTED_EDGE('',*,*,#5300,.F.);
#7160=ORIENTED_EDGE('',*,*,#5301,.F.);
#7161=ORIENTED_EDGE('',*,*,#5302,.T.);
#7162=ORIENTED_EDGE('',*,*,#5303,.F.);
#7163=ORIENTED_EDGE('',*,*,#5304,.T.);
#7164=ORIENTED_EDGE('',*,*,#5305,.F.);
#7165=ORIENTED_EDGE('',*,*,#5306,.F.);
#7166=ORIENTED_EDGE('',*,*,#5307,.F.);
#7167=ORIENTED_EDGE('',*,*,#5308,.T.);
#7168=ORIENTED_EDGE('',*,*,#5309,.F.);
#7169=ORIENTED_EDGE('',*,*,#5310,.T.);
#7170=ORIENTED_EDGE('',*,*,#5311,.F.);
#7171=ORIENTED_EDGE('',*,*,#5312,.F.);
#7172=ORIENTED_EDGE('',*,*,#5313,.F.);
#7173=ORIENTED_EDGE('',*,*,#5314,.T.);
#7174=ORIENTED_EDGE('',*,*,#5315,.F.);
#7175=ORIENTED_EDGE('',*,*,#5316,.T.);
#7176=ORIENTED_EDGE('',*,*,#5317,.F.);
#7177=ORIENTED_EDGE('',*,*,#5318,.F.);
#7178=ORIENTED_EDGE('',*,*,#5319,.F.);
#7179=ORIENTED_EDGE('',*,*,#5320,.T.);
#7180=ORIENTED_EDGE('',*,*,#5321,.F.);
#7181=ORIENTED_EDGE('',*,*,#5322,.T.);
#7182=ORIENTED_EDGE('',*,*,#5323,.F.);
#7183=ORIENTED_EDGE('',*,*,#5324,.F.);
#7184=ORIENTED_EDGE('',*,*,#5325,.F.);
#7185=ORIENTED_EDGE('',*,*,#5326,.T.);
#7186=ORIENTED_EDGE('',*,*,#5327,.F.);
#7187=ORIENTED_EDGE('',*,*,#5328,.T.);
#7188=ORIENTED_EDGE('',*,*,#5329,.F.);
#7189=ORIENTED_EDGE('',*,*,#5330,.F.);
#7190=ORIENTED_EDGE('',*,*,#5331,.F.);
#7191=ORIENTED_EDGE('',*,*,#5332,.T.);
#7192=ORIENTED_EDGE('',*,*,#5333,.F.);
#7193=ORIENTED_EDGE('',*,*,#5334,.T.);
#7194=ORIENTED_EDGE('',*,*,#5335,.F.);
#7195=ORIENTED_EDGE('',*,*,#5336,.F.);
#7196=ORIENTED_EDGE('',*,*,#5337,.F.);
#7197=ORIENTED_EDGE('',*,*,#5338,.T.);
#7198=ORIENTED_EDGE('',*,*,#5339,.F.);
#7199=ORIENTED_EDGE('',*,*,#5340,.T.);
#7200=ORIENTED_EDGE('',*,*,#5341,.F.);
#7201=ORIENTED_EDGE('',*,*,#5342,.F.);
#7202=ORIENTED_EDGE('',*,*,#5343,.F.);
#7203=ORIENTED_EDGE('',*,*,#5344,.T.);
#7204=ORIENTED_EDGE('',*,*,#5345,.F.);
#7205=ORIENTED_EDGE('',*,*,#5346,.T.);
#7206=ORIENTED_EDGE('',*,*,#5347,.F.);
#7207=ORIENTED_EDGE('',*,*,#5348,.F.);
#7208=ORIENTED_EDGE('',*,*,#5349,.F.);
#7209=ORIENTED_EDGE('',*,*,#5350,.T.);
#7210=ORIENTED_EDGE('',*,*,#5351,.F.);
#7211=ORIENTED_EDGE('',*,*,#5352,.T.);
#7212=ORIENTED_EDGE('',*,*,#5353,.F.);
#7213=ORIENTED_EDGE('',*,*,#5354,.F.);
#7214=ORIENTED_EDGE('',*,*,#5355,.F.);
#7215=ORIENTED_EDGE('',*,*,#5356,.T.);
#7216=ORIENTED_EDGE('',*,*,#5357,.F.);
#7217=ORIENTED_EDGE('',*,*,#5358,.T.);
#7218=ORIENTED_EDGE('',*,*,#5359,.F.);
#7219=ORIENTED_EDGE('',*,*,#5360,.F.);
#7220=ORIENTED_EDGE('',*,*,#5361,.F.);
#7221=ORIENTED_EDGE('',*,*,#5362,.T.);
#7222=ORIENTED_EDGE('',*,*,#5363,.F.);
#7223=ORIENTED_EDGE('',*,*,#5364,.T.);
#7224=ORIENTED_EDGE('',*,*,#5365,.F.);
#7225=ORIENTED_EDGE('',*,*,#5366,.F.);
#7226=ORIENTED_EDGE('',*,*,#5367,.F.);
#7227=ORIENTED_EDGE('',*,*,#5368,.T.);
#7228=ORIENTED_EDGE('',*,*,#5369,.F.);
#7229=ORIENTED_EDGE('',*,*,#5370,.T.);
#7230=ORIENTED_EDGE('',*,*,#5371,.F.);
#7231=ORIENTED_EDGE('',*,*,#5372,.F.);
#7232=ORIENTED_EDGE('',*,*,#5373,.F.);
#7233=ORIENTED_EDGE('',*,*,#5374,.T.);
#7234=ORIENTED_EDGE('',*,*,#5375,.F.);
#7235=ORIENTED_EDGE('',*,*,#5376,.T.);
#7236=ORIENTED_EDGE('',*,*,#5377,.F.);
#7237=ORIENTED_EDGE('',*,*,#5378,.F.);
#7238=ORIENTED_EDGE('',*,*,#5379,.F.);
#7239=ORIENTED_EDGE('',*,*,#5380,.T.);
#7240=ORIENTED_EDGE('',*,*,#5381,.F.);
#7241=ORIENTED_EDGE('',*,*,#5382,.T.);
#7242=ORIENTED_EDGE('',*,*,#5383,.F.);
#7243=ORIENTED_EDGE('',*,*,#5384,.F.);
#7244=ORIENTED_EDGE('',*,*,#5385,.F.);
#7245=ORIENTED_EDGE('',*,*,#5386,.T.);
#7246=ORIENTED_EDGE('',*,*,#5387,.F.);
#7247=ORIENTED_EDGE('',*,*,#5388,.T.);
#7248=ORIENTED_EDGE('',*,*,#5389,.F.);
#7249=ORIENTED_EDGE('',*,*,#5390,.F.);
#7250=ORIENTED_EDGE('',*,*,#5391,.F.);
#7251=ORIENTED_EDGE('',*,*,#5392,.T.);
#7252=ORIENTED_EDGE('',*,*,#5393,.F.);
#7253=ORIENTED_EDGE('',*,*,#5394,.T.);
#7254=ORIENTED_EDGE('',*,*,#5395,.F.);
#7255=ORIENTED_EDGE('',*,*,#5396,.F.);
#7256=ORIENTED_EDGE('',*,*,#5397,.F.);
#7257=ORIENTED_EDGE('',*,*,#5398,.T.);
#7258=ORIENTED_EDGE('',*,*,#5399,.F.);
#7259=ORIENTED_EDGE('',*,*,#5400,.T.);
#7260=ORIENTED_EDGE('',*,*,#5401,.F.);
#7261=ORIENTED_EDGE('',*,*,#5402,.F.);
#7262=ORIENTED_EDGE('',*,*,#5403,.F.);
#7263=ORIENTED_EDGE('',*,*,#5404,.T.);
#7264=ORIENTED_EDGE('',*,*,#5405,.F.);
#7265=ORIENTED_EDGE('',*,*,#5406,.T.);
#7266=ORIENTED_EDGE('',*,*,#5407,.F.);
#7267=ORIENTED_EDGE('',*,*,#5408,.F.);
#7268=ORIENTED_EDGE('',*,*,#5409,.F.);
#7269=ORIENTED_EDGE('',*,*,#5410,.T.);
#7270=ORIENTED_EDGE('',*,*,#5411,.F.);
#7271=ORIENTED_EDGE('',*,*,#5412,.T.);
#7272=ORIENTED_EDGE('',*,*,#5413,.F.);
#7273=ORIENTED_EDGE('',*,*,#5414,.F.);
#7274=ORIENTED_EDGE('',*,*,#5415,.F.);
#7275=ORIENTED_EDGE('',*,*,#5416,.T.);
#7276=ORIENTED_EDGE('',*,*,#5417,.F.);
#7277=ORIENTED_EDGE('',*,*,#5418,.T.);
#7278=ORIENTED_EDGE('',*,*,#5419,.F.);
#7279=ORIENTED_EDGE('',*,*,#5420,.F.);
#7280=ORIENTED_EDGE('',*,*,#5421,.F.);
#7281=ORIENTED_EDGE('',*,*,#5422,.T.);
#7282=ORIENTED_EDGE('',*,*,#5423,.F.);
#7283=ORIENTED_EDGE('',*,*,#5424,.T.);
#7284=ORIENTED_EDGE('',*,*,#5425,.F.);
#7285=ORIENTED_EDGE('',*,*,#5426,.F.);
#7286=ORIENTED_EDGE('',*,*,#5427,.F.);
#7287=ORIENTED_EDGE('',*,*,#5428,.T.);
#7288=ORIENTED_EDGE('',*,*,#5429,.F.);
#7289=ORIENTED_EDGE('',*,*,#5430,.T.);
#7290=ORIENTED_EDGE('',*,*,#5431,.F.);
#7291=ORIENTED_EDGE('',*,*,#5432,.F.);
#7292=ORIENTED_EDGE('',*,*,#5433,.F.);
#7293=ORIENTED_EDGE('',*,*,#5434,.T.);
#7294=ORIENTED_EDGE('',*,*,#5435,.F.);
#7295=ORIENTED_EDGE('',*,*,#5436,.T.);
#7296=ORIENTED_EDGE('',*,*,#5437,.F.);
#7297=ORIENTED_EDGE('',*,*,#5438,.F.);
#7298=ORIENTED_EDGE('',*,*,#5439,.F.);
#7299=ORIENTED_EDGE('',*,*,#5440,.T.);
#7300=ORIENTED_EDGE('',*,*,#5441,.F.);
#7301=ORIENTED_EDGE('',*,*,#5442,.T.);
#7302=ORIENTED_EDGE('',*,*,#5443,.F.);
#7303=ORIENTED_EDGE('',*,*,#5444,.F.);
#7304=ORIENTED_EDGE('',*,*,#5445,.F.);
#7305=ORIENTED_EDGE('',*,*,#5446,.T.);
#7306=ORIENTED_EDGE('',*,*,#5447,.F.);
#7307=ORIENTED_EDGE('',*,*,#5448,.T.);
#7308=ORIENTED_EDGE('',*,*,#5449,.F.);
#7309=ORIENTED_EDGE('',*,*,#5450,.F.);
#7310=ORIENTED_EDGE('',*,*,#5451,.F.);
#7311=ORIENTED_EDGE('',*,*,#5452,.T.);
#7312=ORIENTED_EDGE('',*,*,#5453,.F.);
#7313=ORIENTED_EDGE('',*,*,#5454,.T.);
#7314=ORIENTED_EDGE('',*,*,#5455,.F.);
#7315=ORIENTED_EDGE('',*,*,#5456,.F.);
#7316=ORIENTED_EDGE('',*,*,#5457,.F.);
#7317=ORIENTED_EDGE('',*,*,#5458,.T.);
#7318=ORIENTED_EDGE('',*,*,#5459,.F.);
#7319=ORIENTED_EDGE('',*,*,#5460,.T.);
#7320=ORIENTED_EDGE('',*,*,#5461,.F.);
#7321=ORIENTED_EDGE('',*,*,#5462,.F.);
#7322=ORIENTED_EDGE('',*,*,#5463,.F.);
#7323=ORIENTED_EDGE('',*,*,#5464,.T.);
#7324=ORIENTED_EDGE('',*,*,#5465,.F.);
#7325=ORIENTED_EDGE('',*,*,#5466,.T.);
#7326=ORIENTED_EDGE('',*,*,#5467,.F.);
#7327=ORIENTED_EDGE('',*,*,#5468,.F.);
#7328=ORIENTED_EDGE('',*,*,#5469,.F.);
#7329=ORIENTED_EDGE('',*,*,#5470,.T.);
#7330=ORIENTED_EDGE('',*,*,#5471,.F.);
#7331=ORIENTED_EDGE('',*,*,#5472,.T.);
#7332=ORIENTED_EDGE('',*,*,#5473,.F.);
#7333=ORIENTED_EDGE('',*,*,#5474,.F.);
#7334=ORIENTED_EDGE('',*,*,#5475,.F.);
#7335=ORIENTED_EDGE('',*,*,#5476,.T.);
#7336=ORIENTED_EDGE('',*,*,#5477,.F.);
#7337=ORIENTED_EDGE('',*,*,#5478,.T.);
#7338=ORIENTED_EDGE('',*,*,#5479,.F.);
#7339=ORIENTED_EDGE('',*,*,#5480,.F.);
#7340=ORIENTED_EDGE('',*,*,#5481,.F.);
#7341=ORIENTED_EDGE('',*,*,#5482,.T.);
#7342=ORIENTED_EDGE('',*,*,#5483,.F.);
#7343=ORIENTED_EDGE('',*,*,#5484,.T.);
#7344=ORIENTED_EDGE('',*,*,#5485,.F.);
#7345=ORIENTED_EDGE('',*,*,#5486,.F.);
#7346=ORIENTED_EDGE('',*,*,#5487,.F.);
#7347=ORIENTED_EDGE('',*,*,#5488,.T.);
#7348=ORIENTED_EDGE('',*,*,#5489,.F.);
#7349=ORIENTED_EDGE('',*,*,#5490,.T.);
#7350=ORIENTED_EDGE('',*,*,#5491,.F.);
#7351=ORIENTED_EDGE('',*,*,#5492,.F.);
#7352=ORIENTED_EDGE('',*,*,#5493,.F.);
#7353=ORIENTED_EDGE('',*,*,#5494,.T.);
#7354=ORIENTED_EDGE('',*,*,#5495,.F.);
#7355=ORIENTED_EDGE('',*,*,#5496,.T.);
#7356=ORIENTED_EDGE('',*,*,#5497,.F.);
#7357=ORIENTED_EDGE('',*,*,#5498,.F.);
#7358=ORIENTED_EDGE('',*,*,#5499,.F.);
#7359=ORIENTED_EDGE('',*,*,#5500,.T.);
#7360=ORIENTED_EDGE('',*,*,#5501,.F.);
#7361=ORIENTED_EDGE('',*,*,#5502,.T.);
#7362=ORIENTED_EDGE('',*,*,#5503,.F.);
#7363=ORIENTED_EDGE('',*,*,#5504,.F.);
#7364=ORIENTED_EDGE('',*,*,#5505,.F.);
#7365=ORIENTED_EDGE('',*,*,#5506,.T.);
#7366=ORIENTED_EDGE('',*,*,#5507,.F.);
#7367=ORIENTED_EDGE('',*,*,#5508,.T.);
#7368=ORIENTED_EDGE('',*,*,#5509,.F.);
#7369=ORIENTED_EDGE('',*,*,#5510,.F.);
#7370=ORIENTED_EDGE('',*,*,#5511,.F.);
#7371=ORIENTED_EDGE('',*,*,#5512,.T.);
#7372=ORIENTED_EDGE('',*,*,#5513,.F.);
#7373=ORIENTED_EDGE('',*,*,#5514,.T.);
#7374=ORIENTED_EDGE('',*,*,#5515,.F.);
#7375=ORIENTED_EDGE('',*,*,#5516,.F.);
#7376=ORIENTED_EDGE('',*,*,#5517,.F.);
#7377=ORIENTED_EDGE('',*,*,#5518,.T.);
#7378=ORIENTED_EDGE('',*,*,#5519,.F.);
#7379=ORIENTED_EDGE('',*,*,#5520,.T.);
#7380=ORIENTED_EDGE('',*,*,#5521,.F.);
#7381=ORIENTED_EDGE('',*,*,#5522,.F.);
#7382=ORIENTED_EDGE('',*,*,#5523,.F.);
#7383=ORIENTED_EDGE('',*,*,#5524,.T.);
#7384=ORIENTED_EDGE('',*,*,#5525,.F.);
#7385=ORIENTED_EDGE('',*,*,#5526,.T.);
#7386=ORIENTED_EDGE('',*,*,#5527,.F.);
#7387=ORIENTED_EDGE('',*,*,#5528,.F.);
#7388=ORIENTED_EDGE('',*,*,#5529,.F.);
#7389=ORIENTED_EDGE('',*,*,#5530,.T.);
#7390=ORIENTED_EDGE('',*,*,#5531,.F.);
#7391=ORIENTED_EDGE('',*,*,#5532,.T.);
#7392=ORIENTED_EDGE('',*,*,#5533,.F.);
#7393=ORIENTED_EDGE('',*,*,#5534,.F.);
#7394=ORIENTED_EDGE('',*,*,#5535,.F.);
#7395=ORIENTED_EDGE('',*,*,#5536,.T.);
#7396=ORIENTED_EDGE('',*,*,#5537,.F.);
#7397=ORIENTED_EDGE('',*,*,#5538,.T.);
#7398=ORIENTED_EDGE('',*,*,#5539,.F.);
#7399=ORIENTED_EDGE('',*,*,#5540,.F.);
#7400=ORIENTED_EDGE('',*,*,#5541,.F.);
#7401=ORIENTED_EDGE('',*,*,#5542,.T.);
#7402=ORIENTED_EDGE('',*,*,#5543,.F.);
#7403=ORIENTED_EDGE('',*,*,#5544,.F.);
#7404=ORIENTED_EDGE('',*,*,#5545,.F.);
#7405=ORIENTED_EDGE('',*,*,#5546,.F.);
#7406=ORIENTED_EDGE('',*,*,#5547,.F.);
#7407=ORIENTED_EDGE('',*,*,#5548,.F.);
#7408=ORIENTED_EDGE('',*,*,#5549,.F.);
#7409=ORIENTED_EDGE('',*,*,#5550,.F.);
#7410=ORIENTED_EDGE('',*,*,#5551,.F.);
#7411=ORIENTED_EDGE('',*,*,#5552,.F.);
#7412=ORIENTED_EDGE('',*,*,#5553,.F.);
#7413=ORIENTED_EDGE('',*,*,#5554,.F.);
#7414=ORIENTED_EDGE('',*,*,#5555,.F.);
#7415=ORIENTED_EDGE('',*,*,#5556,.F.);
#7416=ORIENTED_EDGE('',*,*,#5557,.F.);
#7417=ORIENTED_EDGE('',*,*,#5558,.F.);
#7418=ORIENTED_EDGE('',*,*,#5559,.F.);
#7419=ORIENTED_EDGE('',*,*,#5560,.F.);
#7420=ORIENTED_EDGE('',*,*,#5561,.F.);
#7421=ORIENTED_EDGE('',*,*,#5562,.F.);
#7422=ORIENTED_EDGE('',*,*,#5563,.F.);
#7423=ORIENTED_EDGE('',*,*,#5564,.F.);
#7424=ORIENTED_EDGE('',*,*,#5565,.F.);
#7425=ORIENTED_EDGE('',*,*,#5566,.F.);
#7426=ORIENTED_EDGE('',*,*,#5567,.F.);
#7427=ORIENTED_EDGE('',*,*,#5568,.F.);
#7428=ORIENTED_EDGE('',*,*,#5569,.F.);
#7429=ORIENTED_EDGE('',*,*,#5570,.F.);
#7430=ORIENTED_EDGE('',*,*,#5571,.F.);
#7431=ORIENTED_EDGE('',*,*,#5572,.F.);
#7432=ORIENTED_EDGE('',*,*,#5573,.F.);
#7433=ORIENTED_EDGE('',*,*,#5574,.F.);
#7434=ORIENTED_EDGE('',*,*,#5575,.F.);
#7435=ORIENTED_EDGE('',*,*,#5576,.F.);
#7436=ORIENTED_EDGE('',*,*,#5577,.F.);
#7437=ORIENTED_EDGE('',*,*,#5578,.F.);
#7438=ORIENTED_EDGE('',*,*,#5579,.F.);
#7439=ORIENTED_EDGE('',*,*,#5580,.F.);
#7440=ORIENTED_EDGE('',*,*,#5581,.F.);
#7441=ORIENTED_EDGE('',*,*,#5582,.F.);
#7442=ORIENTED_EDGE('',*,*,#5583,.F.);
#7443=ORIENTED_EDGE('',*,*,#5584,.F.);
#7444=ORIENTED_EDGE('',*,*,#5585,.F.);
#7445=ORIENTED_EDGE('',*,*,#5586,.F.);
#7446=ORIENTED_EDGE('',*,*,#5587,.F.);
#7447=ORIENTED_EDGE('',*,*,#5588,.F.);
#7448=ORIENTED_EDGE('',*,*,#5589,.F.);
#7449=ORIENTED_EDGE('',*,*,#5590,.F.);
#7450=ORIENTED_EDGE('',*,*,#5591,.F.);
#7451=ORIENTED_EDGE('',*,*,#5592,.F.);
#7452=ORIENTED_EDGE('',*,*,#5593,.F.);
#7453=ORIENTED_EDGE('',*,*,#5594,.F.);
#7454=ORIENTED_EDGE('',*,*,#5595,.F.);
#7455=ORIENTED_EDGE('',*,*,#5596,.F.);
#7456=ORIENTED_EDGE('',*,*,#5597,.F.);
#7457=ORIENTED_EDGE('',*,*,#5598,.F.);
#7458=ORIENTED_EDGE('',*,*,#5599,.F.);
#7459=ORIENTED_EDGE('',*,*,#5600,.F.);
#7460=ORIENTED_EDGE('',*,*,#5601,.F.);
#7461=ORIENTED_EDGE('',*,*,#5602,.F.);
#7462=ORIENTED_EDGE('',*,*,#5603,.F.);
#7463=ORIENTED_EDGE('',*,*,#5604,.F.);
#7464=ORIENTED_EDGE('',*,*,#5605,.F.);
#7465=ORIENTED_EDGE('',*,*,#5606,.F.);
#7466=ORIENTED_EDGE('',*,*,#5607,.F.);
#7467=ORIENTED_EDGE('',*,*,#5608,.F.);
#7468=ORIENTED_EDGE('',*,*,#5609,.F.);
#7469=ORIENTED_EDGE('',*,*,#5610,.F.);
#7470=ORIENTED_EDGE('',*,*,#5611,.F.);
#7471=ORIENTED_EDGE('',*,*,#5612,.F.);
#7472=ORIENTED_EDGE('',*,*,#5613,.F.);
#7473=ORIENTED_EDGE('',*,*,#5614,.F.);
#7474=ORIENTED_EDGE('',*,*,#5615,.F.);
#7475=ORIENTED_EDGE('',*,*,#5616,.F.);
#7476=ORIENTED_EDGE('',*,*,#5617,.F.);
#7477=ORIENTED_EDGE('',*,*,#5618,.F.);
#7478=ORIENTED_EDGE('',*,*,#5619,.F.);
#7479=ORIENTED_EDGE('',*,*,#5620,.F.);
#7480=ORIENTED_EDGE('',*,*,#5621,.F.);
#7481=ORIENTED_EDGE('',*,*,#5622,.F.);
#7482=ORIENTED_EDGE('',*,*,#5623,.F.);
#7483=ORIENTED_EDGE('',*,*,#5624,.F.);
#7484=ORIENTED_EDGE('',*,*,#5625,.F.);
#7485=ORIENTED_EDGE('',*,*,#5626,.F.);
#7486=ORIENTED_EDGE('',*,*,#5627,.F.);
#7487=ORIENTED_EDGE('',*,*,#5628,.F.);
#7488=ORIENTED_EDGE('',*,*,#5629,.F.);
#7489=ORIENTED_EDGE('',*,*,#5630,.F.);
#7490=ORIENTED_EDGE('',*,*,#5631,.F.);
#7491=ORIENTED_EDGE('',*,*,#5632,.F.);
#7492=ORIENTED_EDGE('',*,*,#5633,.T.);
#7493=ORIENTED_EDGE('',*,*,#5634,.F.);
#7494=ORIENTED_EDGE('',*,*,#5633,.F.);
#7495=ORIENTED_EDGE('',*,*,#5635,.F.);
#7496=ORIENTED_EDGE('',*,*,#5636,.F.);
#7497=ORIENTED_EDGE('',*,*,#5637,.F.);
#7498=ORIENTED_EDGE('',*,*,#5638,.F.);
#7499=ORIENTED_EDGE('',*,*,#5639,.F.);
#7500=ORIENTED_EDGE('',*,*,#5640,.F.);
#7501=ORIENTED_EDGE('',*,*,#5641,.F.);
#7502=ORIENTED_EDGE('',*,*,#5642,.F.);
#7503=ORIENTED_EDGE('',*,*,#5643,.F.);
#7504=ORIENTED_EDGE('',*,*,#5644,.F.);
#7505=ORIENTED_EDGE('',*,*,#5645,.F.);
#7506=ORIENTED_EDGE('',*,*,#5646,.F.);
#7507=ORIENTED_EDGE('',*,*,#5647,.F.);
#7508=ORIENTED_EDGE('',*,*,#5648,.F.);
#7509=ORIENTED_EDGE('',*,*,#5649,.F.);
#7510=ORIENTED_EDGE('',*,*,#5650,.F.);
#7511=ORIENTED_EDGE('',*,*,#5651,.F.);
#7512=ORIENTED_EDGE('',*,*,#5652,.F.);
#7513=ORIENTED_EDGE('',*,*,#5653,.F.);
#7514=ORIENTED_EDGE('',*,*,#5654,.F.);
#7515=ORIENTED_EDGE('',*,*,#5655,.F.);
#7516=ORIENTED_EDGE('',*,*,#5656,.F.);
#7517=ORIENTED_EDGE('',*,*,#5657,.F.);
#7518=ORIENTED_EDGE('',*,*,#5658,.F.);
#7519=ORIENTED_EDGE('',*,*,#5659,.F.);
#7520=ORIENTED_EDGE('',*,*,#5660,.F.);
#7521=ORIENTED_EDGE('',*,*,#5661,.F.);
#7522=ORIENTED_EDGE('',*,*,#5662,.F.);
#7523=ORIENTED_EDGE('',*,*,#5663,.F.);
#7524=ORIENTED_EDGE('',*,*,#5664,.F.);
#7525=ORIENTED_EDGE('',*,*,#5665,.F.);
#7526=ORIENTED_EDGE('',*,*,#5666,.F.);
#7527=ORIENTED_EDGE('',*,*,#5667,.F.);
#7528=ORIENTED_EDGE('',*,*,#5668,.F.);
#7529=ORIENTED_EDGE('',*,*,#5669,.F.);
#7530=ORIENTED_EDGE('',*,*,#5670,.F.);
#7531=ORIENTED_EDGE('',*,*,#5671,.F.);
#7532=ORIENTED_EDGE('',*,*,#5672,.F.);
#7533=ORIENTED_EDGE('',*,*,#5673,.F.);
#7534=ORIENTED_EDGE('',*,*,#5674,.F.);
#7535=ORIENTED_EDGE('',*,*,#5675,.F.);
#7536=ORIENTED_EDGE('',*,*,#5676,.F.);
#7537=ORIENTED_EDGE('',*,*,#5677,.F.);
#7538=ORIENTED_EDGE('',*,*,#5678,.F.);
#7539=ORIENTED_EDGE('',*,*,#5679,.F.);
#7540=ORIENTED_EDGE('',*,*,#5680,.F.);
#7541=ORIENTED_EDGE('',*,*,#5681,.F.);
#7542=ORIENTED_EDGE('',*,*,#5682,.F.);
#7543=ORIENTED_EDGE('',*,*,#5683,.F.);
#7544=ORIENTED_EDGE('',*,*,#5684,.F.);
#7545=ORIENTED_EDGE('',*,*,#5685,.F.);
#7546=ORIENTED_EDGE('',*,*,#5686,.F.);
#7547=ORIENTED_EDGE('',*,*,#5687,.F.);
#7548=ORIENTED_EDGE('',*,*,#5688,.F.);
#7549=ORIENTED_EDGE('',*,*,#5689,.F.);
#7550=ORIENTED_EDGE('',*,*,#5690,.F.);
#7551=ORIENTED_EDGE('',*,*,#5691,.F.);
#7552=ORIENTED_EDGE('',*,*,#5692,.F.);
#7553=ORIENTED_EDGE('',*,*,#5693,.F.);
#7554=ORIENTED_EDGE('',*,*,#5694,.F.);
#7555=ORIENTED_EDGE('',*,*,#5695,.F.);
#7556=ORIENTED_EDGE('',*,*,#5696,.F.);
#7557=ORIENTED_EDGE('',*,*,#5697,.F.);
#7558=ORIENTED_EDGE('',*,*,#5698,.F.);
#7559=ORIENTED_EDGE('',*,*,#5699,.F.);
#7560=ORIENTED_EDGE('',*,*,#5700,.F.);
#7561=ORIENTED_EDGE('',*,*,#5701,.F.);
#7562=ORIENTED_EDGE('',*,*,#5702,.F.);
#7563=ORIENTED_EDGE('',*,*,#5703,.F.);
#7564=ORIENTED_EDGE('',*,*,#5704,.F.);
#7565=ORIENTED_EDGE('',*,*,#5705,.F.);
#7566=ORIENTED_EDGE('',*,*,#5706,.F.);
#7567=ORIENTED_EDGE('',*,*,#5707,.F.);
#7568=ORIENTED_EDGE('',*,*,#5708,.F.);
#7569=ORIENTED_EDGE('',*,*,#5709,.F.);
#7570=ORIENTED_EDGE('',*,*,#5710,.F.);
#7571=ORIENTED_EDGE('',*,*,#5711,.F.);
#7572=ORIENTED_EDGE('',*,*,#5712,.F.);
#7573=ORIENTED_EDGE('',*,*,#5713,.F.);
#7574=ORIENTED_EDGE('',*,*,#5714,.F.);
#7575=ORIENTED_EDGE('',*,*,#5715,.F.);
#7576=ORIENTED_EDGE('',*,*,#5716,.F.);
#7577=ORIENTED_EDGE('',*,*,#5717,.F.);
#7578=ORIENTED_EDGE('',*,*,#5718,.F.);
#7579=ORIENTED_EDGE('',*,*,#5719,.F.);
#7580=ORIENTED_EDGE('',*,*,#5720,.F.);
#7581=ORIENTED_EDGE('',*,*,#5721,.F.);
#7582=ORIENTED_EDGE('',*,*,#5722,.F.);
#7583=ORIENTED_EDGE('',*,*,#5723,.T.);
#7584=ORIENTED_EDGE('',*,*,#5724,.T.);
#7585=ORIENTED_EDGE('',*,*,#5725,.F.);
#7586=ORIENTED_EDGE('',*,*,#5726,.F.);
#7587=ORIENTED_EDGE('',*,*,#5727,.T.);
#7588=ORIENTED_EDGE('',*,*,#5728,.T.);
#7589=ORIENTED_EDGE('',*,*,#5729,.F.);
#7590=ORIENTED_EDGE('',*,*,#5730,.T.);
#7591=ORIENTED_EDGE('',*,*,#5731,.T.);
#7592=ORIENTED_EDGE('',*,*,#5732,.T.);
#7593=ORIENTED_EDGE('',*,*,#5733,.F.);
#7594=ORIENTED_EDGE('',*,*,#5734,.T.);
#7595=ORIENTED_EDGE('',*,*,#5735,.T.);
#7596=ORIENTED_EDGE('',*,*,#5736,.T.);
#7597=ORIENTED_EDGE('',*,*,#5737,.F.);
#7598=ORIENTED_EDGE('',*,*,#5738,.T.);
#7599=ORIENTED_EDGE('',*,*,#5739,.T.);
#7600=ORIENTED_EDGE('',*,*,#5740,.T.);
#7601=ORIENTED_EDGE('',*,*,#5741,.F.);
#7602=ORIENTED_EDGE('',*,*,#5742,.T.);
#7603=ORIENTED_EDGE('',*,*,#5743,.T.);
#7604=ORIENTED_EDGE('',*,*,#5744,.T.);
#7605=ORIENTED_EDGE('',*,*,#5745,.F.);
#7606=ORIENTED_EDGE('',*,*,#5746,.T.);
#7607=ORIENTED_EDGE('',*,*,#5747,.T.);
#7608=ORIENTED_EDGE('',*,*,#5748,.T.);
#7609=ORIENTED_EDGE('',*,*,#5749,.F.);
#7610=ORIENTED_EDGE('',*,*,#5750,.T.);
#7611=ORIENTED_EDGE('',*,*,#5751,.T.);
#7612=ORIENTED_EDGE('',*,*,#5752,.T.);
#7613=ORIENTED_EDGE('',*,*,#5753,.F.);
#7614=ORIENTED_EDGE('',*,*,#5754,.T.);
#7615=ORIENTED_EDGE('',*,*,#5755,.T.);
#7616=ORIENTED_EDGE('',*,*,#5756,.T.);
#7617=ORIENTED_EDGE('',*,*,#5757,.F.);
#7618=ORIENTED_EDGE('',*,*,#5758,.T.);
#7619=ORIENTED_EDGE('',*,*,#5759,.T.);
#7620=ORIENTED_EDGE('',*,*,#5760,.T.);
#7621=ORIENTED_EDGE('',*,*,#5761,.F.);
#7622=ORIENTED_EDGE('',*,*,#5762,.T.);
#7623=ORIENTED_EDGE('',*,*,#5763,.T.);
#7624=ORIENTED_EDGE('',*,*,#5764,.T.);
#7625=ORIENTED_EDGE('',*,*,#5765,.F.);
#7626=ORIENTED_EDGE('',*,*,#5766,.T.);
#7627=ORIENTED_EDGE('',*,*,#5767,.T.);
#7628=ORIENTED_EDGE('',*,*,#5768,.T.);
#7629=ORIENTED_EDGE('',*,*,#5769,.F.);
#7630=ORIENTED_EDGE('',*,*,#5770,.T.);
#7631=ORIENTED_EDGE('',*,*,#5771,.T.);
#7632=ORIENTED_EDGE('',*,*,#5772,.T.);
#7633=ORIENTED_EDGE('',*,*,#5773,.F.);
#7634=ORIENTED_EDGE('',*,*,#5774,.T.);
#7635=ORIENTED_EDGE('',*,*,#5775,.T.);
#7636=ORIENTED_EDGE('',*,*,#5776,.T.);
#7637=ORIENTED_EDGE('',*,*,#5777,.F.);
#7638=ORIENTED_EDGE('',*,*,#5778,.T.);
#7639=ORIENTED_EDGE('',*,*,#5779,.T.);
#7640=ORIENTED_EDGE('',*,*,#5780,.T.);
#7641=ORIENTED_EDGE('',*,*,#5781,.F.);
#7642=ORIENTED_EDGE('',*,*,#5782,.T.);
#7643=ORIENTED_EDGE('',*,*,#5783,.T.);
#7644=ORIENTED_EDGE('',*,*,#5784,.T.);
#7645=ORIENTED_EDGE('',*,*,#5785,.F.);
#7646=ORIENTED_EDGE('',*,*,#5786,.T.);
#7647=ORIENTED_EDGE('',*,*,#5787,.T.);
#7648=ORIENTED_EDGE('',*,*,#5788,.T.);
#7649=ORIENTED_EDGE('',*,*,#5789,.F.);
#7650=ORIENTED_EDGE('',*,*,#5790,.T.);
#7651=ORIENTED_EDGE('',*,*,#5791,.T.);
#7652=ORIENTED_EDGE('',*,*,#5792,.T.);
#7653=ORIENTED_EDGE('',*,*,#5793,.F.);
#7654=ORIENTED_EDGE('',*,*,#5794,.T.);
#7655=ORIENTED_EDGE('',*,*,#5795,.T.);
#7656=ORIENTED_EDGE('',*,*,#5796,.T.);
#7657=ORIENTED_EDGE('',*,*,#5797,.F.);
#7658=ORIENTED_EDGE('',*,*,#5798,.T.);
#7659=ORIENTED_EDGE('',*,*,#5799,.T.);
#7660=ORIENTED_EDGE('',*,*,#5800,.T.);
#7661=ORIENTED_EDGE('',*,*,#5801,.F.);
#7662=ORIENTED_EDGE('',*,*,#5802,.T.);
#7663=ORIENTED_EDGE('',*,*,#5803,.T.);
#7664=ORIENTED_EDGE('',*,*,#5804,.T.);
#7665=ORIENTED_EDGE('',*,*,#5805,.F.);
#7666=ORIENTED_EDGE('',*,*,#5806,.T.);
#7667=ORIENTED_EDGE('',*,*,#5807,.T.);
#7668=ORIENTED_EDGE('',*,*,#5808,.T.);
#7669=ORIENTED_EDGE('',*,*,#5809,.F.);
#7670=ORIENTED_EDGE('',*,*,#5810,.T.);
#7671=ORIENTED_EDGE('',*,*,#5811,.T.);
#7672=ORIENTED_EDGE('',*,*,#5812,.T.);
#7673=ORIENTED_EDGE('',*,*,#5813,.F.);
#7674=ORIENTED_EDGE('',*,*,#5814,.T.);
#7675=ORIENTED_EDGE('',*,*,#5815,.T.);
#7676=ORIENTED_EDGE('',*,*,#5816,.T.);
#7677=ORIENTED_EDGE('',*,*,#5817,.F.);
#7678=ORIENTED_EDGE('',*,*,#5816,.F.);
#7679=ORIENTED_EDGE('',*,*,#5818,.T.);
#7680=ORIENTED_EDGE('',*,*,#5819,.T.);
#7681=ORIENTED_EDGE('',*,*,#5820,.F.);
#7682=ORIENTED_EDGE('',*,*,#5821,.T.);
#7683=ORIENTED_EDGE('',*,*,#5822,.T.);
#7684=ORIENTED_EDGE('',*,*,#5823,.T.);
#7685=ORIENTED_EDGE('',*,*,#5824,.F.);
#7686=ORIENTED_EDGE('',*,*,#5825,.T.);
#7687=ORIENTED_EDGE('',*,*,#5826,.T.);
#7688=ORIENTED_EDGE('',*,*,#5827,.T.);
#7689=ORIENTED_EDGE('',*,*,#5828,.F.);
#7690=ORIENTED_EDGE('',*,*,#5829,.T.);
#7691=ORIENTED_EDGE('',*,*,#5830,.T.);
#7692=ORIENTED_EDGE('',*,*,#5831,.T.);
#7693=ORIENTED_EDGE('',*,*,#5832,.F.);
#7694=ORIENTED_EDGE('',*,*,#5833,.T.);
#7695=ORIENTED_EDGE('',*,*,#5834,.T.);
#7696=ORIENTED_EDGE('',*,*,#5835,.T.);
#7697=ORIENTED_EDGE('',*,*,#5836,.F.);
#7698=ORIENTED_EDGE('',*,*,#5837,.T.);
#7699=ORIENTED_EDGE('',*,*,#5838,.T.);
#7700=ORIENTED_EDGE('',*,*,#5839,.T.);
#7701=ORIENTED_EDGE('',*,*,#5840,.F.);
#7702=ORIENTED_EDGE('',*,*,#5841,.T.);
#7703=ORIENTED_EDGE('',*,*,#5842,.T.);
#7704=ORIENTED_EDGE('',*,*,#5843,.T.);
#7705=ORIENTED_EDGE('',*,*,#5844,.F.);
#7706=ORIENTED_EDGE('',*,*,#5845,.T.);
#7707=ORIENTED_EDGE('',*,*,#5846,.T.);
#7708=ORIENTED_EDGE('',*,*,#5847,.T.);
#7709=ORIENTED_EDGE('',*,*,#5848,.F.);
#7710=ORIENTED_EDGE('',*,*,#5849,.T.);
#7711=ORIENTED_EDGE('',*,*,#5850,.T.);
#7712=ORIENTED_EDGE('',*,*,#5851,.T.);
#7713=ORIENTED_EDGE('',*,*,#5852,.F.);
#7714=ORIENTED_EDGE('',*,*,#5853,.T.);
#7715=ORIENTED_EDGE('',*,*,#5854,.T.);
#7716=ORIENTED_EDGE('',*,*,#5855,.T.);
#7717=ORIENTED_EDGE('',*,*,#5856,.F.);
#7718=ORIENTED_EDGE('',*,*,#5857,.T.);
#7719=ORIENTED_EDGE('',*,*,#5858,.T.);
#7720=ORIENTED_EDGE('',*,*,#5859,.T.);
#7721=ORIENTED_EDGE('',*,*,#5860,.F.);
#7722=ORIENTED_EDGE('',*,*,#5861,.T.);
#7723=ORIENTED_EDGE('',*,*,#5862,.T.);
#7724=ORIENTED_EDGE('',*,*,#5863,.T.);
#7725=ORIENTED_EDGE('',*,*,#5864,.F.);
#7726=ORIENTED_EDGE('',*,*,#5865,.T.);
#7727=ORIENTED_EDGE('',*,*,#5866,.T.);
#7728=ORIENTED_EDGE('',*,*,#5867,.T.);
#7729=ORIENTED_EDGE('',*,*,#5868,.F.);
#7730=ORIENTED_EDGE('',*,*,#5869,.T.);
#7731=ORIENTED_EDGE('',*,*,#5870,.T.);
#7732=ORIENTED_EDGE('',*,*,#5871,.T.);
#7733=ORIENTED_EDGE('',*,*,#5872,.F.);
#7734=ORIENTED_EDGE('',*,*,#5873,.T.);
#7735=ORIENTED_EDGE('',*,*,#5874,.T.);
#7736=ORIENTED_EDGE('',*,*,#5875,.T.);
#7737=ORIENTED_EDGE('',*,*,#5876,.F.);
#7738=ORIENTED_EDGE('',*,*,#5877,.T.);
#7739=ORIENTED_EDGE('',*,*,#5878,.T.);
#7740=ORIENTED_EDGE('',*,*,#5879,.T.);
#7741=ORIENTED_EDGE('',*,*,#5880,.F.);
#7742=ORIENTED_EDGE('',*,*,#5881,.T.);
#7743=ORIENTED_EDGE('',*,*,#5882,.T.);
#7744=ORIENTED_EDGE('',*,*,#5883,.T.);
#7745=ORIENTED_EDGE('',*,*,#5884,.F.);
#7746=ORIENTED_EDGE('',*,*,#5885,.T.);
#7747=ORIENTED_EDGE('',*,*,#5886,.T.);
#7748=ORIENTED_EDGE('',*,*,#5887,.T.);
#7749=ORIENTED_EDGE('',*,*,#5888,.F.);
#7750=ORIENTED_EDGE('',*,*,#5889,.T.);
#7751=ORIENTED_EDGE('',*,*,#5890,.T.);
#7752=ORIENTED_EDGE('',*,*,#5891,.T.);
#7753=ORIENTED_EDGE('',*,*,#5892,.F.);
#7754=ORIENTED_EDGE('',*,*,#5893,.T.);
#7755=ORIENTED_EDGE('',*,*,#5894,.T.);
#7756=ORIENTED_EDGE('',*,*,#5895,.T.);
#7757=ORIENTED_EDGE('',*,*,#5896,.F.);
#7758=ORIENTED_EDGE('',*,*,#5897,.T.);
#7759=ORIENTED_EDGE('',*,*,#5898,.T.);
#7760=ORIENTED_EDGE('',*,*,#5899,.T.);
#7761=ORIENTED_EDGE('',*,*,#5900,.F.);
#7762=ORIENTED_EDGE('',*,*,#5901,.T.);
#7763=ORIENTED_EDGE('',*,*,#5902,.T.);
#7764=ORIENTED_EDGE('',*,*,#5903,.T.);
#7765=ORIENTED_EDGE('',*,*,#5904,.F.);
#7766=ORIENTED_EDGE('',*,*,#5905,.T.);
#7767=ORIENTED_EDGE('',*,*,#5906,.F.);
#7768=ORIENTED_EDGE('',*,*,#5765,.T.);
#7769=ORIENTED_EDGE('',*,*,#5907,.F.);
#7770=ORIENTED_EDGE('',*,*,#5540,.T.);
#7771=ORIENTED_EDGE('',*,*,#5908,.F.);
#7772=ORIENTED_EDGE('',*,*,#5534,.T.);
#7773=ORIENTED_EDGE('',*,*,#5909,.F.);
#7774=ORIENTED_EDGE('',*,*,#5769,.T.);
#7775=ORIENTED_EDGE('',*,*,#5910,.F.);
#7776=ORIENTED_EDGE('',*,*,#5761,.T.);
#7777=ORIENTED_EDGE('',*,*,#5911,.F.);
#7778=ORIENTED_EDGE('',*,*,#5528,.T.);
#7779=ORIENTED_EDGE('',*,*,#5912,.F.);
#7780=ORIENTED_EDGE('',*,*,#5757,.T.);
#7781=ORIENTED_EDGE('',*,*,#5913,.F.);
#7782=ORIENTED_EDGE('',*,*,#5522,.T.);
#7783=ORIENTED_EDGE('',*,*,#5914,.F.);
#7784=ORIENTED_EDGE('',*,*,#5753,.T.);
#7785=ORIENTED_EDGE('',*,*,#5915,.F.);
#7786=ORIENTED_EDGE('',*,*,#5516,.T.);
#7787=ORIENTED_EDGE('',*,*,#5916,.F.);
#7788=ORIENTED_EDGE('',*,*,#5749,.T.);
#7789=ORIENTED_EDGE('',*,*,#5917,.F.);
#7790=ORIENTED_EDGE('',*,*,#5510,.T.);
#7791=ORIENTED_EDGE('',*,*,#5918,.F.);
#7792=ORIENTED_EDGE('',*,*,#5745,.T.);
#7793=ORIENTED_EDGE('',*,*,#5919,.F.);
#7794=ORIENTED_EDGE('',*,*,#5504,.T.);
#7795=ORIENTED_EDGE('',*,*,#5920,.F.);
#7796=ORIENTED_EDGE('',*,*,#5741,.T.);
#7797=ORIENTED_EDGE('',*,*,#5921,.F.);
#7798=ORIENTED_EDGE('',*,*,#5498,.T.);
#7799=ORIENTED_EDGE('',*,*,#5922,.F.);
#7800=ORIENTED_EDGE('',*,*,#5737,.T.);
#7801=ORIENTED_EDGE('',*,*,#5923,.F.);
#7802=ORIENTED_EDGE('',*,*,#5492,.T.);
#7803=ORIENTED_EDGE('',*,*,#5924,.F.);
#7804=ORIENTED_EDGE('',*,*,#5733,.T.);
#7805=ORIENTED_EDGE('',*,*,#5925,.F.);
#7806=ORIENTED_EDGE('',*,*,#5486,.T.);
#7807=ORIENTED_EDGE('',*,*,#5926,.F.);
#7808=ORIENTED_EDGE('',*,*,#5729,.T.);
#7809=ORIENTED_EDGE('',*,*,#5927,.F.);
#7810=ORIENTED_EDGE('',*,*,#5480,.T.);
#7811=ORIENTED_EDGE('',*,*,#5928,.F.);
#7812=ORIENTED_EDGE('',*,*,#5904,.T.);
#7813=ORIENTED_EDGE('',*,*,#5929,.F.);
#7814=ORIENTED_EDGE('',*,*,#5474,.T.);
#7815=ORIENTED_EDGE('',*,*,#5930,.F.);
#7816=ORIENTED_EDGE('',*,*,#5900,.T.);
#7817=ORIENTED_EDGE('',*,*,#5931,.F.);
#7818=ORIENTED_EDGE('',*,*,#5468,.T.);
#7819=ORIENTED_EDGE('',*,*,#5932,.F.);
#7820=ORIENTED_EDGE('',*,*,#5896,.T.);
#7821=ORIENTED_EDGE('',*,*,#5933,.F.);
#7822=ORIENTED_EDGE('',*,*,#5462,.T.);
#7823=ORIENTED_EDGE('',*,*,#5934,.F.);
#7824=ORIENTED_EDGE('',*,*,#5892,.T.);
#7825=ORIENTED_EDGE('',*,*,#5935,.F.);
#7826=ORIENTED_EDGE('',*,*,#5456,.T.);
#7827=ORIENTED_EDGE('',*,*,#5936,.F.);
#7828=ORIENTED_EDGE('',*,*,#5888,.T.);
#7829=ORIENTED_EDGE('',*,*,#5937,.F.);
#7830=ORIENTED_EDGE('',*,*,#5450,.T.);
#7831=ORIENTED_EDGE('',*,*,#5938,.F.);
#7832=ORIENTED_EDGE('',*,*,#5884,.T.);
#7833=ORIENTED_EDGE('',*,*,#5939,.F.);
#7834=ORIENTED_EDGE('',*,*,#5444,.T.);
#7835=ORIENTED_EDGE('',*,*,#5940,.F.);
#7836=ORIENTED_EDGE('',*,*,#5880,.T.);
#7837=ORIENTED_EDGE('',*,*,#5941,.F.);
#7838=ORIENTED_EDGE('',*,*,#5438,.T.);
#7839=ORIENTED_EDGE('',*,*,#5942,.F.);
#7840=ORIENTED_EDGE('',*,*,#5876,.T.);
#7841=ORIENTED_EDGE('',*,*,#5943,.F.);
#7842=ORIENTED_EDGE('',*,*,#5432,.T.);
#7843=ORIENTED_EDGE('',*,*,#5944,.F.);
#7844=ORIENTED_EDGE('',*,*,#5872,.T.);
#7845=ORIENTED_EDGE('',*,*,#5945,.F.);
#7846=ORIENTED_EDGE('',*,*,#5426,.T.);
#7847=ORIENTED_EDGE('',*,*,#5946,.F.);
#7848=ORIENTED_EDGE('',*,*,#5868,.T.);
#7849=ORIENTED_EDGE('',*,*,#5947,.F.);
#7850=ORIENTED_EDGE('',*,*,#5420,.T.);
#7851=ORIENTED_EDGE('',*,*,#5948,.F.);
#7852=ORIENTED_EDGE('',*,*,#5864,.T.);
#7853=ORIENTED_EDGE('',*,*,#5949,.F.);
#7854=ORIENTED_EDGE('',*,*,#5414,.T.);
#7855=ORIENTED_EDGE('',*,*,#5950,.F.);
#7856=ORIENTED_EDGE('',*,*,#5860,.T.);
#7857=ORIENTED_EDGE('',*,*,#5951,.F.);
#7858=ORIENTED_EDGE('',*,*,#5408,.T.);
#7859=ORIENTED_EDGE('',*,*,#5952,.F.);
#7860=ORIENTED_EDGE('',*,*,#5856,.T.);
#7861=ORIENTED_EDGE('',*,*,#5953,.F.);
#7862=ORIENTED_EDGE('',*,*,#5402,.T.);
#7863=ORIENTED_EDGE('',*,*,#5954,.F.);
#7864=ORIENTED_EDGE('',*,*,#5852,.T.);
#7865=ORIENTED_EDGE('',*,*,#5955,.F.);
#7866=ORIENTED_EDGE('',*,*,#5396,.T.);
#7867=ORIENTED_EDGE('',*,*,#5956,.F.);
#7868=ORIENTED_EDGE('',*,*,#5848,.T.);
#7869=ORIENTED_EDGE('',*,*,#5957,.F.);
#7870=ORIENTED_EDGE('',*,*,#5390,.T.);
#7871=ORIENTED_EDGE('',*,*,#5958,.F.);
#7872=ORIENTED_EDGE('',*,*,#5844,.T.);
#7873=ORIENTED_EDGE('',*,*,#5959,.F.);
#7874=ORIENTED_EDGE('',*,*,#5384,.T.);
#7875=ORIENTED_EDGE('',*,*,#5960,.F.);
#7876=ORIENTED_EDGE('',*,*,#5840,.T.);
#7877=ORIENTED_EDGE('',*,*,#5961,.F.);
#7878=ORIENTED_EDGE('',*,*,#5378,.T.);
#7879=ORIENTED_EDGE('',*,*,#5962,.F.);
#7880=ORIENTED_EDGE('',*,*,#5836,.T.);
#7881=ORIENTED_EDGE('',*,*,#5963,.F.);
#7882=ORIENTED_EDGE('',*,*,#5372,.T.);
#7883=ORIENTED_EDGE('',*,*,#5964,.F.);
#7884=ORIENTED_EDGE('',*,*,#5832,.T.);
#7885=ORIENTED_EDGE('',*,*,#5965,.F.);
#7886=ORIENTED_EDGE('',*,*,#5366,.T.);
#7887=ORIENTED_EDGE('',*,*,#5966,.F.);
#7888=ORIENTED_EDGE('',*,*,#5828,.T.);
#7889=ORIENTED_EDGE('',*,*,#5967,.F.);
#7890=ORIENTED_EDGE('',*,*,#5360,.T.);
#7891=ORIENTED_EDGE('',*,*,#5968,.F.);
#7892=ORIENTED_EDGE('',*,*,#5824,.T.);
#7893=ORIENTED_EDGE('',*,*,#5969,.F.);
#7894=ORIENTED_EDGE('',*,*,#5354,.T.);
#7895=ORIENTED_EDGE('',*,*,#5970,.F.);
#7896=ORIENTED_EDGE('',*,*,#5820,.T.);
#7897=ORIENTED_EDGE('',*,*,#5971,.F.);
#7898=ORIENTED_EDGE('',*,*,#5348,.T.);
#7899=ORIENTED_EDGE('',*,*,#5972,.F.);
#7900=ORIENTED_EDGE('',*,*,#5813,.T.);
#7901=ORIENTED_EDGE('',*,*,#5973,.F.);
#7902=ORIENTED_EDGE('',*,*,#5342,.T.);
#7903=ORIENTED_EDGE('',*,*,#5974,.F.);
#7904=ORIENTED_EDGE('',*,*,#5809,.T.);
#7905=ORIENTED_EDGE('',*,*,#5975,.F.);
#7906=ORIENTED_EDGE('',*,*,#5336,.T.);
#7907=ORIENTED_EDGE('',*,*,#5976,.F.);
#7908=ORIENTED_EDGE('',*,*,#5805,.T.);
#7909=ORIENTED_EDGE('',*,*,#5977,.F.);
#7910=ORIENTED_EDGE('',*,*,#5330,.T.);
#7911=ORIENTED_EDGE('',*,*,#5978,.F.);
#7912=ORIENTED_EDGE('',*,*,#5801,.T.);
#7913=ORIENTED_EDGE('',*,*,#5979,.F.);
#7914=ORIENTED_EDGE('',*,*,#5324,.T.);
#7915=ORIENTED_EDGE('',*,*,#5980,.F.);
#7916=ORIENTED_EDGE('',*,*,#5797,.T.);
#7917=ORIENTED_EDGE('',*,*,#5981,.F.);
#7918=ORIENTED_EDGE('',*,*,#5318,.T.);
#7919=ORIENTED_EDGE('',*,*,#5982,.F.);
#7920=ORIENTED_EDGE('',*,*,#5793,.T.);
#7921=ORIENTED_EDGE('',*,*,#5983,.F.);
#7922=ORIENTED_EDGE('',*,*,#5312,.T.);
#7923=ORIENTED_EDGE('',*,*,#5984,.F.);
#7924=ORIENTED_EDGE('',*,*,#5789,.T.);
#7925=ORIENTED_EDGE('',*,*,#5985,.F.);
#7926=ORIENTED_EDGE('',*,*,#5306,.T.);
#7927=ORIENTED_EDGE('',*,*,#5986,.F.);
#7928=ORIENTED_EDGE('',*,*,#5785,.T.);
#7929=ORIENTED_EDGE('',*,*,#5987,.F.);
#7930=ORIENTED_EDGE('',*,*,#5300,.T.);
#7931=ORIENTED_EDGE('',*,*,#5988,.F.);
#7932=ORIENTED_EDGE('',*,*,#5781,.T.);
#7933=ORIENTED_EDGE('',*,*,#5989,.F.);
#7934=ORIENTED_EDGE('',*,*,#5294,.T.);
#7935=ORIENTED_EDGE('',*,*,#5990,.F.);
#7936=ORIENTED_EDGE('',*,*,#5777,.T.);
#7937=ORIENTED_EDGE('',*,*,#5991,.F.);
#7938=ORIENTED_EDGE('',*,*,#5288,.T.);
#7939=ORIENTED_EDGE('',*,*,#5992,.F.);
#7940=ORIENTED_EDGE('',*,*,#5773,.T.);
#7941=ORIENTED_EDGE('',*,*,#5993,.F.);
#7942=ORIENTED_EDGE('',*,*,#5282,.T.);
#7943=ORIENTED_EDGE('',*,*,#5537,.T.);
#7944=ORIENTED_EDGE('',*,*,#5994,.T.);
#7945=ORIENTED_EDGE('',*,*,#5590,.T.);
#7946=ORIENTED_EDGE('',*,*,#5995,.T.);
#7947=ORIENTED_EDGE('',*,*,#5594,.T.);
#7948=ORIENTED_EDGE('',*,*,#5996,.T.);
#7949=ORIENTED_EDGE('',*,*,#5543,.T.);
#7950=ORIENTED_EDGE('',*,*,#5997,.T.);
#7951=ORIENTED_EDGE('',*,*,#5598,.T.);
#7952=ORIENTED_EDGE('',*,*,#5998,.T.);
#7953=ORIENTED_EDGE('',*,*,#5531,.T.);
#7954=ORIENTED_EDGE('',*,*,#5999,.T.);
#7955=ORIENTED_EDGE('',*,*,#5602,.T.);
#7956=ORIENTED_EDGE('',*,*,#6000,.T.);
#7957=ORIENTED_EDGE('',*,*,#5525,.T.);
#7958=ORIENTED_EDGE('',*,*,#6001,.T.);
#7959=ORIENTED_EDGE('',*,*,#5606,.T.);
#7960=ORIENTED_EDGE('',*,*,#6002,.T.);
#7961=ORIENTED_EDGE('',*,*,#5519,.T.);
#7962=ORIENTED_EDGE('',*,*,#6003,.T.);
#7963=ORIENTED_EDGE('',*,*,#5610,.T.);
#7964=ORIENTED_EDGE('',*,*,#6004,.T.);
#7965=ORIENTED_EDGE('',*,*,#5513,.T.);
#7966=ORIENTED_EDGE('',*,*,#6005,.T.);
#7967=ORIENTED_EDGE('',*,*,#5618,.T.);
#7968=ORIENTED_EDGE('',*,*,#6006,.T.);
#7969=ORIENTED_EDGE('',*,*,#5501,.T.);
#7970=ORIENTED_EDGE('',*,*,#6007,.T.);
#7971=ORIENTED_EDGE('',*,*,#5614,.T.);
#7972=ORIENTED_EDGE('',*,*,#6008,.T.);
#7973=ORIENTED_EDGE('',*,*,#5507,.T.);
#7974=ORIENTED_EDGE('',*,*,#6009,.T.);
#7975=ORIENTED_EDGE('',*,*,#5622,.T.);
#7976=ORIENTED_EDGE('',*,*,#6010,.T.);
#7977=ORIENTED_EDGE('',*,*,#5495,.T.);
#7978=ORIENTED_EDGE('',*,*,#6011,.T.);
#7979=ORIENTED_EDGE('',*,*,#5626,.T.);
#7980=ORIENTED_EDGE('',*,*,#6012,.T.);
#7981=ORIENTED_EDGE('',*,*,#5489,.T.);
#7982=ORIENTED_EDGE('',*,*,#6013,.T.);
#7983=ORIENTED_EDGE('',*,*,#5630,.T.);
#7984=ORIENTED_EDGE('',*,*,#6014,.T.);
#7985=ORIENTED_EDGE('',*,*,#5483,.T.);
#7986=ORIENTED_EDGE('',*,*,#6015,.T.);
#7987=ORIENTED_EDGE('',*,*,#5637,.T.);
#7988=ORIENTED_EDGE('',*,*,#6016,.T.);
#7989=ORIENTED_EDGE('',*,*,#5477,.T.);
#7990=ORIENTED_EDGE('',*,*,#6017,.T.);
#7991=ORIENTED_EDGE('',*,*,#5641,.T.);
#7992=ORIENTED_EDGE('',*,*,#6018,.T.);
#7993=ORIENTED_EDGE('',*,*,#5471,.T.);
#7994=ORIENTED_EDGE('',*,*,#6019,.T.);
#7995=ORIENTED_EDGE('',*,*,#5645,.T.);
#7996=ORIENTED_EDGE('',*,*,#6020,.T.);
#7997=ORIENTED_EDGE('',*,*,#5465,.T.);
#7998=ORIENTED_EDGE('',*,*,#6021,.T.);
#7999=ORIENTED_EDGE('',*,*,#5649,.T.);
#8000=ORIENTED_EDGE('',*,*,#6022,.T.);
#8001=ORIENTED_EDGE('',*,*,#5459,.T.);
#8002=ORIENTED_EDGE('',*,*,#6023,.T.);
#8003=ORIENTED_EDGE('',*,*,#5653,.T.);
#8004=ORIENTED_EDGE('',*,*,#6024,.T.);
#8005=ORIENTED_EDGE('',*,*,#5453,.T.);
#8006=ORIENTED_EDGE('',*,*,#6025,.T.);
#8007=ORIENTED_EDGE('',*,*,#5657,.T.);
#8008=ORIENTED_EDGE('',*,*,#6026,.T.);
#8009=ORIENTED_EDGE('',*,*,#5447,.T.);
#8010=ORIENTED_EDGE('',*,*,#6027,.T.);
#8011=ORIENTED_EDGE('',*,*,#5661,.T.);
#8012=ORIENTED_EDGE('',*,*,#6028,.T.);
#8013=ORIENTED_EDGE('',*,*,#5441,.T.);
#8014=ORIENTED_EDGE('',*,*,#6029,.T.);
#8015=ORIENTED_EDGE('',*,*,#5665,.T.);
#8016=ORIENTED_EDGE('',*,*,#6030,.T.);
#8017=ORIENTED_EDGE('',*,*,#5435,.T.);
#8018=ORIENTED_EDGE('',*,*,#6031,.T.);
#8019=ORIENTED_EDGE('',*,*,#5669,.T.);
#8020=ORIENTED_EDGE('',*,*,#6032,.T.);
#8021=ORIENTED_EDGE('',*,*,#5429,.T.);
#8022=ORIENTED_EDGE('',*,*,#6033,.T.);
#8023=ORIENTED_EDGE('',*,*,#5673,.T.);
#8024=ORIENTED_EDGE('',*,*,#6034,.T.);
#8025=ORIENTED_EDGE('',*,*,#5423,.T.);
#8026=ORIENTED_EDGE('',*,*,#6035,.T.);
#8027=ORIENTED_EDGE('',*,*,#5677,.T.);
#8028=ORIENTED_EDGE('',*,*,#6036,.T.);
#8029=ORIENTED_EDGE('',*,*,#5417,.T.);
#8030=ORIENTED_EDGE('',*,*,#6037,.T.);
#8031=ORIENTED_EDGE('',*,*,#5681,.T.);
#8032=ORIENTED_EDGE('',*,*,#6038,.T.);
#8033=ORIENTED_EDGE('',*,*,#5411,.T.);
#8034=ORIENTED_EDGE('',*,*,#6039,.T.);
#8035=ORIENTED_EDGE('',*,*,#5685,.T.);
#8036=ORIENTED_EDGE('',*,*,#6040,.T.);
#8037=ORIENTED_EDGE('',*,*,#5405,.T.);
#8038=ORIENTED_EDGE('',*,*,#6041,.T.);
#8039=ORIENTED_EDGE('',*,*,#5689,.T.);
#8040=ORIENTED_EDGE('',*,*,#6042,.T.);
#8041=ORIENTED_EDGE('',*,*,#5399,.T.);
#8042=ORIENTED_EDGE('',*,*,#6043,.T.);
#8043=ORIENTED_EDGE('',*,*,#5693,.T.);
#8044=ORIENTED_EDGE('',*,*,#6044,.T.);
#8045=ORIENTED_EDGE('',*,*,#5393,.T.);
#8046=ORIENTED_EDGE('',*,*,#6045,.T.);
#8047=ORIENTED_EDGE('',*,*,#5697,.T.);
#8048=ORIENTED_EDGE('',*,*,#6046,.T.);
#8049=ORIENTED_EDGE('',*,*,#5387,.T.);
#8050=ORIENTED_EDGE('',*,*,#6047,.T.);
#8051=ORIENTED_EDGE('',*,*,#5701,.T.);
#8052=ORIENTED_EDGE('',*,*,#6048,.T.);
#8053=ORIENTED_EDGE('',*,*,#5381,.T.);
#8054=ORIENTED_EDGE('',*,*,#6049,.T.);
#8055=ORIENTED_EDGE('',*,*,#5709,.T.);
#8056=ORIENTED_EDGE('',*,*,#6050,.T.);
#8057=ORIENTED_EDGE('',*,*,#5369,.T.);
#8058=ORIENTED_EDGE('',*,*,#6051,.T.);
#8059=ORIENTED_EDGE('',*,*,#5705,.T.);
#8060=ORIENTED_EDGE('',*,*,#6052,.T.);
#8061=ORIENTED_EDGE('',*,*,#5375,.T.);
#8062=ORIENTED_EDGE('',*,*,#6053,.T.);
#8063=ORIENTED_EDGE('',*,*,#5713,.T.);
#8064=ORIENTED_EDGE('',*,*,#6054,.T.);
#8065=ORIENTED_EDGE('',*,*,#5363,.T.);
#8066=ORIENTED_EDGE('',*,*,#6055,.T.);
#8067=ORIENTED_EDGE('',*,*,#5717,.T.);
#8068=ORIENTED_EDGE('',*,*,#6056,.T.);
#8069=ORIENTED_EDGE('',*,*,#5357,.T.);
#8070=ORIENTED_EDGE('',*,*,#6057,.T.);
#8071=ORIENTED_EDGE('',*,*,#5721,.T.);
#8072=ORIENTED_EDGE('',*,*,#6058,.T.);
#8073=ORIENTED_EDGE('',*,*,#5351,.T.);
#8074=ORIENTED_EDGE('',*,*,#6059,.T.);
#8075=ORIENTED_EDGE('',*,*,#5546,.T.);
#8076=ORIENTED_EDGE('',*,*,#6060,.T.);
#8077=ORIENTED_EDGE('',*,*,#5345,.T.);
#8078=ORIENTED_EDGE('',*,*,#6061,.T.);
#8079=ORIENTED_EDGE('',*,*,#5550,.T.);
#8080=ORIENTED_EDGE('',*,*,#6062,.T.);
#8081=ORIENTED_EDGE('',*,*,#5339,.T.);
#8082=ORIENTED_EDGE('',*,*,#6063,.T.);
#8083=ORIENTED_EDGE('',*,*,#5554,.T.);
#8084=ORIENTED_EDGE('',*,*,#6064,.T.);
#8085=ORIENTED_EDGE('',*,*,#5333,.T.);
#8086=ORIENTED_EDGE('',*,*,#6065,.T.);
#8087=ORIENTED_EDGE('',*,*,#5558,.T.);
#8088=ORIENTED_EDGE('',*,*,#6066,.T.);
#8089=ORIENTED_EDGE('',*,*,#5327,.T.);
#8090=ORIENTED_EDGE('',*,*,#6067,.T.);
#8091=ORIENTED_EDGE('',*,*,#5562,.T.);
#8092=ORIENTED_EDGE('',*,*,#6068,.T.);
#8093=ORIENTED_EDGE('',*,*,#5321,.T.);
#8094=ORIENTED_EDGE('',*,*,#6069,.T.);
#8095=ORIENTED_EDGE('',*,*,#5566,.T.);
#8096=ORIENTED_EDGE('',*,*,#6070,.T.);
#8097=ORIENTED_EDGE('',*,*,#5315,.T.);
#8098=ORIENTED_EDGE('',*,*,#6071,.T.);
#8099=ORIENTED_EDGE('',*,*,#5570,.T.);
#8100=ORIENTED_EDGE('',*,*,#6072,.T.);
#8101=ORIENTED_EDGE('',*,*,#5309,.T.);
#8102=ORIENTED_EDGE('',*,*,#6073,.T.);
#8103=ORIENTED_EDGE('',*,*,#5574,.T.);
#8104=ORIENTED_EDGE('',*,*,#6074,.T.);
#8105=ORIENTED_EDGE('',*,*,#5303,.T.);
#8106=ORIENTED_EDGE('',*,*,#6075,.T.);
#8107=ORIENTED_EDGE('',*,*,#5578,.T.);
#8108=ORIENTED_EDGE('',*,*,#6076,.T.);
#8109=ORIENTED_EDGE('',*,*,#5297,.T.);
#8110=ORIENTED_EDGE('',*,*,#6077,.T.);
#8111=ORIENTED_EDGE('',*,*,#5582,.T.);
#8112=ORIENTED_EDGE('',*,*,#6078,.T.);
#8113=ORIENTED_EDGE('',*,*,#5291,.T.);
#8114=ORIENTED_EDGE('',*,*,#6079,.T.);
#8115=ORIENTED_EDGE('',*,*,#5586,.T.);
#8116=ORIENTED_EDGE('',*,*,#6080,.T.);
#8117=ORIENTED_EDGE('',*,*,#5285,.T.);
#8118=ORIENTED_EDGE('',*,*,#6081,.T.);
#8119=ORIENTED_EDGE('',*,*,#5634,.T.);
#8120=ORIENTED_EDGE('',*,*,#5723,.F.);
#8121=ORIENTED_EDGE('',*,*,#6082,.F.);
#8122=ORIENTED_EDGE('',*,*,#6083,.T.);
#8123=ORIENTED_EDGE('',*,*,#6084,.T.);
#8124=ORIENTED_EDGE('',*,*,#5817,.T.);
#8125=ORIENTED_EDGE('',*,*,#6085,.T.);
#8126=ORIENTED_EDGE('',*,*,#5725,.T.);
#8127=ORIENTED_EDGE('',*,*,#6086,.F.);
#8128=ORIENTED_EDGE('',*,*,#6087,.F.);
#8129=ORIENTED_EDGE('',*,*,#6085,.F.);
#8130=ORIENTED_EDGE('',*,*,#6088,.F.);
#8131=ORIENTED_EDGE('',*,*,#6082,.T.);
#8132=ORIENTED_EDGE('',*,*,#5726,.T.);
#8133=ORIENTED_EDGE('',*,*,#6086,.T.);
#8134=ORIENTED_EDGE('',*,*,#5724,.F.);
#8135=ORIENTED_EDGE('',*,*,#6084,.F.);
#8136=ORIENTED_EDGE('',*,*,#6089,.T.);
#8137=ORIENTED_EDGE('',*,*,#6087,.T.);
#8138=ORIENTED_EDGE('',*,*,#6089,.F.);
#8139=ORIENTED_EDGE('',*,*,#6083,.F.);
#8140=ORIENTED_EDGE('',*,*,#6088,.T.);
#8141=ORIENTED_EDGE('',*,*,#5588,.T.);
#8142=ORIENTED_EDGE('',*,*,#6090,.F.);
#8143=ORIENTED_EDGE('',*,*,#6091,.F.);
#8144=ORIENTED_EDGE('',*,*,#6092,.F.);
#8145=ORIENTED_EDGE('',*,*,#6093,.T.);
#8146=ORIENTED_EDGE('',*,*,#5589,.T.);
#8147=ORIENTED_EDGE('',*,*,#6093,.F.);
#8148=ORIENTED_EDGE('',*,*,#6094,.F.);
#8149=ORIENTED_EDGE('',*,*,#5532,.F.);
#8150=ORIENTED_EDGE('',*,*,#5995,.F.);
#8151=ORIENTED_EDGE('',*,*,#5587,.T.);
#8152=ORIENTED_EDGE('',*,*,#6081,.F.);
#8153=ORIENTED_EDGE('',*,*,#5284,.F.);
#8154=ORIENTED_EDGE('',*,*,#6095,.F.);
#8155=ORIENTED_EDGE('',*,*,#6090,.T.);
#8156=ORIENTED_EDGE('',*,*,#6096,.F.);
#8157=ORIENTED_EDGE('',*,*,#6092,.T.);
#8158=ORIENTED_EDGE('',*,*,#6091,.T.);
#8159=ORIENTED_EDGE('',*,*,#6097,.T.);
#8160=ORIENTED_EDGE('',*,*,#5771,.F.);
#8161=ORIENTED_EDGE('',*,*,#5909,.T.);
#8162=ORIENTED_EDGE('',*,*,#5533,.T.);
#8163=ORIENTED_EDGE('',*,*,#6094,.T.);
#8164=ORIENTED_EDGE('',*,*,#6096,.T.);
#8165=ORIENTED_EDGE('',*,*,#5770,.F.);
#8166=ORIENTED_EDGE('',*,*,#6097,.F.);
#8167=ORIENTED_EDGE('',*,*,#6095,.T.);
#8168=ORIENTED_EDGE('',*,*,#5283,.T.);
#8169=ORIENTED_EDGE('',*,*,#5993,.T.);
#8170=ORIENTED_EDGE('',*,*,#5772,.F.);
#8171=ORIENTED_EDGE('',*,*,#6098,.F.);
#8172=ORIENTED_EDGE('',*,*,#6099,.T.);
#8173=ORIENTED_EDGE('',*,*,#5583,.T.);
#8174=ORIENTED_EDGE('',*,*,#6079,.F.);
#8175=ORIENTED_EDGE('',*,*,#5290,.F.);
#8176=ORIENTED_EDGE('',*,*,#6080,.F.);
#8177=ORIENTED_EDGE('',*,*,#5585,.T.);
#8178=ORIENTED_EDGE('',*,*,#6100,.F.);
#8179=ORIENTED_EDGE('',*,*,#6101,.F.);
#8180=ORIENTED_EDGE('',*,*,#5280,.F.);
#8181=ORIENTED_EDGE('',*,*,#5584,.T.);
#8182=ORIENTED_EDGE('',*,*,#6099,.F.);
#8183=ORIENTED_EDGE('',*,*,#6102,.F.);
#8184=ORIENTED_EDGE('',*,*,#6103,.F.);
#8185=ORIENTED_EDGE('',*,*,#6100,.T.);
#8186=ORIENTED_EDGE('',*,*,#6104,.F.);
#8187=ORIENTED_EDGE('',*,*,#6105,.T.);
#8188=ORIENTED_EDGE('',*,*,#5579,.T.);
#8189=ORIENTED_EDGE('',*,*,#6077,.F.);
#8190=ORIENTED_EDGE('',*,*,#5296,.F.);
#8191=ORIENTED_EDGE('',*,*,#6078,.F.);
#8192=ORIENTED_EDGE('',*,*,#5581,.T.);
#8193=ORIENTED_EDGE('',*,*,#6106,.F.);
#8194=ORIENTED_EDGE('',*,*,#6107,.F.);
#8195=ORIENTED_EDGE('',*,*,#5286,.F.);
#8196=ORIENTED_EDGE('',*,*,#5580,.T.);
#8197=ORIENTED_EDGE('',*,*,#6105,.F.);
#8198=ORIENTED_EDGE('',*,*,#6108,.F.);
#8199=ORIENTED_EDGE('',*,*,#6109,.F.);
#8200=ORIENTED_EDGE('',*,*,#6106,.T.);
#8201=ORIENTED_EDGE('',*,*,#6110,.F.);
#8202=ORIENTED_EDGE('',*,*,#6111,.T.);
#8203=ORIENTED_EDGE('',*,*,#5575,.T.);
#8204=ORIENTED_EDGE('',*,*,#6075,.F.);
#8205=ORIENTED_EDGE('',*,*,#5302,.F.);
#8206=ORIENTED_EDGE('',*,*,#6076,.F.);
#8207=ORIENTED_EDGE('',*,*,#5577,.T.);
#8208=ORIENTED_EDGE('',*,*,#6112,.F.);
#8209=ORIENTED_EDGE('',*,*,#6113,.F.);
#8210=ORIENTED_EDGE('',*,*,#5292,.F.);
#8211=ORIENTED_EDGE('',*,*,#5576,.T.);
#8212=ORIENTED_EDGE('',*,*,#6111,.F.);
#8213=ORIENTED_EDGE('',*,*,#6114,.F.);
#8214=ORIENTED_EDGE('',*,*,#6115,.F.);
#8215=ORIENTED_EDGE('',*,*,#6112,.T.);
#8216=ORIENTED_EDGE('',*,*,#6116,.F.);
#8217=ORIENTED_EDGE('',*,*,#6117,.T.);
#8218=ORIENTED_EDGE('',*,*,#5571,.T.);
#8219=ORIENTED_EDGE('',*,*,#6073,.F.);
#8220=ORIENTED_EDGE('',*,*,#5308,.F.);
#8221=ORIENTED_EDGE('',*,*,#6074,.F.);
#8222=ORIENTED_EDGE('',*,*,#5573,.T.);
#8223=ORIENTED_EDGE('',*,*,#6118,.F.);
#8224=ORIENTED_EDGE('',*,*,#6119,.F.);
#8225=ORIENTED_EDGE('',*,*,#5298,.F.);
#8226=ORIENTED_EDGE('',*,*,#5572,.T.);
#8227=ORIENTED_EDGE('',*,*,#6117,.F.);
#8228=ORIENTED_EDGE('',*,*,#6120,.F.);
#8229=ORIENTED_EDGE('',*,*,#6121,.F.);
#8230=ORIENTED_EDGE('',*,*,#6118,.T.);
#8231=ORIENTED_EDGE('',*,*,#6122,.F.);
#8232=ORIENTED_EDGE('',*,*,#6123,.T.);
#8233=ORIENTED_EDGE('',*,*,#5567,.T.);
#8234=ORIENTED_EDGE('',*,*,#6071,.F.);
#8235=ORIENTED_EDGE('',*,*,#5314,.F.);
#8236=ORIENTED_EDGE('',*,*,#6072,.F.);
#8237=ORIENTED_EDGE('',*,*,#5569,.T.);
#8238=ORIENTED_EDGE('',*,*,#6124,.F.);
#8239=ORIENTED_EDGE('',*,*,#6125,.F.);
#8240=ORIENTED_EDGE('',*,*,#5304,.F.);
#8241=ORIENTED_EDGE('',*,*,#5568,.T.);
#8242=ORIENTED_EDGE('',*,*,#6123,.F.);
#8243=ORIENTED_EDGE('',*,*,#6126,.F.);
#8244=ORIENTED_EDGE('',*,*,#6127,.F.);
#8245=ORIENTED_EDGE('',*,*,#6124,.T.);
#8246=ORIENTED_EDGE('',*,*,#6128,.F.);
#8247=ORIENTED_EDGE('',*,*,#6129,.T.);
#8248=ORIENTED_EDGE('',*,*,#5563,.T.);
#8249=ORIENTED_EDGE('',*,*,#6069,.F.);
#8250=ORIENTED_EDGE('',*,*,#5320,.F.);
#8251=ORIENTED_EDGE('',*,*,#6070,.F.);
#8252=ORIENTED_EDGE('',*,*,#5565,.T.);
#8253=ORIENTED_EDGE('',*,*,#6130,.F.);
#8254=ORIENTED_EDGE('',*,*,#6131,.F.);
#8255=ORIENTED_EDGE('',*,*,#5310,.F.);
#8256=ORIENTED_EDGE('',*,*,#5564,.T.);
#8257=ORIENTED_EDGE('',*,*,#6129,.F.);
#8258=ORIENTED_EDGE('',*,*,#6132,.F.);
#8259=ORIENTED_EDGE('',*,*,#6133,.F.);
#8260=ORIENTED_EDGE('',*,*,#6130,.T.);
#8261=ORIENTED_EDGE('',*,*,#6134,.F.);
#8262=ORIENTED_EDGE('',*,*,#6135,.T.);
#8263=ORIENTED_EDGE('',*,*,#5559,.T.);
#8264=ORIENTED_EDGE('',*,*,#6067,.F.);
#8265=ORIENTED_EDGE('',*,*,#5326,.F.);
#8266=ORIENTED_EDGE('',*,*,#6068,.F.);
#8267=ORIENTED_EDGE('',*,*,#5561,.T.);
#8268=ORIENTED_EDGE('',*,*,#6136,.F.);
#8269=ORIENTED_EDGE('',*,*,#6137,.F.);
#8270=ORIENTED_EDGE('',*,*,#5316,.F.);
#8271=ORIENTED_EDGE('',*,*,#5560,.T.);
#8272=ORIENTED_EDGE('',*,*,#6135,.F.);
#8273=ORIENTED_EDGE('',*,*,#6138,.F.);
#8274=ORIENTED_EDGE('',*,*,#6139,.F.);
#8275=ORIENTED_EDGE('',*,*,#6136,.T.);
#8276=ORIENTED_EDGE('',*,*,#6140,.F.);
#8277=ORIENTED_EDGE('',*,*,#6141,.T.);
#8278=ORIENTED_EDGE('',*,*,#5555,.T.);
#8279=ORIENTED_EDGE('',*,*,#6065,.F.);
#8280=ORIENTED_EDGE('',*,*,#5332,.F.);
#8281=ORIENTED_EDGE('',*,*,#6066,.F.);
#8282=ORIENTED_EDGE('',*,*,#5557,.T.);
#8283=ORIENTED_EDGE('',*,*,#6142,.F.);
#8284=ORIENTED_EDGE('',*,*,#6143,.F.);
#8285=ORIENTED_EDGE('',*,*,#5322,.F.);
#8286=ORIENTED_EDGE('',*,*,#5556,.T.);
#8287=ORIENTED_EDGE('',*,*,#6141,.F.);
#8288=ORIENTED_EDGE('',*,*,#6144,.F.);
#8289=ORIENTED_EDGE('',*,*,#6145,.F.);
#8290=ORIENTED_EDGE('',*,*,#6142,.T.);
#8291=ORIENTED_EDGE('',*,*,#6146,.F.);
#8292=ORIENTED_EDGE('',*,*,#6147,.T.);
#8293=ORIENTED_EDGE('',*,*,#5551,.T.);
#8294=ORIENTED_EDGE('',*,*,#6063,.F.);
#8295=ORIENTED_EDGE('',*,*,#5338,.F.);
#8296=ORIENTED_EDGE('',*,*,#6064,.F.);
#8297=ORIENTED_EDGE('',*,*,#5553,.T.);
#8298=ORIENTED_EDGE('',*,*,#6148,.F.);
#8299=ORIENTED_EDGE('',*,*,#6149,.F.);
#8300=ORIENTED_EDGE('',*,*,#5328,.F.);
#8301=ORIENTED_EDGE('',*,*,#5552,.T.);
#8302=ORIENTED_EDGE('',*,*,#6147,.F.);
#8303=ORIENTED_EDGE('',*,*,#6150,.F.);
#8304=ORIENTED_EDGE('',*,*,#6151,.F.);
#8305=ORIENTED_EDGE('',*,*,#6148,.T.);
#8306=ORIENTED_EDGE('',*,*,#6152,.F.);
#8307=ORIENTED_EDGE('',*,*,#6153,.T.);
#8308=ORIENTED_EDGE('',*,*,#5547,.T.);
#8309=ORIENTED_EDGE('',*,*,#6061,.F.);
#8310=ORIENTED_EDGE('',*,*,#5344,.F.);
#8311=ORIENTED_EDGE('',*,*,#6062,.F.);
#8312=ORIENTED_EDGE('',*,*,#5549,.T.);
#8313=ORIENTED_EDGE('',*,*,#6154,.F.);
#8314=ORIENTED_EDGE('',*,*,#6155,.F.);
#8315=ORIENTED_EDGE('',*,*,#5334,.F.);
#8316=ORIENTED_EDGE('',*,*,#5548,.T.);
#8317=ORIENTED_EDGE('',*,*,#6153,.F.);
#8318=ORIENTED_EDGE('',*,*,#6156,.F.);
#8319=ORIENTED_EDGE('',*,*,#6157,.F.);
#8320=ORIENTED_EDGE('',*,*,#6154,.T.);
#8321=ORIENTED_EDGE('',*,*,#6158,.F.);
#8322=ORIENTED_EDGE('',*,*,#6159,.T.);
#8323=ORIENTED_EDGE('',*,*,#5722,.T.);
#8324=ORIENTED_EDGE('',*,*,#6059,.F.);
#8325=ORIENTED_EDGE('',*,*,#5350,.F.);
#8326=ORIENTED_EDGE('',*,*,#6060,.F.);
#8327=ORIENTED_EDGE('',*,*,#5545,.T.);
#8328=ORIENTED_EDGE('',*,*,#6160,.F.);
#8329=ORIENTED_EDGE('',*,*,#6161,.F.);
#8330=ORIENTED_EDGE('',*,*,#5340,.F.);
#8331=ORIENTED_EDGE('',*,*,#5544,.T.);
#8332=ORIENTED_EDGE('',*,*,#6159,.F.);
#8333=ORIENTED_EDGE('',*,*,#6162,.F.);
#8334=ORIENTED_EDGE('',*,*,#6163,.F.);
#8335=ORIENTED_EDGE('',*,*,#6160,.T.);
#8336=ORIENTED_EDGE('',*,*,#6164,.F.);
#8337=ORIENTED_EDGE('',*,*,#6165,.T.);
#8338=ORIENTED_EDGE('',*,*,#5718,.T.);
#8339=ORIENTED_EDGE('',*,*,#6057,.F.);
#8340=ORIENTED_EDGE('',*,*,#5356,.F.);
#8341=ORIENTED_EDGE('',*,*,#6058,.F.);
#8342=ORIENTED_EDGE('',*,*,#5720,.T.);
#8343=ORIENTED_EDGE('',*,*,#6166,.F.);
#8344=ORIENTED_EDGE('',*,*,#6167,.F.);
#8345=ORIENTED_EDGE('',*,*,#5346,.F.);
#8346=ORIENTED_EDGE('',*,*,#5719,.T.);
#8347=ORIENTED_EDGE('',*,*,#6165,.F.);
#8348=ORIENTED_EDGE('',*,*,#6168,.F.);
#8349=ORIENTED_EDGE('',*,*,#6169,.F.);
#8350=ORIENTED_EDGE('',*,*,#6166,.T.);
#8351=ORIENTED_EDGE('',*,*,#6170,.F.);
#8352=ORIENTED_EDGE('',*,*,#6171,.T.);
#8353=ORIENTED_EDGE('',*,*,#5714,.T.);
#8354=ORIENTED_EDGE('',*,*,#6055,.F.);
#8355=ORIENTED_EDGE('',*,*,#5362,.F.);
#8356=ORIENTED_EDGE('',*,*,#6056,.F.);
#8357=ORIENTED_EDGE('',*,*,#5716,.T.);
#8358=ORIENTED_EDGE('',*,*,#6172,.F.);
#8359=ORIENTED_EDGE('',*,*,#6173,.F.);
#8360=ORIENTED_EDGE('',*,*,#5352,.F.);
#8361=ORIENTED_EDGE('',*,*,#5715,.T.);
#8362=ORIENTED_EDGE('',*,*,#6171,.F.);
#8363=ORIENTED_EDGE('',*,*,#6174,.F.);
#8364=ORIENTED_EDGE('',*,*,#6175,.F.);
#8365=ORIENTED_EDGE('',*,*,#6172,.T.);
#8366=ORIENTED_EDGE('',*,*,#6176,.F.);
#8367=ORIENTED_EDGE('',*,*,#6177,.T.);
#8368=ORIENTED_EDGE('',*,*,#5710,.T.);
#8369=ORIENTED_EDGE('',*,*,#6051,.F.);
#8370=ORIENTED_EDGE('',*,*,#5368,.F.);
#8371=ORIENTED_EDGE('',*,*,#6054,.F.);
#8372=ORIENTED_EDGE('',*,*,#5712,.T.);
#8373=ORIENTED_EDGE('',*,*,#6178,.F.);
#8374=ORIENTED_EDGE('',*,*,#6179,.F.);
#8375=ORIENTED_EDGE('',*,*,#5358,.F.);
#8376=ORIENTED_EDGE('',*,*,#5711,.T.);
#8377=ORIENTED_EDGE('',*,*,#6177,.F.);
#8378=ORIENTED_EDGE('',*,*,#6180,.F.);
#8379=ORIENTED_EDGE('',*,*,#6181,.F.);
#8380=ORIENTED_EDGE('',*,*,#6178,.T.);
#8381=ORIENTED_EDGE('',*,*,#6050,.F.);
#8382=ORIENTED_EDGE('',*,*,#5708,.T.);
#8383=ORIENTED_EDGE('',*,*,#6182,.F.);
#8384=ORIENTED_EDGE('',*,*,#6183,.F.);
#8385=ORIENTED_EDGE('',*,*,#5364,.F.);
#8386=ORIENTED_EDGE('',*,*,#6184,.F.);
#8387=ORIENTED_EDGE('',*,*,#6185,.T.);
#8388=ORIENTED_EDGE('',*,*,#5706,.T.);
#8389=ORIENTED_EDGE('',*,*,#6053,.F.);
#8390=ORIENTED_EDGE('',*,*,#5374,.F.);
#8391=ORIENTED_EDGE('',*,*,#5707,.T.);
#8392=ORIENTED_EDGE('',*,*,#6185,.F.);
#8393=ORIENTED_EDGE('',*,*,#6186,.F.);
#8394=ORIENTED_EDGE('',*,*,#6187,.F.);
#8395=ORIENTED_EDGE('',*,*,#6182,.T.);
#8396=ORIENTED_EDGE('',*,*,#6188,.F.);
#8397=ORIENTED_EDGE('',*,*,#6189,.T.);
#8398=ORIENTED_EDGE('',*,*,#5702,.T.);
#8399=ORIENTED_EDGE('',*,*,#6049,.F.);
#8400=ORIENTED_EDGE('',*,*,#5380,.F.);
#8401=ORIENTED_EDGE('',*,*,#6052,.F.);
#8402=ORIENTED_EDGE('',*,*,#5704,.T.);
#8403=ORIENTED_EDGE('',*,*,#6190,.F.);
#8404=ORIENTED_EDGE('',*,*,#6191,.F.);
#8405=ORIENTED_EDGE('',*,*,#5370,.F.);
#8406=ORIENTED_EDGE('',*,*,#5703,.T.);
#8407=ORIENTED_EDGE('',*,*,#6189,.F.);
#8408=ORIENTED_EDGE('',*,*,#6192,.F.);
#8409=ORIENTED_EDGE('',*,*,#6193,.F.);
#8410=ORIENTED_EDGE('',*,*,#6190,.T.);
#8411=ORIENTED_EDGE('',*,*,#6194,.F.);
#8412=ORIENTED_EDGE('',*,*,#6195,.T.);
#8413=ORIENTED_EDGE('',*,*,#5698,.T.);
#8414=ORIENTED_EDGE('',*,*,#6047,.F.);
#8415=ORIENTED_EDGE('',*,*,#5386,.F.);
#8416=ORIENTED_EDGE('',*,*,#6048,.F.);
#8417=ORIENTED_EDGE('',*,*,#5700,.T.);
#8418=ORIENTED_EDGE('',*,*,#6196,.F.);
#8419=ORIENTED_EDGE('',*,*,#6197,.F.);
#8420=ORIENTED_EDGE('',*,*,#5376,.F.);
#8421=ORIENTED_EDGE('',*,*,#5699,.T.);
#8422=ORIENTED_EDGE('',*,*,#6195,.F.);
#8423=ORIENTED_EDGE('',*,*,#6198,.F.);
#8424=ORIENTED_EDGE('',*,*,#6199,.F.);
#8425=ORIENTED_EDGE('',*,*,#6196,.T.);
#8426=ORIENTED_EDGE('',*,*,#6200,.F.);
#8427=ORIENTED_EDGE('',*,*,#6201,.T.);
#8428=ORIENTED_EDGE('',*,*,#5694,.T.);
#8429=ORIENTED_EDGE('',*,*,#6045,.F.);
#8430=ORIENTED_EDGE('',*,*,#5392,.F.);
#8431=ORIENTED_EDGE('',*,*,#6046,.F.);
#8432=ORIENTED_EDGE('',*,*,#5696,.T.);
#8433=ORIENTED_EDGE('',*,*,#6202,.F.);
#8434=ORIENTED_EDGE('',*,*,#6203,.F.);
#8435=ORIENTED_EDGE('',*,*,#5382,.F.);
#8436=ORIENTED_EDGE('',*,*,#5695,.T.);
#8437=ORIENTED_EDGE('',*,*,#6201,.F.);
#8438=ORIENTED_EDGE('',*,*,#6204,.F.);
#8439=ORIENTED_EDGE('',*,*,#6205,.F.);
#8440=ORIENTED_EDGE('',*,*,#6202,.T.);
#8441=ORIENTED_EDGE('',*,*,#6206,.F.);
#8442=ORIENTED_EDGE('',*,*,#6207,.T.);
#8443=ORIENTED_EDGE('',*,*,#5690,.T.);
#8444=ORIENTED_EDGE('',*,*,#6043,.F.);
#8445=ORIENTED_EDGE('',*,*,#5398,.F.);
#8446=ORIENTED_EDGE('',*,*,#6044,.F.);
#8447=ORIENTED_EDGE('',*,*,#5692,.T.);
#8448=ORIENTED_EDGE('',*,*,#6208,.F.);
#8449=ORIENTED_EDGE('',*,*,#6209,.F.);
#8450=ORIENTED_EDGE('',*,*,#5388,.F.);
#8451=ORIENTED_EDGE('',*,*,#5691,.T.);
#8452=ORIENTED_EDGE('',*,*,#6207,.F.);
#8453=ORIENTED_EDGE('',*,*,#6210,.F.);
#8454=ORIENTED_EDGE('',*,*,#6211,.F.);
#8455=ORIENTED_EDGE('',*,*,#6208,.T.);
#8456=ORIENTED_EDGE('',*,*,#6212,.F.);
#8457=ORIENTED_EDGE('',*,*,#6213,.T.);
#8458=ORIENTED_EDGE('',*,*,#5686,.T.);
#8459=ORIENTED_EDGE('',*,*,#6041,.F.);
#8460=ORIENTED_EDGE('',*,*,#5404,.F.);
#8461=ORIENTED_EDGE('',*,*,#6042,.F.);
#8462=ORIENTED_EDGE('',*,*,#5688,.T.);
#8463=ORIENTED_EDGE('',*,*,#6214,.F.);
#8464=ORIENTED_EDGE('',*,*,#6215,.F.);
#8465=ORIENTED_EDGE('',*,*,#5394,.F.);
#8466=ORIENTED_EDGE('',*,*,#5687,.T.);
#8467=ORIENTED_EDGE('',*,*,#6213,.F.);
#8468=ORIENTED_EDGE('',*,*,#6216,.F.);
#8469=ORIENTED_EDGE('',*,*,#6217,.F.);
#8470=ORIENTED_EDGE('',*,*,#6214,.T.);
#8471=ORIENTED_EDGE('',*,*,#6218,.F.);
#8472=ORIENTED_EDGE('',*,*,#6219,.T.);
#8473=ORIENTED_EDGE('',*,*,#5682,.T.);
#8474=ORIENTED_EDGE('',*,*,#6039,.F.);
#8475=ORIENTED_EDGE('',*,*,#5410,.F.);
#8476=ORIENTED_EDGE('',*,*,#6040,.F.);
#8477=ORIENTED_EDGE('',*,*,#5684,.T.);
#8478=ORIENTED_EDGE('',*,*,#6220,.F.);
#8479=ORIENTED_EDGE('',*,*,#6221,.F.);
#8480=ORIENTED_EDGE('',*,*,#5400,.F.);
#8481=ORIENTED_EDGE('',*,*,#5683,.T.);
#8482=ORIENTED_EDGE('',*,*,#6219,.F.);
#8483=ORIENTED_EDGE('',*,*,#6222,.F.);
#8484=ORIENTED_EDGE('',*,*,#6223,.F.);
#8485=ORIENTED_EDGE('',*,*,#6220,.T.);
#8486=ORIENTED_EDGE('',*,*,#6224,.F.);
#8487=ORIENTED_EDGE('',*,*,#6225,.T.);
#8488=ORIENTED_EDGE('',*,*,#5678,.T.);
#8489=ORIENTED_EDGE('',*,*,#6037,.F.);
#8490=ORIENTED_EDGE('',*,*,#5416,.F.);
#8491=ORIENTED_EDGE('',*,*,#6038,.F.);
#8492=ORIENTED_EDGE('',*,*,#5680,.T.);
#8493=ORIENTED_EDGE('',*,*,#6226,.F.);
#8494=ORIENTED_EDGE('',*,*,#6227,.F.);
#8495=ORIENTED_EDGE('',*,*,#5406,.F.);
#8496=ORIENTED_EDGE('',*,*,#5679,.T.);
#8497=ORIENTED_EDGE('',*,*,#6225,.F.);
#8498=ORIENTED_EDGE('',*,*,#6228,.F.);
#8499=ORIENTED_EDGE('',*,*,#6229,.F.);
#8500=ORIENTED_EDGE('',*,*,#6226,.T.);
#8501=ORIENTED_EDGE('',*,*,#6230,.F.);
#8502=ORIENTED_EDGE('',*,*,#6231,.T.);
#8503=ORIENTED_EDGE('',*,*,#5674,.T.);
#8504=ORIENTED_EDGE('',*,*,#6035,.F.);
#8505=ORIENTED_EDGE('',*,*,#5422,.F.);
#8506=ORIENTED_EDGE('',*,*,#6036,.F.);
#8507=ORIENTED_EDGE('',*,*,#5676,.T.);
#8508=ORIENTED_EDGE('',*,*,#6232,.F.);
#8509=ORIENTED_EDGE('',*,*,#6233,.F.);
#8510=ORIENTED_EDGE('',*,*,#5412,.F.);
#8511=ORIENTED_EDGE('',*,*,#5675,.T.);
#8512=ORIENTED_EDGE('',*,*,#6231,.F.);
#8513=ORIENTED_EDGE('',*,*,#6234,.F.);
#8514=ORIENTED_EDGE('',*,*,#6235,.F.);
#8515=ORIENTED_EDGE('',*,*,#6232,.T.);
#8516=ORIENTED_EDGE('',*,*,#6236,.F.);
#8517=ORIENTED_EDGE('',*,*,#6237,.T.);
#8518=ORIENTED_EDGE('',*,*,#5670,.T.);
#8519=ORIENTED_EDGE('',*,*,#6033,.F.);
#8520=ORIENTED_EDGE('',*,*,#5428,.F.);
#8521=ORIENTED_EDGE('',*,*,#6034,.F.);
#8522=ORIENTED_EDGE('',*,*,#5672,.T.);
#8523=ORIENTED_EDGE('',*,*,#6238,.F.);
#8524=ORIENTED_EDGE('',*,*,#6239,.F.);
#8525=ORIENTED_EDGE('',*,*,#5418,.F.);
#8526=ORIENTED_EDGE('',*,*,#5671,.T.);
#8527=ORIENTED_EDGE('',*,*,#6237,.F.);
#8528=ORIENTED_EDGE('',*,*,#6240,.F.);
#8529=ORIENTED_EDGE('',*,*,#6241,.F.);
#8530=ORIENTED_EDGE('',*,*,#6238,.T.);
#8531=ORIENTED_EDGE('',*,*,#6242,.F.);
#8532=ORIENTED_EDGE('',*,*,#6243,.T.);
#8533=ORIENTED_EDGE('',*,*,#5666,.T.);
#8534=ORIENTED_EDGE('',*,*,#6031,.F.);
#8535=ORIENTED_EDGE('',*,*,#5434,.F.);
#8536=ORIENTED_EDGE('',*,*,#6032,.F.);
#8537=ORIENTED_EDGE('',*,*,#5668,.T.);
#8538=ORIENTED_EDGE('',*,*,#6244,.F.);
#8539=ORIENTED_EDGE('',*,*,#6245,.F.);
#8540=ORIENTED_EDGE('',*,*,#5424,.F.);
#8541=ORIENTED_EDGE('',*,*,#5667,.T.);
#8542=ORIENTED_EDGE('',*,*,#6243,.F.);
#8543=ORIENTED_EDGE('',*,*,#6246,.F.);
#8544=ORIENTED_EDGE('',*,*,#6247,.F.);
#8545=ORIENTED_EDGE('',*,*,#6244,.T.);
#8546=ORIENTED_EDGE('',*,*,#6248,.F.);
#8547=ORIENTED_EDGE('',*,*,#6249,.T.);
#8548=ORIENTED_EDGE('',*,*,#5662,.T.);
#8549=ORIENTED_EDGE('',*,*,#6029,.F.);
#8550=ORIENTED_EDGE('',*,*,#5440,.F.);
#8551=ORIENTED_EDGE('',*,*,#6030,.F.);
#8552=ORIENTED_EDGE('',*,*,#5664,.T.);
#8553=ORIENTED_EDGE('',*,*,#6250,.F.);
#8554=ORIENTED_EDGE('',*,*,#6251,.F.);
#8555=ORIENTED_EDGE('',*,*,#5430,.F.);
#8556=ORIENTED_EDGE('',*,*,#5663,.T.);
#8557=ORIENTED_EDGE('',*,*,#6249,.F.);
#8558=ORIENTED_EDGE('',*,*,#6252,.F.);
#8559=ORIENTED_EDGE('',*,*,#6253,.F.);
#8560=ORIENTED_EDGE('',*,*,#6250,.T.);
#8561=ORIENTED_EDGE('',*,*,#6254,.F.);
#8562=ORIENTED_EDGE('',*,*,#6255,.T.);
#8563=ORIENTED_EDGE('',*,*,#5658,.T.);
#8564=ORIENTED_EDGE('',*,*,#6027,.F.);
#8565=ORIENTED_EDGE('',*,*,#5446,.F.);
#8566=ORIENTED_EDGE('',*,*,#6028,.F.);
#8567=ORIENTED_EDGE('',*,*,#5660,.T.);
#8568=ORIENTED_EDGE('',*,*,#6256,.F.);
#8569=ORIENTED_EDGE('',*,*,#6257,.F.);
#8570=ORIENTED_EDGE('',*,*,#5436,.F.);
#8571=ORIENTED_EDGE('',*,*,#5659,.T.);
#8572=ORIENTED_EDGE('',*,*,#6255,.F.);
#8573=ORIENTED_EDGE('',*,*,#6258,.F.);
#8574=ORIENTED_EDGE('',*,*,#6259,.F.);
#8575=ORIENTED_EDGE('',*,*,#6256,.T.);
#8576=ORIENTED_EDGE('',*,*,#6260,.F.);
#8577=ORIENTED_EDGE('',*,*,#6261,.T.);
#8578=ORIENTED_EDGE('',*,*,#5654,.T.);
#8579=ORIENTED_EDGE('',*,*,#6025,.F.);
#8580=ORIENTED_EDGE('',*,*,#5452,.F.);
#8581=ORIENTED_EDGE('',*,*,#6026,.F.);
#8582=ORIENTED_EDGE('',*,*,#5656,.T.);
#8583=ORIENTED_EDGE('',*,*,#6262,.F.);
#8584=ORIENTED_EDGE('',*,*,#6263,.F.);
#8585=ORIENTED_EDGE('',*,*,#5442,.F.);
#8586=ORIENTED_EDGE('',*,*,#5655,.T.);
#8587=ORIENTED_EDGE('',*,*,#6261,.F.);
#8588=ORIENTED_EDGE('',*,*,#6264,.F.);
#8589=ORIENTED_EDGE('',*,*,#6265,.F.);
#8590=ORIENTED_EDGE('',*,*,#6262,.T.);
#8591=ORIENTED_EDGE('',*,*,#6266,.F.);
#8592=ORIENTED_EDGE('',*,*,#6267,.T.);
#8593=ORIENTED_EDGE('',*,*,#5650,.T.);
#8594=ORIENTED_EDGE('',*,*,#6023,.F.);
#8595=ORIENTED_EDGE('',*,*,#5458,.F.);
#8596=ORIENTED_EDGE('',*,*,#6024,.F.);
#8597=ORIENTED_EDGE('',*,*,#5652,.T.);
#8598=ORIENTED_EDGE('',*,*,#6268,.F.);
#8599=ORIENTED_EDGE('',*,*,#6269,.F.);
#8600=ORIENTED_EDGE('',*,*,#5448,.F.);
#8601=ORIENTED_EDGE('',*,*,#5651,.T.);
#8602=ORIENTED_EDGE('',*,*,#6267,.F.);
#8603=ORIENTED_EDGE('',*,*,#6270,.F.);
#8604=ORIENTED_EDGE('',*,*,#6271,.F.);
#8605=ORIENTED_EDGE('',*,*,#6268,.T.);
#8606=ORIENTED_EDGE('',*,*,#6272,.F.);
#8607=ORIENTED_EDGE('',*,*,#6273,.T.);
#8608=ORIENTED_EDGE('',*,*,#5646,.T.);
#8609=ORIENTED_EDGE('',*,*,#6021,.F.);
#8610=ORIENTED_EDGE('',*,*,#5464,.F.);
#8611=ORIENTED_EDGE('',*,*,#6022,.F.);
#8612=ORIENTED_EDGE('',*,*,#5648,.T.);
#8613=ORIENTED_EDGE('',*,*,#6274,.F.);
#8614=ORIENTED_EDGE('',*,*,#6275,.F.);
#8615=ORIENTED_EDGE('',*,*,#5454,.F.);
#8616=ORIENTED_EDGE('',*,*,#5647,.T.);
#8617=ORIENTED_EDGE('',*,*,#6273,.F.);
#8618=ORIENTED_EDGE('',*,*,#6276,.F.);
#8619=ORIENTED_EDGE('',*,*,#6277,.F.);
#8620=ORIENTED_EDGE('',*,*,#6274,.T.);
#8621=ORIENTED_EDGE('',*,*,#6278,.F.);
#8622=ORIENTED_EDGE('',*,*,#6279,.T.);
#8623=ORIENTED_EDGE('',*,*,#5642,.T.);
#8624=ORIENTED_EDGE('',*,*,#6019,.F.);
#8625=ORIENTED_EDGE('',*,*,#5470,.F.);
#8626=ORIENTED_EDGE('',*,*,#6020,.F.);
#8627=ORIENTED_EDGE('',*,*,#5644,.T.);
#8628=ORIENTED_EDGE('',*,*,#6280,.F.);
#8629=ORIENTED_EDGE('',*,*,#6281,.F.);
#8630=ORIENTED_EDGE('',*,*,#5460,.F.);
#8631=ORIENTED_EDGE('',*,*,#5643,.T.);
#8632=ORIENTED_EDGE('',*,*,#6279,.F.);
#8633=ORIENTED_EDGE('',*,*,#6282,.F.);
#8634=ORIENTED_EDGE('',*,*,#6283,.F.);
#8635=ORIENTED_EDGE('',*,*,#6280,.T.);
#8636=ORIENTED_EDGE('',*,*,#6284,.F.);
#8637=ORIENTED_EDGE('',*,*,#6285,.T.);
#8638=ORIENTED_EDGE('',*,*,#5638,.T.);
#8639=ORIENTED_EDGE('',*,*,#6017,.F.);
#8640=ORIENTED_EDGE('',*,*,#5476,.F.);
#8641=ORIENTED_EDGE('',*,*,#6018,.F.);
#8642=ORIENTED_EDGE('',*,*,#5640,.T.);
#8643=ORIENTED_EDGE('',*,*,#6286,.F.);
#8644=ORIENTED_EDGE('',*,*,#6287,.F.);
#8645=ORIENTED_EDGE('',*,*,#5466,.F.);
#8646=ORIENTED_EDGE('',*,*,#5639,.T.);
#8647=ORIENTED_EDGE('',*,*,#6285,.F.);
#8648=ORIENTED_EDGE('',*,*,#6288,.F.);
#8649=ORIENTED_EDGE('',*,*,#6289,.F.);
#8650=ORIENTED_EDGE('',*,*,#6286,.T.);
#8651=ORIENTED_EDGE('',*,*,#6290,.F.);
#8652=ORIENTED_EDGE('',*,*,#6291,.T.);
#8653=ORIENTED_EDGE('',*,*,#5631,.T.);
#8654=ORIENTED_EDGE('',*,*,#6015,.F.);
#8655=ORIENTED_EDGE('',*,*,#5482,.F.);
#8656=ORIENTED_EDGE('',*,*,#6016,.F.);
#8657=ORIENTED_EDGE('',*,*,#5636,.T.);
#8658=ORIENTED_EDGE('',*,*,#6292,.F.);
#8659=ORIENTED_EDGE('',*,*,#6293,.F.);
#8660=ORIENTED_EDGE('',*,*,#5472,.F.);
#8661=ORIENTED_EDGE('',*,*,#5635,.T.);
#8662=ORIENTED_EDGE('',*,*,#5632,.T.);
#8663=ORIENTED_EDGE('',*,*,#6291,.F.);
#8664=ORIENTED_EDGE('',*,*,#6294,.F.);
#8665=ORIENTED_EDGE('',*,*,#6295,.F.);
#8666=ORIENTED_EDGE('',*,*,#6292,.T.);
#8667=ORIENTED_EDGE('',*,*,#6296,.F.);
#8668=ORIENTED_EDGE('',*,*,#6297,.T.);
#8669=ORIENTED_EDGE('',*,*,#5627,.T.);
#8670=ORIENTED_EDGE('',*,*,#6013,.F.);
#8671=ORIENTED_EDGE('',*,*,#5488,.F.);
#8672=ORIENTED_EDGE('',*,*,#6014,.F.);
#8673=ORIENTED_EDGE('',*,*,#5629,.T.);
#8674=ORIENTED_EDGE('',*,*,#6298,.F.);
#8675=ORIENTED_EDGE('',*,*,#6299,.F.);
#8676=ORIENTED_EDGE('',*,*,#5478,.F.);
#8677=ORIENTED_EDGE('',*,*,#5628,.T.);
#8678=ORIENTED_EDGE('',*,*,#6297,.F.);
#8679=ORIENTED_EDGE('',*,*,#6300,.F.);
#8680=ORIENTED_EDGE('',*,*,#6301,.F.);
#8681=ORIENTED_EDGE('',*,*,#6298,.T.);
#8682=ORIENTED_EDGE('',*,*,#6302,.F.);
#8683=ORIENTED_EDGE('',*,*,#6303,.T.);
#8684=ORIENTED_EDGE('',*,*,#5623,.T.);
#8685=ORIENTED_EDGE('',*,*,#6011,.F.);
#8686=ORIENTED_EDGE('',*,*,#5494,.F.);
#8687=ORIENTED_EDGE('',*,*,#6012,.F.);
#8688=ORIENTED_EDGE('',*,*,#5625,.T.);
#8689=ORIENTED_EDGE('',*,*,#6304,.F.);
#8690=ORIENTED_EDGE('',*,*,#6305,.F.);
#8691=ORIENTED_EDGE('',*,*,#5484,.F.);
#8692=ORIENTED_EDGE('',*,*,#5624,.T.);
#8693=ORIENTED_EDGE('',*,*,#6303,.F.);
#8694=ORIENTED_EDGE('',*,*,#6306,.F.);
#8695=ORIENTED_EDGE('',*,*,#6307,.F.);
#8696=ORIENTED_EDGE('',*,*,#6304,.T.);
#8697=ORIENTED_EDGE('',*,*,#6308,.F.);
#8698=ORIENTED_EDGE('',*,*,#6309,.T.);
#8699=ORIENTED_EDGE('',*,*,#5619,.T.);
#8700=ORIENTED_EDGE('',*,*,#6007,.F.);
#8701=ORIENTED_EDGE('',*,*,#5500,.F.);
#8702=ORIENTED_EDGE('',*,*,#6010,.F.);
#8703=ORIENTED_EDGE('',*,*,#5621,.T.);
#8704=ORIENTED_EDGE('',*,*,#6310,.F.);
#8705=ORIENTED_EDGE('',*,*,#6311,.F.);
#8706=ORIENTED_EDGE('',*,*,#5490,.F.);
#8707=ORIENTED_EDGE('',*,*,#5620,.T.);
#8708=ORIENTED_EDGE('',*,*,#6309,.F.);
#8709=ORIENTED_EDGE('',*,*,#6312,.F.);
#8710=ORIENTED_EDGE('',*,*,#6313,.F.);
#8711=ORIENTED_EDGE('',*,*,#6310,.T.);
#8712=ORIENTED_EDGE('',*,*,#6006,.F.);
#8713=ORIENTED_EDGE('',*,*,#5617,.T.);
#8714=ORIENTED_EDGE('',*,*,#6314,.F.);
#8715=ORIENTED_EDGE('',*,*,#6315,.F.);
#8716=ORIENTED_EDGE('',*,*,#5496,.F.);
#8717=ORIENTED_EDGE('',*,*,#6316,.F.);
#8718=ORIENTED_EDGE('',*,*,#6317,.T.);
#8719=ORIENTED_EDGE('',*,*,#5615,.T.);
#8720=ORIENTED_EDGE('',*,*,#6009,.F.);
#8721=ORIENTED_EDGE('',*,*,#5506,.F.);
#8722=ORIENTED_EDGE('',*,*,#5616,.T.);
#8723=ORIENTED_EDGE('',*,*,#6317,.F.);
#8724=ORIENTED_EDGE('',*,*,#6318,.F.);
#8725=ORIENTED_EDGE('',*,*,#6319,.F.);
#8726=ORIENTED_EDGE('',*,*,#6314,.T.);
#8727=ORIENTED_EDGE('',*,*,#6320,.F.);
#8728=ORIENTED_EDGE('',*,*,#6321,.T.);
#8729=ORIENTED_EDGE('',*,*,#5611,.T.);
#8730=ORIENTED_EDGE('',*,*,#6005,.F.);
#8731=ORIENTED_EDGE('',*,*,#5512,.F.);
#8732=ORIENTED_EDGE('',*,*,#6008,.F.);
#8733=ORIENTED_EDGE('',*,*,#5613,.T.);
#8734=ORIENTED_EDGE('',*,*,#6322,.F.);
#8735=ORIENTED_EDGE('',*,*,#6323,.F.);
#8736=ORIENTED_EDGE('',*,*,#5502,.F.);
#8737=ORIENTED_EDGE('',*,*,#5612,.T.);
#8738=ORIENTED_EDGE('',*,*,#6321,.F.);
#8739=ORIENTED_EDGE('',*,*,#6324,.F.);
#8740=ORIENTED_EDGE('',*,*,#6325,.F.);
#8741=ORIENTED_EDGE('',*,*,#6322,.T.);
#8742=ORIENTED_EDGE('',*,*,#6326,.F.);
#8743=ORIENTED_EDGE('',*,*,#6327,.T.);
#8744=ORIENTED_EDGE('',*,*,#5607,.T.);
#8745=ORIENTED_EDGE('',*,*,#6003,.F.);
#8746=ORIENTED_EDGE('',*,*,#5518,.F.);
#8747=ORIENTED_EDGE('',*,*,#6004,.F.);
#8748=ORIENTED_EDGE('',*,*,#5609,.T.);
#8749=ORIENTED_EDGE('',*,*,#6328,.F.);
#8750=ORIENTED_EDGE('',*,*,#6329,.F.);
#8751=ORIENTED_EDGE('',*,*,#5508,.F.);
#8752=ORIENTED_EDGE('',*,*,#5608,.T.);
#8753=ORIENTED_EDGE('',*,*,#6327,.F.);
#8754=ORIENTED_EDGE('',*,*,#6330,.F.);
#8755=ORIENTED_EDGE('',*,*,#6331,.F.);
#8756=ORIENTED_EDGE('',*,*,#6328,.T.);
#8757=ORIENTED_EDGE('',*,*,#6332,.F.);
#8758=ORIENTED_EDGE('',*,*,#6333,.T.);
#8759=ORIENTED_EDGE('',*,*,#5603,.T.);
#8760=ORIENTED_EDGE('',*,*,#6001,.F.);
#8761=ORIENTED_EDGE('',*,*,#5524,.F.);
#8762=ORIENTED_EDGE('',*,*,#6002,.F.);
#8763=ORIENTED_EDGE('',*,*,#5605,.T.);
#8764=ORIENTED_EDGE('',*,*,#6334,.F.);
#8765=ORIENTED_EDGE('',*,*,#6335,.F.);
#8766=ORIENTED_EDGE('',*,*,#5514,.F.);
#8767=ORIENTED_EDGE('',*,*,#5604,.T.);
#8768=ORIENTED_EDGE('',*,*,#6333,.F.);
#8769=ORIENTED_EDGE('',*,*,#6336,.F.);
#8770=ORIENTED_EDGE('',*,*,#6337,.F.);
#8771=ORIENTED_EDGE('',*,*,#6334,.T.);
#8772=ORIENTED_EDGE('',*,*,#6338,.F.);
#8773=ORIENTED_EDGE('',*,*,#6339,.T.);
#8774=ORIENTED_EDGE('',*,*,#5599,.T.);
#8775=ORIENTED_EDGE('',*,*,#5999,.F.);
#8776=ORIENTED_EDGE('',*,*,#5530,.F.);
#8777=ORIENTED_EDGE('',*,*,#6000,.F.);
#8778=ORIENTED_EDGE('',*,*,#5601,.T.);
#8779=ORIENTED_EDGE('',*,*,#6340,.F.);
#8780=ORIENTED_EDGE('',*,*,#6341,.F.);
#8781=ORIENTED_EDGE('',*,*,#5520,.F.);
#8782=ORIENTED_EDGE('',*,*,#5600,.T.);
#8783=ORIENTED_EDGE('',*,*,#6339,.F.);
#8784=ORIENTED_EDGE('',*,*,#6342,.F.);
#8785=ORIENTED_EDGE('',*,*,#6343,.F.);
#8786=ORIENTED_EDGE('',*,*,#6340,.T.);
#8787=ORIENTED_EDGE('',*,*,#6344,.F.);
#8788=ORIENTED_EDGE('',*,*,#6345,.T.);
#8789=ORIENTED_EDGE('',*,*,#5595,.T.);
#8790=ORIENTED_EDGE('',*,*,#5997,.F.);
#8791=ORIENTED_EDGE('',*,*,#5542,.F.);
#8792=ORIENTED_EDGE('',*,*,#5998,.F.);
#8793=ORIENTED_EDGE('',*,*,#5597,.T.);
#8794=ORIENTED_EDGE('',*,*,#6346,.F.);
#8795=ORIENTED_EDGE('',*,*,#6347,.F.);
#8796=ORIENTED_EDGE('',*,*,#5526,.F.);
#8797=ORIENTED_EDGE('',*,*,#5596,.T.);
#8798=ORIENTED_EDGE('',*,*,#6345,.F.);
#8799=ORIENTED_EDGE('',*,*,#6348,.F.);
#8800=ORIENTED_EDGE('',*,*,#6349,.F.);
#8801=ORIENTED_EDGE('',*,*,#6346,.T.);
#8802=ORIENTED_EDGE('',*,*,#6350,.F.);
#8803=ORIENTED_EDGE('',*,*,#6351,.T.);
#8804=ORIENTED_EDGE('',*,*,#5591,.T.);
#8805=ORIENTED_EDGE('',*,*,#5994,.F.);
#8806=ORIENTED_EDGE('',*,*,#5536,.F.);
#8807=ORIENTED_EDGE('',*,*,#5996,.F.);
#8808=ORIENTED_EDGE('',*,*,#5593,.T.);
#8809=ORIENTED_EDGE('',*,*,#6352,.F.);
#8810=ORIENTED_EDGE('',*,*,#6353,.F.);
#8811=ORIENTED_EDGE('',*,*,#5538,.F.);
#8812=ORIENTED_EDGE('',*,*,#5592,.T.);
#8813=ORIENTED_EDGE('',*,*,#6351,.F.);
#8814=ORIENTED_EDGE('',*,*,#6354,.F.);
#8815=ORIENTED_EDGE('',*,*,#6355,.F.);
#8816=ORIENTED_EDGE('',*,*,#6352,.T.);
#8817=ORIENTED_EDGE('',*,*,#6356,.F.);
#8818=ORIENTED_EDGE('',*,*,#6103,.T.);
#8819=ORIENTED_EDGE('',*,*,#6102,.T.);
#8820=ORIENTED_EDGE('',*,*,#6357,.T.);
#8821=ORIENTED_EDGE('',*,*,#5775,.F.);
#8822=ORIENTED_EDGE('',*,*,#5992,.T.);
#8823=ORIENTED_EDGE('',*,*,#5281,.T.);
#8824=ORIENTED_EDGE('',*,*,#6101,.T.);
#8825=ORIENTED_EDGE('',*,*,#6356,.T.);
#8826=ORIENTED_EDGE('',*,*,#5774,.F.);
#8827=ORIENTED_EDGE('',*,*,#6357,.F.);
#8828=ORIENTED_EDGE('',*,*,#6098,.T.);
#8829=ORIENTED_EDGE('',*,*,#5289,.T.);
#8830=ORIENTED_EDGE('',*,*,#5991,.T.);
#8831=ORIENTED_EDGE('',*,*,#5776,.F.);
#8832=ORIENTED_EDGE('',*,*,#6358,.F.);
#8833=ORIENTED_EDGE('',*,*,#6109,.T.);
#8834=ORIENTED_EDGE('',*,*,#6108,.T.);
#8835=ORIENTED_EDGE('',*,*,#6359,.T.);
#8836=ORIENTED_EDGE('',*,*,#5779,.F.);
#8837=ORIENTED_EDGE('',*,*,#5990,.T.);
#8838=ORIENTED_EDGE('',*,*,#5287,.T.);
#8839=ORIENTED_EDGE('',*,*,#6107,.T.);
#8840=ORIENTED_EDGE('',*,*,#6358,.T.);
#8841=ORIENTED_EDGE('',*,*,#5778,.F.);
#8842=ORIENTED_EDGE('',*,*,#6359,.F.);
#8843=ORIENTED_EDGE('',*,*,#6104,.T.);
#8844=ORIENTED_EDGE('',*,*,#5295,.T.);
#8845=ORIENTED_EDGE('',*,*,#5989,.T.);
#8846=ORIENTED_EDGE('',*,*,#5780,.F.);
#8847=ORIENTED_EDGE('',*,*,#6360,.F.);
#8848=ORIENTED_EDGE('',*,*,#6115,.T.);
#8849=ORIENTED_EDGE('',*,*,#6114,.T.);
#8850=ORIENTED_EDGE('',*,*,#6361,.T.);
#8851=ORIENTED_EDGE('',*,*,#5783,.F.);
#8852=ORIENTED_EDGE('',*,*,#5988,.T.);
#8853=ORIENTED_EDGE('',*,*,#5293,.T.);
#8854=ORIENTED_EDGE('',*,*,#6113,.T.);
#8855=ORIENTED_EDGE('',*,*,#6360,.T.);
#8856=ORIENTED_EDGE('',*,*,#5782,.F.);
#8857=ORIENTED_EDGE('',*,*,#6361,.F.);
#8858=ORIENTED_EDGE('',*,*,#6110,.T.);
#8859=ORIENTED_EDGE('',*,*,#5301,.T.);
#8860=ORIENTED_EDGE('',*,*,#5987,.T.);
#8861=ORIENTED_EDGE('',*,*,#5784,.F.);
#8862=ORIENTED_EDGE('',*,*,#6362,.F.);
#8863=ORIENTED_EDGE('',*,*,#6121,.T.);
#8864=ORIENTED_EDGE('',*,*,#6120,.T.);
#8865=ORIENTED_EDGE('',*,*,#6363,.T.);
#8866=ORIENTED_EDGE('',*,*,#5787,.F.);
#8867=ORIENTED_EDGE('',*,*,#5986,.T.);
#8868=ORIENTED_EDGE('',*,*,#5299,.T.);
#8869=ORIENTED_EDGE('',*,*,#6119,.T.);
#8870=ORIENTED_EDGE('',*,*,#6362,.T.);
#8871=ORIENTED_EDGE('',*,*,#5786,.F.);
#8872=ORIENTED_EDGE('',*,*,#6363,.F.);
#8873=ORIENTED_EDGE('',*,*,#6116,.T.);
#8874=ORIENTED_EDGE('',*,*,#5307,.T.);
#8875=ORIENTED_EDGE('',*,*,#5985,.T.);
#8876=ORIENTED_EDGE('',*,*,#5788,.F.);
#8877=ORIENTED_EDGE('',*,*,#6364,.F.);
#8878=ORIENTED_EDGE('',*,*,#6127,.T.);
#8879=ORIENTED_EDGE('',*,*,#6126,.T.);
#8880=ORIENTED_EDGE('',*,*,#6365,.T.);
#8881=ORIENTED_EDGE('',*,*,#5791,.F.);
#8882=ORIENTED_EDGE('',*,*,#5984,.T.);
#8883=ORIENTED_EDGE('',*,*,#5305,.T.);
#8884=ORIENTED_EDGE('',*,*,#6125,.T.);
#8885=ORIENTED_EDGE('',*,*,#6364,.T.);
#8886=ORIENTED_EDGE('',*,*,#5790,.F.);
#8887=ORIENTED_EDGE('',*,*,#6365,.F.);
#8888=ORIENTED_EDGE('',*,*,#6122,.T.);
#8889=ORIENTED_EDGE('',*,*,#5313,.T.);
#8890=ORIENTED_EDGE('',*,*,#5983,.T.);
#8891=ORIENTED_EDGE('',*,*,#5792,.F.);
#8892=ORIENTED_EDGE('',*,*,#6366,.F.);
#8893=ORIENTED_EDGE('',*,*,#6133,.T.);
#8894=ORIENTED_EDGE('',*,*,#6132,.T.);
#8895=ORIENTED_EDGE('',*,*,#6367,.T.);
#8896=ORIENTED_EDGE('',*,*,#5795,.F.);
#8897=ORIENTED_EDGE('',*,*,#5982,.T.);
#8898=ORIENTED_EDGE('',*,*,#5311,.T.);
#8899=ORIENTED_EDGE('',*,*,#6131,.T.);
#8900=ORIENTED_EDGE('',*,*,#6366,.T.);
#8901=ORIENTED_EDGE('',*,*,#5794,.F.);
#8902=ORIENTED_EDGE('',*,*,#6367,.F.);
#8903=ORIENTED_EDGE('',*,*,#6128,.T.);
#8904=ORIENTED_EDGE('',*,*,#5319,.T.);
#8905=ORIENTED_EDGE('',*,*,#5981,.T.);
#8906=ORIENTED_EDGE('',*,*,#5796,.F.);
#8907=ORIENTED_EDGE('',*,*,#6368,.F.);
#8908=ORIENTED_EDGE('',*,*,#6139,.T.);
#8909=ORIENTED_EDGE('',*,*,#6138,.T.);
#8910=ORIENTED_EDGE('',*,*,#6369,.T.);
#8911=ORIENTED_EDGE('',*,*,#5799,.F.);
#8912=ORIENTED_EDGE('',*,*,#5980,.T.);
#8913=ORIENTED_EDGE('',*,*,#5317,.T.);
#8914=ORIENTED_EDGE('',*,*,#6137,.T.);
#8915=ORIENTED_EDGE('',*,*,#6368,.T.);
#8916=ORIENTED_EDGE('',*,*,#5798,.F.);
#8917=ORIENTED_EDGE('',*,*,#6369,.F.);
#8918=ORIENTED_EDGE('',*,*,#6134,.T.);
#8919=ORIENTED_EDGE('',*,*,#5325,.T.);
#8920=ORIENTED_EDGE('',*,*,#5979,.T.);
#8921=ORIENTED_EDGE('',*,*,#5800,.F.);
#8922=ORIENTED_EDGE('',*,*,#6370,.F.);
#8923=ORIENTED_EDGE('',*,*,#6145,.T.);
#8924=ORIENTED_EDGE('',*,*,#6144,.T.);
#8925=ORIENTED_EDGE('',*,*,#6371,.T.);
#8926=ORIENTED_EDGE('',*,*,#5803,.F.);
#8927=ORIENTED_EDGE('',*,*,#5978,.T.);
#8928=ORIENTED_EDGE('',*,*,#5323,.T.);
#8929=ORIENTED_EDGE('',*,*,#6143,.T.);
#8930=ORIENTED_EDGE('',*,*,#6370,.T.);
#8931=ORIENTED_EDGE('',*,*,#5802,.F.);
#8932=ORIENTED_EDGE('',*,*,#6371,.F.);
#8933=ORIENTED_EDGE('',*,*,#6140,.T.);
#8934=ORIENTED_EDGE('',*,*,#5331,.T.);
#8935=ORIENTED_EDGE('',*,*,#5977,.T.);
#8936=ORIENTED_EDGE('',*,*,#5804,.F.);
#8937=ORIENTED_EDGE('',*,*,#6372,.F.);
#8938=ORIENTED_EDGE('',*,*,#6151,.T.);
#8939=ORIENTED_EDGE('',*,*,#6150,.T.);
#8940=ORIENTED_EDGE('',*,*,#6373,.T.);
#8941=ORIENTED_EDGE('',*,*,#5807,.F.);
#8942=ORIENTED_EDGE('',*,*,#5976,.T.);
#8943=ORIENTED_EDGE('',*,*,#5329,.T.);
#8944=ORIENTED_EDGE('',*,*,#6149,.T.);
#8945=ORIENTED_EDGE('',*,*,#6372,.T.);
#8946=ORIENTED_EDGE('',*,*,#5806,.F.);
#8947=ORIENTED_EDGE('',*,*,#6373,.F.);
#8948=ORIENTED_EDGE('',*,*,#6146,.T.);
#8949=ORIENTED_EDGE('',*,*,#5337,.T.);
#8950=ORIENTED_EDGE('',*,*,#5975,.T.);
#8951=ORIENTED_EDGE('',*,*,#5808,.F.);
#8952=ORIENTED_EDGE('',*,*,#6374,.F.);
#8953=ORIENTED_EDGE('',*,*,#6157,.T.);
#8954=ORIENTED_EDGE('',*,*,#6156,.T.);
#8955=ORIENTED_EDGE('',*,*,#6375,.T.);
#8956=ORIENTED_EDGE('',*,*,#5811,.F.);
#8957=ORIENTED_EDGE('',*,*,#5974,.T.);
#8958=ORIENTED_EDGE('',*,*,#5335,.T.);
#8959=ORIENTED_EDGE('',*,*,#6155,.T.);
#8960=ORIENTED_EDGE('',*,*,#6374,.T.);
#8961=ORIENTED_EDGE('',*,*,#5810,.F.);
#8962=ORIENTED_EDGE('',*,*,#6375,.F.);
#8963=ORIENTED_EDGE('',*,*,#6152,.T.);
#8964=ORIENTED_EDGE('',*,*,#5343,.T.);
#8965=ORIENTED_EDGE('',*,*,#5973,.T.);
#8966=ORIENTED_EDGE('',*,*,#5812,.F.);
#8967=ORIENTED_EDGE('',*,*,#6376,.F.);
#8968=ORIENTED_EDGE('',*,*,#6163,.T.);
#8969=ORIENTED_EDGE('',*,*,#6162,.T.);
#8970=ORIENTED_EDGE('',*,*,#6377,.T.);
#8971=ORIENTED_EDGE('',*,*,#5818,.F.);
#8972=ORIENTED_EDGE('',*,*,#5815,.F.);
#8973=ORIENTED_EDGE('',*,*,#5972,.T.);
#8974=ORIENTED_EDGE('',*,*,#5341,.T.);
#8975=ORIENTED_EDGE('',*,*,#6161,.T.);
#8976=ORIENTED_EDGE('',*,*,#6376,.T.);
#8977=ORIENTED_EDGE('',*,*,#5814,.F.);
#8978=ORIENTED_EDGE('',*,*,#6377,.F.);
#8979=ORIENTED_EDGE('',*,*,#6158,.T.);
#8980=ORIENTED_EDGE('',*,*,#5349,.T.);
#8981=ORIENTED_EDGE('',*,*,#5971,.T.);
#8982=ORIENTED_EDGE('',*,*,#5819,.F.);
#8983=ORIENTED_EDGE('',*,*,#6378,.F.);
#8984=ORIENTED_EDGE('',*,*,#6169,.T.);
#8985=ORIENTED_EDGE('',*,*,#6168,.T.);
#8986=ORIENTED_EDGE('',*,*,#6379,.T.);
#8987=ORIENTED_EDGE('',*,*,#5822,.F.);
#8988=ORIENTED_EDGE('',*,*,#5970,.T.);
#8989=ORIENTED_EDGE('',*,*,#5347,.T.);
#8990=ORIENTED_EDGE('',*,*,#6167,.T.);
#8991=ORIENTED_EDGE('',*,*,#6378,.T.);
#8992=ORIENTED_EDGE('',*,*,#5821,.F.);
#8993=ORIENTED_EDGE('',*,*,#6379,.F.);
#8994=ORIENTED_EDGE('',*,*,#6164,.T.);
#8995=ORIENTED_EDGE('',*,*,#5355,.T.);
#8996=ORIENTED_EDGE('',*,*,#5969,.T.);
#8997=ORIENTED_EDGE('',*,*,#5823,.F.);
#8998=ORIENTED_EDGE('',*,*,#6380,.F.);
#8999=ORIENTED_EDGE('',*,*,#6175,.T.);
#9000=ORIENTED_EDGE('',*,*,#6174,.T.);
#9001=ORIENTED_EDGE('',*,*,#6381,.T.);
#9002=ORIENTED_EDGE('',*,*,#5826,.F.);
#9003=ORIENTED_EDGE('',*,*,#5968,.T.);
#9004=ORIENTED_EDGE('',*,*,#5353,.T.);
#9005=ORIENTED_EDGE('',*,*,#6173,.T.);
#9006=ORIENTED_EDGE('',*,*,#6380,.T.);
#9007=ORIENTED_EDGE('',*,*,#5825,.F.);
#9008=ORIENTED_EDGE('',*,*,#6381,.F.);
#9009=ORIENTED_EDGE('',*,*,#6170,.T.);
#9010=ORIENTED_EDGE('',*,*,#5361,.T.);
#9011=ORIENTED_EDGE('',*,*,#5967,.T.);
#9012=ORIENTED_EDGE('',*,*,#5827,.F.);
#9013=ORIENTED_EDGE('',*,*,#6382,.F.);
#9014=ORIENTED_EDGE('',*,*,#6181,.T.);
#9015=ORIENTED_EDGE('',*,*,#6180,.T.);
#9016=ORIENTED_EDGE('',*,*,#6383,.T.);
#9017=ORIENTED_EDGE('',*,*,#5830,.F.);
#9018=ORIENTED_EDGE('',*,*,#5966,.T.);
#9019=ORIENTED_EDGE('',*,*,#5359,.T.);
#9020=ORIENTED_EDGE('',*,*,#6179,.T.);
#9021=ORIENTED_EDGE('',*,*,#6382,.T.);
#9022=ORIENTED_EDGE('',*,*,#5829,.F.);
#9023=ORIENTED_EDGE('',*,*,#6383,.F.);
#9024=ORIENTED_EDGE('',*,*,#6176,.T.);
#9025=ORIENTED_EDGE('',*,*,#5367,.T.);
#9026=ORIENTED_EDGE('',*,*,#5965,.T.);
#9027=ORIENTED_EDGE('',*,*,#5831,.F.);
#9028=ORIENTED_EDGE('',*,*,#6384,.F.);
#9029=ORIENTED_EDGE('',*,*,#6184,.T.);
#9030=ORIENTED_EDGE('',*,*,#5373,.T.);
#9031=ORIENTED_EDGE('',*,*,#5963,.T.);
#9032=ORIENTED_EDGE('',*,*,#5835,.F.);
#9033=ORIENTED_EDGE('',*,*,#5964,.T.);
#9034=ORIENTED_EDGE('',*,*,#5365,.T.);
#9035=ORIENTED_EDGE('',*,*,#6183,.T.);
#9036=ORIENTED_EDGE('',*,*,#6385,.T.);
#9037=ORIENTED_EDGE('',*,*,#5833,.F.);
#9038=ORIENTED_EDGE('',*,*,#6385,.F.);
#9039=ORIENTED_EDGE('',*,*,#6187,.T.);
#9040=ORIENTED_EDGE('',*,*,#6186,.T.);
#9041=ORIENTED_EDGE('',*,*,#6384,.T.);
#9042=ORIENTED_EDGE('',*,*,#5834,.F.);
#9043=ORIENTED_EDGE('',*,*,#6386,.F.);
#9044=ORIENTED_EDGE('',*,*,#6193,.T.);
#9045=ORIENTED_EDGE('',*,*,#6192,.T.);
#9046=ORIENTED_EDGE('',*,*,#6387,.T.);
#9047=ORIENTED_EDGE('',*,*,#5838,.F.);
#9048=ORIENTED_EDGE('',*,*,#5962,.T.);
#9049=ORIENTED_EDGE('',*,*,#5371,.T.);
#9050=ORIENTED_EDGE('',*,*,#6191,.T.);
#9051=ORIENTED_EDGE('',*,*,#6386,.T.);
#9052=ORIENTED_EDGE('',*,*,#5837,.F.);
#9053=ORIENTED_EDGE('',*,*,#6387,.F.);
#9054=ORIENTED_EDGE('',*,*,#6188,.T.);
#9055=ORIENTED_EDGE('',*,*,#5379,.T.);
#9056=ORIENTED_EDGE('',*,*,#5961,.T.);
#9057=ORIENTED_EDGE('',*,*,#5839,.F.);
#9058=ORIENTED_EDGE('',*,*,#6388,.F.);
#9059=ORIENTED_EDGE('',*,*,#6199,.T.);
#9060=ORIENTED_EDGE('',*,*,#6198,.T.);
#9061=ORIENTED_EDGE('',*,*,#6389,.T.);
#9062=ORIENTED_EDGE('',*,*,#5842,.F.);
#9063=ORIENTED_EDGE('',*,*,#5960,.T.);
#9064=ORIENTED_EDGE('',*,*,#5377,.T.);
#9065=ORIENTED_EDGE('',*,*,#6197,.T.);
#9066=ORIENTED_EDGE('',*,*,#6388,.T.);
#9067=ORIENTED_EDGE('',*,*,#5841,.F.);
#9068=ORIENTED_EDGE('',*,*,#6389,.F.);
#9069=ORIENTED_EDGE('',*,*,#6194,.T.);
#9070=ORIENTED_EDGE('',*,*,#5385,.T.);
#9071=ORIENTED_EDGE('',*,*,#5959,.T.);
#9072=ORIENTED_EDGE('',*,*,#5843,.F.);
#9073=ORIENTED_EDGE('',*,*,#6390,.F.);
#9074=ORIENTED_EDGE('',*,*,#6205,.T.);
#9075=ORIENTED_EDGE('',*,*,#6204,.T.);
#9076=ORIENTED_EDGE('',*,*,#6391,.T.);
#9077=ORIENTED_EDGE('',*,*,#5846,.F.);
#9078=ORIENTED_EDGE('',*,*,#5958,.T.);
#9079=ORIENTED_EDGE('',*,*,#5383,.T.);
#9080=ORIENTED_EDGE('',*,*,#6203,.T.);
#9081=ORIENTED_EDGE('',*,*,#6390,.T.);
#9082=ORIENTED_EDGE('',*,*,#5845,.F.);
#9083=ORIENTED_EDGE('',*,*,#6391,.F.);
#9084=ORIENTED_EDGE('',*,*,#6200,.T.);
#9085=ORIENTED_EDGE('',*,*,#5391,.T.);
#9086=ORIENTED_EDGE('',*,*,#5957,.T.);
#9087=ORIENTED_EDGE('',*,*,#5847,.F.);
#9088=ORIENTED_EDGE('',*,*,#6392,.F.);
#9089=ORIENTED_EDGE('',*,*,#6211,.T.);
#9090=ORIENTED_EDGE('',*,*,#6210,.T.);
#9091=ORIENTED_EDGE('',*,*,#6393,.T.);
#9092=ORIENTED_EDGE('',*,*,#5850,.F.);
#9093=ORIENTED_EDGE('',*,*,#5956,.T.);
#9094=ORIENTED_EDGE('',*,*,#5389,.T.);
#9095=ORIENTED_EDGE('',*,*,#6209,.T.);
#9096=ORIENTED_EDGE('',*,*,#6392,.T.);
#9097=ORIENTED_EDGE('',*,*,#5849,.F.);
#9098=ORIENTED_EDGE('',*,*,#6393,.F.);
#9099=ORIENTED_EDGE('',*,*,#6206,.T.);
#9100=ORIENTED_EDGE('',*,*,#5397,.T.);
#9101=ORIENTED_EDGE('',*,*,#5955,.T.);
#9102=ORIENTED_EDGE('',*,*,#5851,.F.);
#9103=ORIENTED_EDGE('',*,*,#6394,.F.);
#9104=ORIENTED_EDGE('',*,*,#6217,.T.);
#9105=ORIENTED_EDGE('',*,*,#6216,.T.);
#9106=ORIENTED_EDGE('',*,*,#6395,.T.);
#9107=ORIENTED_EDGE('',*,*,#5854,.F.);
#9108=ORIENTED_EDGE('',*,*,#5954,.T.);
#9109=ORIENTED_EDGE('',*,*,#5395,.T.);
#9110=ORIENTED_EDGE('',*,*,#6215,.T.);
#9111=ORIENTED_EDGE('',*,*,#6394,.T.);
#9112=ORIENTED_EDGE('',*,*,#5853,.F.);
#9113=ORIENTED_EDGE('',*,*,#6395,.F.);
#9114=ORIENTED_EDGE('',*,*,#6212,.T.);
#9115=ORIENTED_EDGE('',*,*,#5403,.T.);
#9116=ORIENTED_EDGE('',*,*,#5953,.T.);
#9117=ORIENTED_EDGE('',*,*,#5855,.F.);
#9118=ORIENTED_EDGE('',*,*,#6396,.F.);
#9119=ORIENTED_EDGE('',*,*,#6223,.T.);
#9120=ORIENTED_EDGE('',*,*,#6222,.T.);
#9121=ORIENTED_EDGE('',*,*,#6397,.T.);
#9122=ORIENTED_EDGE('',*,*,#5858,.F.);
#9123=ORIENTED_EDGE('',*,*,#5952,.T.);
#9124=ORIENTED_EDGE('',*,*,#5401,.T.);
#9125=ORIENTED_EDGE('',*,*,#6221,.T.);
#9126=ORIENTED_EDGE('',*,*,#6396,.T.);
#9127=ORIENTED_EDGE('',*,*,#5857,.F.);
#9128=ORIENTED_EDGE('',*,*,#6397,.F.);
#9129=ORIENTED_EDGE('',*,*,#6218,.T.);
#9130=ORIENTED_EDGE('',*,*,#5409,.T.);
#9131=ORIENTED_EDGE('',*,*,#5951,.T.);
#9132=ORIENTED_EDGE('',*,*,#5859,.F.);
#9133=ORIENTED_EDGE('',*,*,#6398,.F.);
#9134=ORIENTED_EDGE('',*,*,#6229,.T.);
#9135=ORIENTED_EDGE('',*,*,#6228,.T.);
#9136=ORIENTED_EDGE('',*,*,#6399,.T.);
#9137=ORIENTED_EDGE('',*,*,#5862,.F.);
#9138=ORIENTED_EDGE('',*,*,#5950,.T.);
#9139=ORIENTED_EDGE('',*,*,#5407,.T.);
#9140=ORIENTED_EDGE('',*,*,#6227,.T.);
#9141=ORIENTED_EDGE('',*,*,#6398,.T.);
#9142=ORIENTED_EDGE('',*,*,#5861,.F.);
#9143=ORIENTED_EDGE('',*,*,#6399,.F.);
#9144=ORIENTED_EDGE('',*,*,#6224,.T.);
#9145=ORIENTED_EDGE('',*,*,#5415,.T.);
#9146=ORIENTED_EDGE('',*,*,#5949,.T.);
#9147=ORIENTED_EDGE('',*,*,#5863,.F.);
#9148=ORIENTED_EDGE('',*,*,#6400,.F.);
#9149=ORIENTED_EDGE('',*,*,#6235,.T.);
#9150=ORIENTED_EDGE('',*,*,#6234,.T.);
#9151=ORIENTED_EDGE('',*,*,#6401,.T.);
#9152=ORIENTED_EDGE('',*,*,#5866,.F.);
#9153=ORIENTED_EDGE('',*,*,#5948,.T.);
#9154=ORIENTED_EDGE('',*,*,#5413,.T.);
#9155=ORIENTED_EDGE('',*,*,#6233,.T.);
#9156=ORIENTED_EDGE('',*,*,#6400,.T.);
#9157=ORIENTED_EDGE('',*,*,#5865,.F.);
#9158=ORIENTED_EDGE('',*,*,#6401,.F.);
#9159=ORIENTED_EDGE('',*,*,#6230,.T.);
#9160=ORIENTED_EDGE('',*,*,#5421,.T.);
#9161=ORIENTED_EDGE('',*,*,#5947,.T.);
#9162=ORIENTED_EDGE('',*,*,#5867,.F.);
#9163=ORIENTED_EDGE('',*,*,#6402,.F.);
#9164=ORIENTED_EDGE('',*,*,#6241,.T.);
#9165=ORIENTED_EDGE('',*,*,#6240,.T.);
#9166=ORIENTED_EDGE('',*,*,#6403,.T.);
#9167=ORIENTED_EDGE('',*,*,#5870,.F.);
#9168=ORIENTED_EDGE('',*,*,#5946,.T.);
#9169=ORIENTED_EDGE('',*,*,#5419,.T.);
#9170=ORIENTED_EDGE('',*,*,#6239,.T.);
#9171=ORIENTED_EDGE('',*,*,#6402,.T.);
#9172=ORIENTED_EDGE('',*,*,#5869,.F.);
#9173=ORIENTED_EDGE('',*,*,#6403,.F.);
#9174=ORIENTED_EDGE('',*,*,#6236,.T.);
#9175=ORIENTED_EDGE('',*,*,#5427,.T.);
#9176=ORIENTED_EDGE('',*,*,#5945,.T.);
#9177=ORIENTED_EDGE('',*,*,#5871,.F.);
#9178=ORIENTED_EDGE('',*,*,#6404,.F.);
#9179=ORIENTED_EDGE('',*,*,#6247,.T.);
#9180=ORIENTED_EDGE('',*,*,#6246,.T.);
#9181=ORIENTED_EDGE('',*,*,#6405,.T.);
#9182=ORIENTED_EDGE('',*,*,#5874,.F.);
#9183=ORIENTED_EDGE('',*,*,#5944,.T.);
#9184=ORIENTED_EDGE('',*,*,#5425,.T.);
#9185=ORIENTED_EDGE('',*,*,#6245,.T.);
#9186=ORIENTED_EDGE('',*,*,#6404,.T.);
#9187=ORIENTED_EDGE('',*,*,#5873,.F.);
#9188=ORIENTED_EDGE('',*,*,#6405,.F.);
#9189=ORIENTED_EDGE('',*,*,#6242,.T.);
#9190=ORIENTED_EDGE('',*,*,#5433,.T.);
#9191=ORIENTED_EDGE('',*,*,#5943,.T.);
#9192=ORIENTED_EDGE('',*,*,#5875,.F.);
#9193=ORIENTED_EDGE('',*,*,#6406,.F.);
#9194=ORIENTED_EDGE('',*,*,#6253,.T.);
#9195=ORIENTED_EDGE('',*,*,#6252,.T.);
#9196=ORIENTED_EDGE('',*,*,#6407,.T.);
#9197=ORIENTED_EDGE('',*,*,#5878,.F.);
#9198=ORIENTED_EDGE('',*,*,#5942,.T.);
#9199=ORIENTED_EDGE('',*,*,#5431,.T.);
#9200=ORIENTED_EDGE('',*,*,#6251,.T.);
#9201=ORIENTED_EDGE('',*,*,#6406,.T.);
#9202=ORIENTED_EDGE('',*,*,#5877,.F.);
#9203=ORIENTED_EDGE('',*,*,#6407,.F.);
#9204=ORIENTED_EDGE('',*,*,#6248,.T.);
#9205=ORIENTED_EDGE('',*,*,#5439,.T.);
#9206=ORIENTED_EDGE('',*,*,#5941,.T.);
#9207=ORIENTED_EDGE('',*,*,#5879,.F.);
#9208=ORIENTED_EDGE('',*,*,#6408,.F.);
#9209=ORIENTED_EDGE('',*,*,#6259,.T.);
#9210=ORIENTED_EDGE('',*,*,#6258,.T.);
#9211=ORIENTED_EDGE('',*,*,#6409,.T.);
#9212=ORIENTED_EDGE('',*,*,#5882,.F.);
#9213=ORIENTED_EDGE('',*,*,#5940,.T.);
#9214=ORIENTED_EDGE('',*,*,#5437,.T.);
#9215=ORIENTED_EDGE('',*,*,#6257,.T.);
#9216=ORIENTED_EDGE('',*,*,#6408,.T.);
#9217=ORIENTED_EDGE('',*,*,#5881,.F.);
#9218=ORIENTED_EDGE('',*,*,#6409,.F.);
#9219=ORIENTED_EDGE('',*,*,#6254,.T.);
#9220=ORIENTED_EDGE('',*,*,#5445,.T.);
#9221=ORIENTED_EDGE('',*,*,#5939,.T.);
#9222=ORIENTED_EDGE('',*,*,#5883,.F.);
#9223=ORIENTED_EDGE('',*,*,#6410,.F.);
#9224=ORIENTED_EDGE('',*,*,#6265,.T.);
#9225=ORIENTED_EDGE('',*,*,#6264,.T.);
#9226=ORIENTED_EDGE('',*,*,#6411,.T.);
#9227=ORIENTED_EDGE('',*,*,#5886,.F.);
#9228=ORIENTED_EDGE('',*,*,#5938,.T.);
#9229=ORIENTED_EDGE('',*,*,#5443,.T.);
#9230=ORIENTED_EDGE('',*,*,#6263,.T.);
#9231=ORIENTED_EDGE('',*,*,#6410,.T.);
#9232=ORIENTED_EDGE('',*,*,#5885,.F.);
#9233=ORIENTED_EDGE('',*,*,#6411,.F.);
#9234=ORIENTED_EDGE('',*,*,#6260,.T.);
#9235=ORIENTED_EDGE('',*,*,#5451,.T.);
#9236=ORIENTED_EDGE('',*,*,#5937,.T.);
#9237=ORIENTED_EDGE('',*,*,#5887,.F.);
#9238=ORIENTED_EDGE('',*,*,#6412,.F.);
#9239=ORIENTED_EDGE('',*,*,#6271,.T.);
#9240=ORIENTED_EDGE('',*,*,#6270,.T.);
#9241=ORIENTED_EDGE('',*,*,#6413,.T.);
#9242=ORIENTED_EDGE('',*,*,#5890,.F.);
#9243=ORIENTED_EDGE('',*,*,#5936,.T.);
#9244=ORIENTED_EDGE('',*,*,#5449,.T.);
#9245=ORIENTED_EDGE('',*,*,#6269,.T.);
#9246=ORIENTED_EDGE('',*,*,#6412,.T.);
#9247=ORIENTED_EDGE('',*,*,#5889,.F.);
#9248=ORIENTED_EDGE('',*,*,#6413,.F.);
#9249=ORIENTED_EDGE('',*,*,#6266,.T.);
#9250=ORIENTED_EDGE('',*,*,#5457,.T.);
#9251=ORIENTED_EDGE('',*,*,#5935,.T.);
#9252=ORIENTED_EDGE('',*,*,#5891,.F.);
#9253=ORIENTED_EDGE('',*,*,#6414,.F.);
#9254=ORIENTED_EDGE('',*,*,#6277,.T.);
#9255=ORIENTED_EDGE('',*,*,#6276,.T.);
#9256=ORIENTED_EDGE('',*,*,#6415,.T.);
#9257=ORIENTED_EDGE('',*,*,#5894,.F.);
#9258=ORIENTED_EDGE('',*,*,#5934,.T.);
#9259=ORIENTED_EDGE('',*,*,#5455,.T.);
#9260=ORIENTED_EDGE('',*,*,#6275,.T.);
#9261=ORIENTED_EDGE('',*,*,#6414,.T.);
#9262=ORIENTED_EDGE('',*,*,#5893,.F.);
#9263=ORIENTED_EDGE('',*,*,#6415,.F.);
#9264=ORIENTED_EDGE('',*,*,#6272,.T.);
#9265=ORIENTED_EDGE('',*,*,#5463,.T.);
#9266=ORIENTED_EDGE('',*,*,#5933,.T.);
#9267=ORIENTED_EDGE('',*,*,#5895,.F.);
#9268=ORIENTED_EDGE('',*,*,#6416,.F.);
#9269=ORIENTED_EDGE('',*,*,#6283,.T.);
#9270=ORIENTED_EDGE('',*,*,#6282,.T.);
#9271=ORIENTED_EDGE('',*,*,#6417,.T.);
#9272=ORIENTED_EDGE('',*,*,#5898,.F.);
#9273=ORIENTED_EDGE('',*,*,#5932,.T.);
#9274=ORIENTED_EDGE('',*,*,#5461,.T.);
#9275=ORIENTED_EDGE('',*,*,#6281,.T.);
#9276=ORIENTED_EDGE('',*,*,#6416,.T.);
#9277=ORIENTED_EDGE('',*,*,#5897,.F.);
#9278=ORIENTED_EDGE('',*,*,#6417,.F.);
#9279=ORIENTED_EDGE('',*,*,#6278,.T.);
#9280=ORIENTED_EDGE('',*,*,#5469,.T.);
#9281=ORIENTED_EDGE('',*,*,#5931,.T.);
#9282=ORIENTED_EDGE('',*,*,#5899,.F.);
#9283=ORIENTED_EDGE('',*,*,#6418,.F.);
#9284=ORIENTED_EDGE('',*,*,#6289,.T.);
#9285=ORIENTED_EDGE('',*,*,#6288,.T.);
#9286=ORIENTED_EDGE('',*,*,#6419,.T.);
#9287=ORIENTED_EDGE('',*,*,#5902,.F.);
#9288=ORIENTED_EDGE('',*,*,#5930,.T.);
#9289=ORIENTED_EDGE('',*,*,#5467,.T.);
#9290=ORIENTED_EDGE('',*,*,#6287,.T.);
#9291=ORIENTED_EDGE('',*,*,#6418,.T.);
#9292=ORIENTED_EDGE('',*,*,#5901,.F.);
#9293=ORIENTED_EDGE('',*,*,#6419,.F.);
#9294=ORIENTED_EDGE('',*,*,#6284,.T.);
#9295=ORIENTED_EDGE('',*,*,#5475,.T.);
#9296=ORIENTED_EDGE('',*,*,#5929,.T.);
#9297=ORIENTED_EDGE('',*,*,#5903,.F.);
#9298=ORIENTED_EDGE('',*,*,#6420,.F.);
#9299=ORIENTED_EDGE('',*,*,#6295,.T.);
#9300=ORIENTED_EDGE('',*,*,#6294,.T.);
#9301=ORIENTED_EDGE('',*,*,#6421,.T.);
#9302=ORIENTED_EDGE('',*,*,#5727,.F.);
#9303=ORIENTED_EDGE('',*,*,#5928,.T.);
#9304=ORIENTED_EDGE('',*,*,#5473,.T.);
#9305=ORIENTED_EDGE('',*,*,#6293,.T.);
#9306=ORIENTED_EDGE('',*,*,#6420,.T.);
#9307=ORIENTED_EDGE('',*,*,#5905,.F.);
#9308=ORIENTED_EDGE('',*,*,#6421,.F.);
#9309=ORIENTED_EDGE('',*,*,#6290,.T.);
#9310=ORIENTED_EDGE('',*,*,#5481,.T.);
#9311=ORIENTED_EDGE('',*,*,#5927,.T.);
#9312=ORIENTED_EDGE('',*,*,#5728,.F.);
#9313=ORIENTED_EDGE('',*,*,#6422,.F.);
#9314=ORIENTED_EDGE('',*,*,#6301,.T.);
#9315=ORIENTED_EDGE('',*,*,#6300,.T.);
#9316=ORIENTED_EDGE('',*,*,#6423,.T.);
#9317=ORIENTED_EDGE('',*,*,#5731,.F.);
#9318=ORIENTED_EDGE('',*,*,#5926,.T.);
#9319=ORIENTED_EDGE('',*,*,#5479,.T.);
#9320=ORIENTED_EDGE('',*,*,#6299,.T.);
#9321=ORIENTED_EDGE('',*,*,#6422,.T.);
#9322=ORIENTED_EDGE('',*,*,#5730,.F.);
#9323=ORIENTED_EDGE('',*,*,#6423,.F.);
#9324=ORIENTED_EDGE('',*,*,#6296,.T.);
#9325=ORIENTED_EDGE('',*,*,#5487,.T.);
#9326=ORIENTED_EDGE('',*,*,#5925,.T.);
#9327=ORIENTED_EDGE('',*,*,#5732,.F.);
#9328=ORIENTED_EDGE('',*,*,#6424,.F.);
#9329=ORIENTED_EDGE('',*,*,#6307,.T.);
#9330=ORIENTED_EDGE('',*,*,#6306,.T.);
#9331=ORIENTED_EDGE('',*,*,#6425,.T.);
#9332=ORIENTED_EDGE('',*,*,#5735,.F.);
#9333=ORIENTED_EDGE('',*,*,#5924,.T.);
#9334=ORIENTED_EDGE('',*,*,#5485,.T.);
#9335=ORIENTED_EDGE('',*,*,#6305,.T.);
#9336=ORIENTED_EDGE('',*,*,#6424,.T.);
#9337=ORIENTED_EDGE('',*,*,#5734,.F.);
#9338=ORIENTED_EDGE('',*,*,#6425,.F.);
#9339=ORIENTED_EDGE('',*,*,#6302,.T.);
#9340=ORIENTED_EDGE('',*,*,#5493,.T.);
#9341=ORIENTED_EDGE('',*,*,#5923,.T.);
#9342=ORIENTED_EDGE('',*,*,#5736,.F.);
#9343=ORIENTED_EDGE('',*,*,#6426,.F.);
#9344=ORIENTED_EDGE('',*,*,#6313,.T.);
#9345=ORIENTED_EDGE('',*,*,#6312,.T.);
#9346=ORIENTED_EDGE('',*,*,#6427,.T.);
#9347=ORIENTED_EDGE('',*,*,#5739,.F.);
#9348=ORIENTED_EDGE('',*,*,#5922,.T.);
#9349=ORIENTED_EDGE('',*,*,#5491,.T.);
#9350=ORIENTED_EDGE('',*,*,#6311,.T.);
#9351=ORIENTED_EDGE('',*,*,#6426,.T.);
#9352=ORIENTED_EDGE('',*,*,#5738,.F.);
#9353=ORIENTED_EDGE('',*,*,#6427,.F.);
#9354=ORIENTED_EDGE('',*,*,#6308,.T.);
#9355=ORIENTED_EDGE('',*,*,#5499,.T.);
#9356=ORIENTED_EDGE('',*,*,#5921,.T.);
#9357=ORIENTED_EDGE('',*,*,#5740,.F.);
#9358=ORIENTED_EDGE('',*,*,#6428,.F.);
#9359=ORIENTED_EDGE('',*,*,#6316,.T.);
#9360=ORIENTED_EDGE('',*,*,#5505,.T.);
#9361=ORIENTED_EDGE('',*,*,#5919,.T.);
#9362=ORIENTED_EDGE('',*,*,#5744,.F.);
#9363=ORIENTED_EDGE('',*,*,#5920,.T.);
#9364=ORIENTED_EDGE('',*,*,#5497,.T.);
#9365=ORIENTED_EDGE('',*,*,#6315,.T.);
#9366=ORIENTED_EDGE('',*,*,#6429,.T.);
#9367=ORIENTED_EDGE('',*,*,#5742,.F.);
#9368=ORIENTED_EDGE('',*,*,#6429,.F.);
#9369=ORIENTED_EDGE('',*,*,#6319,.T.);
#9370=ORIENTED_EDGE('',*,*,#6318,.T.);
#9371=ORIENTED_EDGE('',*,*,#6428,.T.);
#9372=ORIENTED_EDGE('',*,*,#5743,.F.);
#9373=ORIENTED_EDGE('',*,*,#6430,.F.);
#9374=ORIENTED_EDGE('',*,*,#6325,.T.);
#9375=ORIENTED_EDGE('',*,*,#6324,.T.);
#9376=ORIENTED_EDGE('',*,*,#6431,.T.);
#9377=ORIENTED_EDGE('',*,*,#5747,.F.);
#9378=ORIENTED_EDGE('',*,*,#5918,.T.);
#9379=ORIENTED_EDGE('',*,*,#5503,.T.);
#9380=ORIENTED_EDGE('',*,*,#6323,.T.);
#9381=ORIENTED_EDGE('',*,*,#6430,.T.);
#9382=ORIENTED_EDGE('',*,*,#5746,.F.);
#9383=ORIENTED_EDGE('',*,*,#6431,.F.);
#9384=ORIENTED_EDGE('',*,*,#6320,.T.);
#9385=ORIENTED_EDGE('',*,*,#5511,.T.);
#9386=ORIENTED_EDGE('',*,*,#5917,.T.);
#9387=ORIENTED_EDGE('',*,*,#5748,.F.);
#9388=ORIENTED_EDGE('',*,*,#6432,.F.);
#9389=ORIENTED_EDGE('',*,*,#6331,.T.);
#9390=ORIENTED_EDGE('',*,*,#6330,.T.);
#9391=ORIENTED_EDGE('',*,*,#6433,.T.);
#9392=ORIENTED_EDGE('',*,*,#5751,.F.);
#9393=ORIENTED_EDGE('',*,*,#5916,.T.);
#9394=ORIENTED_EDGE('',*,*,#5509,.T.);
#9395=ORIENTED_EDGE('',*,*,#6329,.T.);
#9396=ORIENTED_EDGE('',*,*,#6432,.T.);
#9397=ORIENTED_EDGE('',*,*,#5750,.F.);
#9398=ORIENTED_EDGE('',*,*,#6433,.F.);
#9399=ORIENTED_EDGE('',*,*,#6326,.T.);
#9400=ORIENTED_EDGE('',*,*,#5517,.T.);
#9401=ORIENTED_EDGE('',*,*,#5915,.T.);
#9402=ORIENTED_EDGE('',*,*,#5752,.F.);
#9403=ORIENTED_EDGE('',*,*,#6434,.F.);
#9404=ORIENTED_EDGE('',*,*,#6337,.T.);
#9405=ORIENTED_EDGE('',*,*,#6336,.T.);
#9406=ORIENTED_EDGE('',*,*,#6435,.T.);
#9407=ORIENTED_EDGE('',*,*,#5755,.F.);
#9408=ORIENTED_EDGE('',*,*,#5914,.T.);
#9409=ORIENTED_EDGE('',*,*,#5515,.T.);
#9410=ORIENTED_EDGE('',*,*,#6335,.T.);
#9411=ORIENTED_EDGE('',*,*,#6434,.T.);
#9412=ORIENTED_EDGE('',*,*,#5754,.F.);
#9413=ORIENTED_EDGE('',*,*,#6435,.F.);
#9414=ORIENTED_EDGE('',*,*,#6332,.T.);
#9415=ORIENTED_EDGE('',*,*,#5523,.T.);
#9416=ORIENTED_EDGE('',*,*,#5913,.T.);
#9417=ORIENTED_EDGE('',*,*,#5756,.F.);
#9418=ORIENTED_EDGE('',*,*,#6436,.F.);
#9419=ORIENTED_EDGE('',*,*,#6343,.T.);
#9420=ORIENTED_EDGE('',*,*,#6342,.T.);
#9421=ORIENTED_EDGE('',*,*,#6437,.T.);
#9422=ORIENTED_EDGE('',*,*,#5759,.F.);
#9423=ORIENTED_EDGE('',*,*,#5912,.T.);
#9424=ORIENTED_EDGE('',*,*,#5521,.T.);
#9425=ORIENTED_EDGE('',*,*,#6341,.T.);
#9426=ORIENTED_EDGE('',*,*,#6436,.T.);
#9427=ORIENTED_EDGE('',*,*,#5758,.F.);
#9428=ORIENTED_EDGE('',*,*,#6437,.F.);
#9429=ORIENTED_EDGE('',*,*,#6338,.T.);
#9430=ORIENTED_EDGE('',*,*,#5529,.T.);
#9431=ORIENTED_EDGE('',*,*,#5911,.T.);
#9432=ORIENTED_EDGE('',*,*,#5760,.F.);
#9433=ORIENTED_EDGE('',*,*,#6438,.F.);
#9434=ORIENTED_EDGE('',*,*,#6349,.T.);
#9435=ORIENTED_EDGE('',*,*,#6348,.T.);
#9436=ORIENTED_EDGE('',*,*,#6439,.T.);
#9437=ORIENTED_EDGE('',*,*,#5763,.F.);
#9438=ORIENTED_EDGE('',*,*,#5910,.T.);
#9439=ORIENTED_EDGE('',*,*,#5527,.T.);
#9440=ORIENTED_EDGE('',*,*,#6347,.T.);
#9441=ORIENTED_EDGE('',*,*,#6438,.T.);
#9442=ORIENTED_EDGE('',*,*,#5762,.F.);
#9443=ORIENTED_EDGE('',*,*,#6439,.F.);
#9444=ORIENTED_EDGE('',*,*,#6344,.T.);
#9445=ORIENTED_EDGE('',*,*,#5541,.T.);
#9446=ORIENTED_EDGE('',*,*,#5907,.T.);
#9447=ORIENTED_EDGE('',*,*,#5764,.F.);
#9448=ORIENTED_EDGE('',*,*,#6440,.F.);
#9449=ORIENTED_EDGE('',*,*,#6355,.T.);
#9450=ORIENTED_EDGE('',*,*,#6354,.T.);
#9451=ORIENTED_EDGE('',*,*,#6441,.T.);
#9452=ORIENTED_EDGE('',*,*,#5767,.F.);
#9453=ORIENTED_EDGE('',*,*,#5906,.T.);
#9454=ORIENTED_EDGE('',*,*,#5539,.T.);
#9455=ORIENTED_EDGE('',*,*,#6353,.T.);
#9456=ORIENTED_EDGE('',*,*,#6440,.T.);
#9457=ORIENTED_EDGE('',*,*,#5766,.F.);
#9458=ORIENTED_EDGE('',*,*,#6441,.F.);
#9459=ORIENTED_EDGE('',*,*,#6350,.T.);
#9460=ORIENTED_EDGE('',*,*,#5535,.T.);
#9461=ORIENTED_EDGE('',*,*,#5908,.T.);
#9462=ORIENTED_EDGE('',*,*,#5768,.F.);
#9463=ORIENTED_EDGE('',*,*,#6442,.F.);
#9464=ORIENTED_EDGE('',*,*,#6443,.T.);
#9465=ORIENTED_EDGE('',*,*,#6444,.T.);
#9466=ORIENTED_EDGE('',*,*,#6443,.F.);
#9467=ORIENTED_EDGE('',*,*,#6445,.F.);
#9468=ORIENTED_EDGE('',*,*,#6446,.T.);
#9469=ORIENTED_EDGE('',*,*,#6447,.T.);
#9470=ORIENTED_EDGE('',*,*,#6446,.F.);
#9471=ORIENTED_EDGE('',*,*,#6448,.F.);
#9472=ORIENTED_EDGE('',*,*,#6449,.T.);
#9473=ORIENTED_EDGE('',*,*,#6450,.F.);
#9474=ORIENTED_EDGE('',*,*,#6449,.F.);
#9475=ORIENTED_EDGE('',*,*,#6451,.F.);
#9476=ORIENTED_EDGE('',*,*,#6452,.T.);
#9477=ORIENTED_EDGE('',*,*,#6453,.F.);
#9478=ORIENTED_EDGE('',*,*,#6452,.F.);
#9479=ORIENTED_EDGE('',*,*,#6454,.T.);
#9480=ORIENTED_EDGE('',*,*,#6455,.T.);
#9481=ORIENTED_EDGE('',*,*,#6456,.F.);
#9482=ORIENTED_EDGE('',*,*,#6455,.F.);
#9483=ORIENTED_EDGE('',*,*,#6457,.T.);
#9484=ORIENTED_EDGE('',*,*,#6458,.T.);
#9485=ORIENTED_EDGE('',*,*,#6459,.F.);
#9486=ORIENTED_EDGE('',*,*,#6458,.F.);
#9487=ORIENTED_EDGE('',*,*,#6460,.T.);
#9488=ORIENTED_EDGE('',*,*,#6461,.T.);
#9489=ORIENTED_EDGE('',*,*,#6462,.F.);
#9490=ORIENTED_EDGE('',*,*,#6461,.F.);
#9491=ORIENTED_EDGE('',*,*,#6463,.T.);
#9492=ORIENTED_EDGE('',*,*,#6464,.T.);
#9493=ORIENTED_EDGE('',*,*,#6465,.F.);
#9494=ORIENTED_EDGE('',*,*,#6464,.F.);
#9495=ORIENTED_EDGE('',*,*,#6466,.T.);
#9496=ORIENTED_EDGE('',*,*,#6467,.T.);
#9497=ORIENTED_EDGE('',*,*,#6468,.F.);
#9498=ORIENTED_EDGE('',*,*,#6467,.F.);
#9499=ORIENTED_EDGE('',*,*,#6469,.T.);
#9500=ORIENTED_EDGE('',*,*,#6470,.T.);
#9501=ORIENTED_EDGE('',*,*,#6471,.F.);
#9502=ORIENTED_EDGE('',*,*,#6470,.F.);
#9503=ORIENTED_EDGE('',*,*,#6472,.T.);
#9504=ORIENTED_EDGE('',*,*,#6473,.T.);
#9505=ORIENTED_EDGE('',*,*,#6474,.F.);
#9506=ORIENTED_EDGE('',*,*,#6473,.F.);
#9507=ORIENTED_EDGE('',*,*,#6475,.T.);
#9508=ORIENTED_EDGE('',*,*,#6476,.T.);
#9509=ORIENTED_EDGE('',*,*,#6477,.F.);
#9510=ORIENTED_EDGE('',*,*,#6476,.F.);
#9511=ORIENTED_EDGE('',*,*,#6478,.T.);
#9512=ORIENTED_EDGE('',*,*,#6479,.T.);
#9513=ORIENTED_EDGE('',*,*,#6480,.F.);
#9514=ORIENTED_EDGE('',*,*,#6479,.F.);
#9515=ORIENTED_EDGE('',*,*,#6481,.T.);
#9516=ORIENTED_EDGE('',*,*,#6482,.F.);
#9517=ORIENTED_EDGE('',*,*,#6483,.F.);
#9518=ORIENTED_EDGE('',*,*,#6484,.F.);
#9519=ORIENTED_EDGE('',*,*,#6485,.T.);
#9520=ORIENTED_EDGE('',*,*,#6486,.T.);
#9521=ORIENTED_EDGE('',*,*,#6487,.T.);
#9522=ORIENTED_EDGE('',*,*,#6488,.T.);
#9523=ORIENTED_EDGE('',*,*,#6489,.T.);
#9524=ORIENTED_EDGE('',*,*,#6490,.F.);
#9525=ORIENTED_EDGE('',*,*,#6491,.T.);
#9526=ORIENTED_EDGE('',*,*,#6492,.T.);
#9527=ORIENTED_EDGE('',*,*,#6493,.T.);
#9528=ORIENTED_EDGE('',*,*,#6494,.T.);
#9529=ORIENTED_EDGE('',*,*,#6495,.T.);
#9530=ORIENTED_EDGE('',*,*,#6496,.F.);
#9531=ORIENTED_EDGE('',*,*,#6497,.T.);
#9532=ORIENTED_EDGE('',*,*,#6498,.F.);
#9533=ORIENTED_EDGE('',*,*,#6499,.T.);
#9534=ORIENTED_EDGE('',*,*,#6500,.T.);
#9535=ORIENTED_EDGE('',*,*,#6501,.T.);
#9536=ORIENTED_EDGE('',*,*,#6502,.T.);
#9537=ORIENTED_EDGE('',*,*,#6503,.T.);
#9538=ORIENTED_EDGE('',*,*,#6504,.F.);
#9539=ORIENTED_EDGE('',*,*,#6505,.T.);
#9540=ORIENTED_EDGE('',*,*,#6486,.F.);
#9541=ORIENTED_EDGE('',*,*,#6506,.T.);
#9542=ORIENTED_EDGE('',*,*,#6492,.F.);
#9543=ORIENTED_EDGE('',*,*,#6507,.T.);
#9544=ORIENTED_EDGE('',*,*,#6494,.F.);
#9545=ORIENTED_EDGE('',*,*,#6508,.T.);
#9546=ORIENTED_EDGE('',*,*,#6509,.F.);
#9547=ORIENTED_EDGE('',*,*,#6510,.F.);
#9548=ORIENTED_EDGE('',*,*,#6511,.F.);
#9549=ORIENTED_EDGE('',*,*,#6453,.T.);
#9550=ORIENTED_EDGE('',*,*,#6450,.T.);
#9551=ORIENTED_EDGE('',*,*,#6512,.T.);
#9552=ORIENTED_EDGE('',*,*,#6513,.F.);
#9553=ORIENTED_EDGE('',*,*,#6514,.F.);
#9554=ORIENTED_EDGE('',*,*,#6515,.F.);
#9555=ORIENTED_EDGE('',*,*,#6516,.T.);
#9556=ORIENTED_EDGE('',*,*,#6517,.T.);
#9557=ORIENTED_EDGE('',*,*,#6518,.T.);
#9558=ORIENTED_EDGE('',*,*,#6509,.T.);
#9559=ORIENTED_EDGE('',*,*,#6519,.T.);
#9560=ORIENTED_EDGE('',*,*,#6517,.F.);
#9561=ORIENTED_EDGE('',*,*,#6520,.F.);
#9562=ORIENTED_EDGE('',*,*,#6500,.F.);
#9563=ORIENTED_EDGE('',*,*,#6521,.F.);
#9564=ORIENTED_EDGE('',*,*,#6502,.F.);
#9565=ORIENTED_EDGE('',*,*,#6522,.F.);
#9566=ORIENTED_EDGE('',*,*,#6488,.F.);
#9567=ORIENTED_EDGE('',*,*,#6523,.F.);
#9568=ORIENTED_EDGE('',*,*,#6524,.F.);
#9569=ORIENTED_EDGE('',*,*,#6454,.F.);
#9570=ORIENTED_EDGE('',*,*,#6457,.F.);
#9571=ORIENTED_EDGE('',*,*,#6510,.T.);
#9572=ORIENTED_EDGE('',*,*,#6518,.F.);
#9573=ORIENTED_EDGE('',*,*,#6519,.F.);
#9574=ORIENTED_EDGE('',*,*,#6525,.F.);
#9575=ORIENTED_EDGE('',*,*,#6523,.T.);
#9576=ORIENTED_EDGE('',*,*,#6487,.F.);
#9577=ORIENTED_EDGE('',*,*,#6505,.F.);
#9578=ORIENTED_EDGE('',*,*,#6526,.F.);
#9579=ORIENTED_EDGE('',*,*,#6444,.F.);
#9580=ORIENTED_EDGE('',*,*,#6527,.T.);
#9581=ORIENTED_EDGE('',*,*,#6484,.T.);
#9582=ORIENTED_EDGE('',*,*,#6528,.F.);
#9583=ORIENTED_EDGE('',*,*,#6529,.F.);
#9584=ORIENTED_EDGE('',*,*,#6530,.T.);
#9585=ORIENTED_EDGE('',*,*,#6513,.T.);
#9586=ORIENTED_EDGE('',*,*,#6531,.T.);
#9587=ORIENTED_EDGE('',*,*,#6496,.T.);
#9588=ORIENTED_EDGE('',*,*,#6532,.T.);
#9589=ORIENTED_EDGE('',*,*,#6490,.T.);
#9590=ORIENTED_EDGE('',*,*,#6448,.T.);
#9591=ORIENTED_EDGE('',*,*,#6451,.T.);
#9592=ORIENTED_EDGE('',*,*,#6483,.T.);
#9593=ORIENTED_EDGE('',*,*,#6533,.F.);
#9594=ORIENTED_EDGE('',*,*,#6534,.F.);
#9595=ORIENTED_EDGE('',*,*,#6528,.T.);
#9596=ORIENTED_EDGE('',*,*,#6442,.T.);
#9597=ORIENTED_EDGE('',*,*,#6535,.T.);
#9598=ORIENTED_EDGE('',*,*,#6504,.T.);
#9599=ORIENTED_EDGE('',*,*,#6536,.T.);
#9600=ORIENTED_EDGE('',*,*,#6498,.T.);
#9601=ORIENTED_EDGE('',*,*,#6537,.T.);
#9602=ORIENTED_EDGE('',*,*,#6515,.T.);
#9603=ORIENTED_EDGE('',*,*,#6538,.F.);
#9604=ORIENTED_EDGE('',*,*,#6539,.F.);
#9605=ORIENTED_EDGE('',*,*,#6533,.T.);
#9606=ORIENTED_EDGE('',*,*,#6482,.T.);
#9607=ORIENTED_EDGE('',*,*,#6456,.T.);
#9608=ORIENTED_EDGE('',*,*,#6459,.T.);
#9609=ORIENTED_EDGE('',*,*,#6514,.T.);
#9610=ORIENTED_EDGE('',*,*,#6530,.F.);
#9611=ORIENTED_EDGE('',*,*,#6540,.F.);
#9612=ORIENTED_EDGE('',*,*,#6538,.T.);
#9613=ORIENTED_EDGE('',*,*,#6529,.T.);
#9614=ORIENTED_EDGE('',*,*,#6534,.T.);
#9615=ORIENTED_EDGE('',*,*,#6539,.T.);
#9616=ORIENTED_EDGE('',*,*,#6540,.T.);
#9617=ORIENTED_EDGE('',*,*,#6445,.T.);
#9618=ORIENTED_EDGE('',*,*,#6460,.F.);
#9619=ORIENTED_EDGE('',*,*,#6463,.F.);
#9620=ORIENTED_EDGE('',*,*,#6466,.F.);
#9621=ORIENTED_EDGE('',*,*,#6469,.F.);
#9622=ORIENTED_EDGE('',*,*,#6472,.F.);
#9623=ORIENTED_EDGE('',*,*,#6475,.F.);
#9624=ORIENTED_EDGE('',*,*,#6478,.F.);
#9625=ORIENTED_EDGE('',*,*,#6541,.F.);
#9626=ORIENTED_EDGE('',*,*,#6542,.F.);
#9627=ORIENTED_EDGE('',*,*,#6543,.F.);
#9628=ORIENTED_EDGE('',*,*,#6544,.F.);
#9629=ORIENTED_EDGE('',*,*,#6462,.T.);
#9630=ORIENTED_EDGE('',*,*,#6465,.T.);
#9631=ORIENTED_EDGE('',*,*,#6468,.T.);
#9632=ORIENTED_EDGE('',*,*,#6471,.T.);
#9633=ORIENTED_EDGE('',*,*,#6474,.T.);
#9634=ORIENTED_EDGE('',*,*,#6477,.T.);
#9635=ORIENTED_EDGE('',*,*,#6480,.T.);
#9636=ORIENTED_EDGE('',*,*,#6447,.F.);
#9637=ORIENTED_EDGE('',*,*,#6503,.F.);
#9638=ORIENTED_EDGE('',*,*,#6521,.T.);
#9639=ORIENTED_EDGE('',*,*,#6499,.F.);
#9640=ORIENTED_EDGE('',*,*,#6536,.F.);
#9641=ORIENTED_EDGE('',*,*,#6497,.F.);
#9642=ORIENTED_EDGE('',*,*,#6520,.T.);
#9643=ORIENTED_EDGE('',*,*,#6516,.F.);
#9644=ORIENTED_EDGE('',*,*,#6537,.F.);
#9645=ORIENTED_EDGE('',*,*,#6481,.F.);
#9646=ORIENTED_EDGE('',*,*,#6522,.T.);
#9647=ORIENTED_EDGE('',*,*,#6501,.F.);
#9648=ORIENTED_EDGE('',*,*,#6535,.F.);
#9649=ORIENTED_EDGE('',*,*,#6491,.F.);
#9650=ORIENTED_EDGE('',*,*,#6532,.F.);
#9651=ORIENTED_EDGE('',*,*,#6495,.F.);
#9652=ORIENTED_EDGE('',*,*,#6507,.F.);
#9653=ORIENTED_EDGE('',*,*,#6493,.F.);
#9654=ORIENTED_EDGE('',*,*,#6531,.F.);
#9655=ORIENTED_EDGE('',*,*,#6512,.F.);
#9656=ORIENTED_EDGE('',*,*,#6508,.F.);
#9657=ORIENTED_EDGE('',*,*,#6485,.F.);
#9658=ORIENTED_EDGE('',*,*,#6527,.F.);
#9659=ORIENTED_EDGE('',*,*,#6489,.F.);
#9660=ORIENTED_EDGE('',*,*,#6506,.F.);
#9661=ORIENTED_EDGE('',*,*,#6545,.T.);
#9662=ORIENTED_EDGE('',*,*,#6542,.T.);
#9663=ORIENTED_EDGE('',*,*,#6546,.T.);
#9664=ORIENTED_EDGE('',*,*,#6511,.T.);
#9665=ORIENTED_EDGE('',*,*,#6546,.F.);
#9666=ORIENTED_EDGE('',*,*,#6541,.T.);
#9667=ORIENTED_EDGE('',*,*,#6547,.T.);
#9668=ORIENTED_EDGE('',*,*,#6526,.T.);
#9669=ORIENTED_EDGE('',*,*,#6545,.F.);
#9670=ORIENTED_EDGE('',*,*,#6525,.T.);
#9671=ORIENTED_EDGE('',*,*,#6548,.T.);
#9672=ORIENTED_EDGE('',*,*,#6543,.T.);
#9673=ORIENTED_EDGE('',*,*,#6547,.F.);
#9674=ORIENTED_EDGE('',*,*,#6544,.T.);
#9675=ORIENTED_EDGE('',*,*,#6548,.F.);
#9676=ORIENTED_EDGE('',*,*,#6524,.T.);
#9677=ORIENTED_EDGE('',*,*,#6549,.T.);
#9678=ORIENTED_EDGE('',*,*,#6550,.T.);
#9679=ORIENTED_EDGE('',*,*,#6551,.T.);
#9680=ORIENTED_EDGE('',*,*,#6552,.T.);
#9681=ORIENTED_EDGE('',*,*,#6553,.T.);
#9682=ORIENTED_EDGE('',*,*,#6554,.T.);
#9683=ORIENTED_EDGE('',*,*,#6555,.T.);
#9684=ORIENTED_EDGE('',*,*,#6556,.T.);
#9685=ORIENTED_EDGE('',*,*,#6557,.T.);
#9686=ORIENTED_EDGE('',*,*,#6558,.T.);
#9687=ORIENTED_EDGE('',*,*,#6559,.T.);
#9688=ORIENTED_EDGE('',*,*,#6560,.T.);
#9689=ORIENTED_EDGE('',*,*,#6561,.T.);
#9690=ORIENTED_EDGE('',*,*,#6562,.T.);
#9691=ORIENTED_EDGE('',*,*,#6563,.T.);
#9692=ORIENTED_EDGE('',*,*,#6564,.T.);
#9693=ORIENTED_EDGE('',*,*,#6565,.T.);
#9694=ORIENTED_EDGE('',*,*,#6566,.T.);
#9695=ORIENTED_EDGE('',*,*,#6567,.T.);
#9696=ORIENTED_EDGE('',*,*,#6568,.T.);
#9697=ORIENTED_EDGE('',*,*,#6569,.T.);
#9698=ORIENTED_EDGE('',*,*,#6570,.T.);
#9699=ORIENTED_EDGE('',*,*,#6571,.T.);
#9700=ORIENTED_EDGE('',*,*,#6572,.T.);
#9701=ORIENTED_EDGE('',*,*,#6573,.F.);
#9702=ORIENTED_EDGE('',*,*,#6549,.F.);
#9703=ORIENTED_EDGE('',*,*,#6574,.F.);
#9704=ORIENTED_EDGE('',*,*,#6571,.F.);
#9705=ORIENTED_EDGE('',*,*,#6575,.F.);
#9706=ORIENTED_EDGE('',*,*,#6573,.T.);
#9707=ORIENTED_EDGE('',*,*,#6576,.F.);
#9708=ORIENTED_EDGE('',*,*,#6577,.F.);
#9709=ORIENTED_EDGE('',*,*,#6574,.T.);
#9710=ORIENTED_EDGE('',*,*,#6578,.F.);
#9711=ORIENTED_EDGE('',*,*,#6576,.T.);
#9712=ORIENTED_EDGE('',*,*,#6570,.F.);
#9713=ORIENTED_EDGE('',*,*,#6579,.F.);
#9714=ORIENTED_EDGE('',*,*,#6555,.F.);
#9715=ORIENTED_EDGE('',*,*,#6575,.T.);
#9716=ORIENTED_EDGE('',*,*,#6554,.F.);
#9717=ORIENTED_EDGE('',*,*,#6580,.F.);
#9718=ORIENTED_EDGE('',*,*,#6550,.F.);
#9719=ORIENTED_EDGE('',*,*,#6581,.F.);
#9720=ORIENTED_EDGE('',*,*,#6551,.F.);
#9721=ORIENTED_EDGE('',*,*,#6582,.F.);
#9722=ORIENTED_EDGE('',*,*,#6565,.F.);
#9723=ORIENTED_EDGE('',*,*,#6578,.T.);
#9724=ORIENTED_EDGE('',*,*,#6552,.F.);
#9725=ORIENTED_EDGE('',*,*,#6583,.F.);
#9726=ORIENTED_EDGE('',*,*,#6564,.F.);
#9727=ORIENTED_EDGE('',*,*,#6577,.T.);
#9728=ORIENTED_EDGE('',*,*,#6563,.F.);
#9729=ORIENTED_EDGE('',*,*,#6584,.F.);
#9730=ORIENTED_EDGE('',*,*,#6572,.F.);
#9731=ORIENTED_EDGE('',*,*,#6585,.F.);
#9732=ORIENTED_EDGE('',*,*,#6569,.F.);
#9733=ORIENTED_EDGE('',*,*,#6586,.F.);
#9734=ORIENTED_EDGE('',*,*,#6559,.F.);
#9735=ORIENTED_EDGE('',*,*,#6579,.T.);
#9736=ORIENTED_EDGE('',*,*,#6585,.T.);
#9737=ORIENTED_EDGE('',*,*,#6587,.F.);
#9738=ORIENTED_EDGE('',*,*,#6582,.T.);
#9739=ORIENTED_EDGE('',*,*,#6580,.T.);
#9740=ORIENTED_EDGE('',*,*,#6588,.F.);
#9741=ORIENTED_EDGE('',*,*,#6583,.T.);
#9742=ORIENTED_EDGE('',*,*,#6581,.T.);
#9743=ORIENTED_EDGE('',*,*,#6589,.F.);
#9744=ORIENTED_EDGE('',*,*,#6586,.T.);
#9745=ORIENTED_EDGE('',*,*,#6584,.T.);
#9746=ORIENTED_EDGE('',*,*,#6590,.F.);
#9747=ORIENTED_EDGE('',*,*,#6587,.T.);
#9748=ORIENTED_EDGE('',*,*,#6558,.F.);
#9749=ORIENTED_EDGE('',*,*,#6591,.F.);
#9750=ORIENTED_EDGE('',*,*,#6556,.F.);
#9751=ORIENTED_EDGE('',*,*,#6588,.T.);
#9752=ORIENTED_EDGE('',*,*,#6553,.F.);
#9753=ORIENTED_EDGE('',*,*,#6592,.F.);
#9754=ORIENTED_EDGE('',*,*,#6566,.F.);
#9755=ORIENTED_EDGE('',*,*,#6589,.T.);
#9756=ORIENTED_EDGE('',*,*,#6568,.F.);
#9757=ORIENTED_EDGE('',*,*,#6593,.F.);
#9758=ORIENTED_EDGE('',*,*,#6561,.F.);
#9759=ORIENTED_EDGE('',*,*,#6590,.T.);
#9760=ORIENTED_EDGE('',*,*,#6562,.F.);
#9761=ORIENTED_EDGE('',*,*,#6594,.F.);
#9762=ORIENTED_EDGE('',*,*,#6560,.F.);
#9763=ORIENTED_EDGE('',*,*,#6592,.T.);
#9764=ORIENTED_EDGE('',*,*,#6591,.T.);
#9765=ORIENTED_EDGE('',*,*,#6595,.F.);
#9766=ORIENTED_EDGE('',*,*,#6594,.T.);
#9767=ORIENTED_EDGE('',*,*,#6593,.T.);
#9768=ORIENTED_EDGE('',*,*,#6596,.F.);
#9769=ORIENTED_EDGE('',*,*,#6595,.T.);
#9770=ORIENTED_EDGE('',*,*,#6557,.F.);
#9771=ORIENTED_EDGE('',*,*,#6596,.T.);
#9772=ORIENTED_EDGE('',*,*,#6567,.F.);
#9773=ORIENTED_EDGE('',*,*,#6597,.T.);
#9774=ORIENTED_EDGE('',*,*,#6598,.T.);
#9775=ORIENTED_EDGE('',*,*,#6599,.F.);
#9776=ORIENTED_EDGE('',*,*,#6598,.F.);
#9777=ORIENTED_EDGE('',*,*,#6600,.T.);
#9778=ORIENTED_EDGE('',*,*,#6601,.T.);
#9779=ORIENTED_EDGE('',*,*,#6602,.F.);
#9780=ORIENTED_EDGE('',*,*,#6601,.F.);
#9781=ORIENTED_EDGE('',*,*,#6603,.T.);
#9782=ORIENTED_EDGE('',*,*,#6604,.T.);
#9783=ORIENTED_EDGE('',*,*,#6605,.F.);
#9784=ORIENTED_EDGE('',*,*,#6604,.F.);
#9785=ORIENTED_EDGE('',*,*,#6606,.T.);
#9786=ORIENTED_EDGE('',*,*,#6607,.T.);
#9787=ORIENTED_EDGE('',*,*,#6608,.F.);
#9788=ORIENTED_EDGE('',*,*,#6607,.F.);
#9789=ORIENTED_EDGE('',*,*,#6609,.T.);
#9790=ORIENTED_EDGE('',*,*,#6610,.T.);
#9791=ORIENTED_EDGE('',*,*,#6611,.F.);
#9792=ORIENTED_EDGE('',*,*,#6610,.F.);
#9793=ORIENTED_EDGE('',*,*,#6612,.T.);
#9794=ORIENTED_EDGE('',*,*,#6613,.T.);
#9795=ORIENTED_EDGE('',*,*,#6614,.F.);
#9796=ORIENTED_EDGE('',*,*,#6613,.F.);
#9797=ORIENTED_EDGE('',*,*,#6615,.T.);
#9798=ORIENTED_EDGE('',*,*,#6616,.T.);
#9799=ORIENTED_EDGE('',*,*,#6617,.F.);
#9800=ORIENTED_EDGE('',*,*,#6616,.F.);
#9801=ORIENTED_EDGE('',*,*,#6618,.T.);
#9802=ORIENTED_EDGE('',*,*,#6619,.T.);
#9803=ORIENTED_EDGE('',*,*,#6620,.F.);
#9804=ORIENTED_EDGE('',*,*,#6619,.F.);
#9805=ORIENTED_EDGE('',*,*,#6620,.T.);
#9806=ORIENTED_EDGE('',*,*,#6615,.F.);
#9807=ORIENTED_EDGE('',*,*,#6609,.F.);
#9808=ORIENTED_EDGE('',*,*,#6603,.F.);
#9809=ORIENTED_EDGE('',*,*,#6597,.F.);
#9810=ORIENTED_EDGE('',*,*,#6600,.F.);
#9811=ORIENTED_EDGE('',*,*,#6606,.F.);
#9812=ORIENTED_EDGE('',*,*,#6612,.F.);
#9813=ORIENTED_EDGE('',*,*,#6618,.F.);
#9814=ORIENTED_EDGE('',*,*,#6617,.T.);
#9815=ORIENTED_EDGE('',*,*,#6614,.T.);
#9816=ORIENTED_EDGE('',*,*,#6611,.T.);
#9817=ORIENTED_EDGE('',*,*,#6608,.T.);
#9818=ORIENTED_EDGE('',*,*,#6605,.T.);
#9819=ORIENTED_EDGE('',*,*,#6602,.T.);
#9820=ORIENTED_EDGE('',*,*,#6599,.T.);
#9821=ORIENTED_EDGE('',*,*,#6621,.T.);
#9822=ORIENTED_EDGE('',*,*,#6622,.T.);
#9823=ORIENTED_EDGE('',*,*,#6623,.F.);
#9824=ORIENTED_EDGE('',*,*,#6622,.F.);
#9825=ORIENTED_EDGE('',*,*,#6624,.T.);
#9826=ORIENTED_EDGE('',*,*,#6625,.T.);
#9827=ORIENTED_EDGE('',*,*,#6626,.F.);
#9828=ORIENTED_EDGE('',*,*,#6625,.F.);
#9829=ORIENTED_EDGE('',*,*,#6627,.T.);
#9830=ORIENTED_EDGE('',*,*,#6628,.T.);
#9831=ORIENTED_EDGE('',*,*,#6629,.F.);
#9832=ORIENTED_EDGE('',*,*,#6628,.F.);
#9833=ORIENTED_EDGE('',*,*,#6630,.T.);
#9834=ORIENTED_EDGE('',*,*,#6631,.T.);
#9835=ORIENTED_EDGE('',*,*,#6632,.F.);
#9836=ORIENTED_EDGE('',*,*,#6631,.F.);
#9837=ORIENTED_EDGE('',*,*,#6633,.T.);
#9838=ORIENTED_EDGE('',*,*,#6634,.T.);
#9839=ORIENTED_EDGE('',*,*,#6635,.F.);
#9840=ORIENTED_EDGE('',*,*,#6634,.F.);
#9841=ORIENTED_EDGE('',*,*,#6636,.T.);
#9842=ORIENTED_EDGE('',*,*,#6637,.T.);
#9843=ORIENTED_EDGE('',*,*,#6638,.F.);
#9844=ORIENTED_EDGE('',*,*,#6637,.F.);
#9845=ORIENTED_EDGE('',*,*,#6639,.T.);
#9846=ORIENTED_EDGE('',*,*,#6640,.T.);
#9847=ORIENTED_EDGE('',*,*,#6641,.F.);
#9848=ORIENTED_EDGE('',*,*,#6640,.F.);
#9849=ORIENTED_EDGE('',*,*,#6642,.T.);
#9850=ORIENTED_EDGE('',*,*,#6643,.T.);
#9851=ORIENTED_EDGE('',*,*,#6644,.F.);
#9852=ORIENTED_EDGE('',*,*,#6643,.F.);
#9853=ORIENTED_EDGE('',*,*,#6644,.T.);
#9854=ORIENTED_EDGE('',*,*,#6639,.F.);
#9855=ORIENTED_EDGE('',*,*,#6633,.F.);
#9856=ORIENTED_EDGE('',*,*,#6627,.F.);
#9857=ORIENTED_EDGE('',*,*,#6621,.F.);
#9858=ORIENTED_EDGE('',*,*,#6624,.F.);
#9859=ORIENTED_EDGE('',*,*,#6630,.F.);
#9860=ORIENTED_EDGE('',*,*,#6636,.F.);
#9861=ORIENTED_EDGE('',*,*,#6642,.F.);
#9862=ORIENTED_EDGE('',*,*,#6641,.T.);
#9863=ORIENTED_EDGE('',*,*,#6638,.T.);
#9864=ORIENTED_EDGE('',*,*,#6635,.T.);
#9865=ORIENTED_EDGE('',*,*,#6632,.T.);
#9866=ORIENTED_EDGE('',*,*,#6629,.T.);
#9867=ORIENTED_EDGE('',*,*,#6626,.T.);
#9868=ORIENTED_EDGE('',*,*,#6623,.T.);
#9869=ORIENTED_EDGE('',*,*,#6645,.F.);
#9870=ORIENTED_EDGE('',*,*,#6646,.T.);
#9871=ORIENTED_EDGE('',*,*,#6647,.F.);
#9872=ORIENTED_EDGE('',*,*,#6646,.F.);
#9873=ORIENTED_EDGE('',*,*,#6648,.F.);
#9874=ORIENTED_EDGE('',*,*,#6649,.T.);
#9875=ORIENTED_EDGE('',*,*,#6650,.F.);
#9876=ORIENTED_EDGE('',*,*,#6651,.F.);
#9877=ORIENTED_EDGE('',*,*,#6649,.F.);
#9878=ORIENTED_EDGE('',*,*,#6652,.T.);
#9879=ORIENTED_EDGE('',*,*,#6653,.T.);
#9880=ORIENTED_EDGE('',*,*,#6650,.T.);
#9881=ORIENTED_EDGE('',*,*,#6651,.T.);
#9882=ORIENTED_EDGE('',*,*,#6653,.F.);
#9883=ORIENTED_EDGE('',*,*,#6654,.T.);
#9884=ORIENTED_EDGE('',*,*,#6655,.T.);
#9885=ORIENTED_EDGE('',*,*,#6645,.T.);
#9886=ORIENTED_EDGE('',*,*,#6655,.F.);
#9887=ORIENTED_EDGE('',*,*,#6647,.T.);
#9888=ORIENTED_EDGE('',*,*,#6648,.T.);
#9889=ORIENTED_EDGE('',*,*,#6652,.F.);
#9890=ORIENTED_EDGE('',*,*,#6654,.F.);
#9891=ORIENTED_EDGE('',*,*,#6656,.T.);
#9892=ORIENTED_EDGE('',*,*,#6657,.T.);
#9893=ORIENTED_EDGE('',*,*,#6658,.F.);
#9894=ORIENTED_EDGE('',*,*,#6657,.F.);
#9895=ORIENTED_EDGE('',*,*,#6659,.F.);
#9896=ORIENTED_EDGE('',*,*,#6660,.F.);
#9897=ORIENTED_EDGE('',*,*,#6661,.T.);
#9898=ORIENTED_EDGE('',*,*,#6662,.T.);
#9899=ORIENTED_EDGE('',*,*,#6663,.F.);
#9900=ORIENTED_EDGE('',*,*,#6664,.F.);
#9901=ORIENTED_EDGE('',*,*,#6665,.T.);
#9902=ORIENTED_EDGE('',*,*,#6660,.T.);
#9903=ORIENTED_EDGE('',*,*,#6666,.F.);
#9904=ORIENTED_EDGE('',*,*,#6667,.F.);
#9905=ORIENTED_EDGE('',*,*,#6668,.T.);
#9906=ORIENTED_EDGE('',*,*,#6664,.T.);
#9907=ORIENTED_EDGE('',*,*,#6669,.F.);
#9908=ORIENTED_EDGE('',*,*,#6670,.F.);
#9909=ORIENTED_EDGE('',*,*,#6671,.T.);
#9910=ORIENTED_EDGE('',*,*,#6667,.T.);
#9911=ORIENTED_EDGE('',*,*,#6672,.F.);
#9912=ORIENTED_EDGE('',*,*,#6673,.F.);
#9913=ORIENTED_EDGE('',*,*,#6674,.T.);
#9914=ORIENTED_EDGE('',*,*,#6670,.T.);
#9915=ORIENTED_EDGE('',*,*,#6675,.F.);
#9916=ORIENTED_EDGE('',*,*,#6662,.F.);
#9917=ORIENTED_EDGE('',*,*,#6676,.T.);
#9918=ORIENTED_EDGE('',*,*,#6673,.T.);
#9919=ORIENTED_EDGE('',*,*,#6661,.F.);
#9920=ORIENTED_EDGE('',*,*,#6665,.F.);
#9921=ORIENTED_EDGE('',*,*,#6668,.F.);
#9922=ORIENTED_EDGE('',*,*,#6671,.F.);
#9923=ORIENTED_EDGE('',*,*,#6674,.F.);
#9924=ORIENTED_EDGE('',*,*,#6676,.F.);
#9925=ORIENTED_EDGE('',*,*,#6656,.F.);
#9926=ORIENTED_EDGE('',*,*,#6659,.T.);
#9927=ORIENTED_EDGE('',*,*,#6675,.T.);
#9928=ORIENTED_EDGE('',*,*,#6672,.T.);
#9929=ORIENTED_EDGE('',*,*,#6669,.T.);
#9930=ORIENTED_EDGE('',*,*,#6666,.T.);
#9931=ORIENTED_EDGE('',*,*,#6663,.T.);
#9932=ORIENTED_EDGE('',*,*,#6658,.T.);
#9933=ORIENTED_EDGE('',*,*,#6677,.T.);
#9934=ORIENTED_EDGE('',*,*,#6678,.T.);
#9935=ORIENTED_EDGE('',*,*,#6679,.F.);
#9936=ORIENTED_EDGE('',*,*,#6680,.T.);
#9937=ORIENTED_EDGE('',*,*,#6681,.F.);
#9938=ORIENTED_EDGE('',*,*,#6682,.T.);
#9939=ORIENTED_EDGE('',*,*,#6683,.T.);
#9940=ORIENTED_EDGE('',*,*,#6684,.T.);
#9941=ORIENTED_EDGE('',*,*,#6685,.F.);
#9942=ORIENTED_EDGE('',*,*,#6686,.T.);
#9943=ORIENTED_EDGE('',*,*,#6687,.T.);
#9944=ORIENTED_EDGE('',*,*,#6688,.T.);
#9945=ORIENTED_EDGE('',*,*,#6689,.T.);
#9946=ORIENTED_EDGE('',*,*,#6690,.T.);
#9947=ORIENTED_EDGE('',*,*,#6691,.F.);
#9948=ORIENTED_EDGE('',*,*,#6692,.F.);
#9949=ORIENTED_EDGE('',*,*,#6693,.F.);
#9950=ORIENTED_EDGE('',*,*,#6694,.F.);
#9951=ORIENTED_EDGE('',*,*,#6695,.T.);
#9952=ORIENTED_EDGE('',*,*,#6692,.T.);
#9953=ORIENTED_EDGE('',*,*,#6696,.F.);
#9954=ORIENTED_EDGE('',*,*,#6697,.T.);
#9955=ORIENTED_EDGE('',*,*,#6698,.T.);
#9956=ORIENTED_EDGE('',*,*,#6694,.T.);
#9957=ORIENTED_EDGE('',*,*,#6699,.T.);
#9958=ORIENTED_EDGE('',*,*,#6700,.T.);
#9959=ORIENTED_EDGE('',*,*,#6701,.F.);
#9960=ORIENTED_EDGE('',*,*,#6702,.T.);
#9961=ORIENTED_EDGE('',*,*,#6703,.T.);
#9962=ORIENTED_EDGE('',*,*,#6704,.T.);
#9963=ORIENTED_EDGE('',*,*,#6705,.F.);
#9964=ORIENTED_EDGE('',*,*,#6706,.T.);
#9965=ORIENTED_EDGE('',*,*,#6687,.F.);
#9966=ORIENTED_EDGE('',*,*,#6707,.T.);
#9967=ORIENTED_EDGE('',*,*,#6689,.F.);
#9968=ORIENTED_EDGE('',*,*,#6695,.F.);
#9969=ORIENTED_EDGE('',*,*,#6698,.F.);
#9970=ORIENTED_EDGE('',*,*,#6708,.T.);
#9971=ORIENTED_EDGE('',*,*,#6699,.F.);
#9972=ORIENTED_EDGE('',*,*,#6709,.T.);
#9973=ORIENTED_EDGE('',*,*,#6703,.F.);
#9974=ORIENTED_EDGE('',*,*,#6710,.T.);
#9975=ORIENTED_EDGE('',*,*,#6677,.F.);
#9976=ORIENTED_EDGE('',*,*,#6711,.T.);
#9977=ORIENTED_EDGE('',*,*,#6683,.F.);
#9978=ORIENTED_EDGE('',*,*,#6712,.T.);
#9979=ORIENTED_EDGE('',*,*,#6691,.T.);
#9980=ORIENTED_EDGE('',*,*,#6713,.T.);
#9981=ORIENTED_EDGE('',*,*,#6685,.T.);
#9982=ORIENTED_EDGE('',*,*,#6714,.T.);
#9983=ORIENTED_EDGE('',*,*,#6681,.T.);
#9984=ORIENTED_EDGE('',*,*,#6715,.T.);
#9985=ORIENTED_EDGE('',*,*,#6679,.T.);
#9986=ORIENTED_EDGE('',*,*,#6716,.T.);
#9987=ORIENTED_EDGE('',*,*,#6705,.T.);
#9988=ORIENTED_EDGE('',*,*,#6717,.T.);
#9989=ORIENTED_EDGE('',*,*,#6701,.T.);
#9990=ORIENTED_EDGE('',*,*,#6718,.T.);
#9991=ORIENTED_EDGE('',*,*,#6696,.T.);
#9992=ORIENTED_EDGE('',*,*,#6693,.T.);
#9993=ORIENTED_EDGE('',*,*,#6707,.F.);
#9994=ORIENTED_EDGE('',*,*,#6686,.F.);
#9995=ORIENTED_EDGE('',*,*,#6713,.F.);
#9996=ORIENTED_EDGE('',*,*,#6690,.F.);
#9997=ORIENTED_EDGE('',*,*,#6712,.F.);
#9998=ORIENTED_EDGE('',*,*,#6682,.F.);
#9999=ORIENTED_EDGE('',*,*,#6714,.F.);
#10000=ORIENTED_EDGE('',*,*,#6688,.F.);
#10001=ORIENTED_EDGE('',*,*,#6708,.F.);
#10002=ORIENTED_EDGE('',*,*,#6697,.F.);
#10003=ORIENTED_EDGE('',*,*,#6718,.F.);
#10004=ORIENTED_EDGE('',*,*,#6700,.F.);
#10005=ORIENTED_EDGE('',*,*,#6709,.F.);
#10006=ORIENTED_EDGE('',*,*,#6702,.F.);
#10007=ORIENTED_EDGE('',*,*,#6717,.F.);
#10008=ORIENTED_EDGE('',*,*,#6704,.F.);
#10009=ORIENTED_EDGE('',*,*,#6710,.F.);
#10010=ORIENTED_EDGE('',*,*,#6706,.F.);
#10011=ORIENTED_EDGE('',*,*,#6716,.F.);
#10012=ORIENTED_EDGE('',*,*,#6678,.F.);
#10013=ORIENTED_EDGE('',*,*,#6711,.F.);
#10014=ORIENTED_EDGE('',*,*,#6680,.F.);
#10015=ORIENTED_EDGE('',*,*,#6715,.F.);
#10016=ORIENTED_EDGE('',*,*,#6684,.F.);
#10017=ORIENTED_EDGE('',*,*,#6719,.F.);
#10018=ORIENTED_EDGE('',*,*,#6720,.T.);
#10019=ORIENTED_EDGE('',*,*,#6721,.T.);
#10020=ORIENTED_EDGE('',*,*,#6720,.F.);
#10021=ORIENTED_EDGE('',*,*,#6722,.F.);
#10022=ORIENTED_EDGE('',*,*,#6723,.T.);
#10023=ORIENTED_EDGE('',*,*,#6724,.T.);
#10024=ORIENTED_EDGE('',*,*,#6723,.F.);
#10025=ORIENTED_EDGE('',*,*,#6722,.T.);
#10026=ORIENTED_EDGE('',*,*,#6721,.F.);
#10027=ORIENTED_EDGE('',*,*,#6724,.F.);
#10028=ORIENTED_EDGE('',*,*,#6719,.T.);
#10029=CYLINDRICAL_SURFACE('',#10966,2.5);
#10030=CYLINDRICAL_SURFACE('',#10969,2.5);
#10031=CYLINDRICAL_SURFACE('',#10972,2.5);
#10032=CYLINDRICAL_SURFACE('',#10975,2.5);
#10033=CYLINDRICAL_SURFACE('',#10978,3.);
#10034=CYLINDRICAL_SURFACE('',#10981,2.99999999999999);
#10035=CYLINDRICAL_SURFACE('',#10984,3.);
#10036=CYLINDRICAL_SURFACE('',#10987,3.);
#10037=CYLINDRICAL_SURFACE('',#10990,3.);
#10038=CYLINDRICAL_SURFACE('',#10993,3.);
#10039=CYLINDRICAL_SURFACE('',#10996,17.5);
#10040=CYLINDRICAL_SURFACE('',#11027,17.5);
#10041=CYLINDRICAL_SURFACE('',#11028,2.50000000000001);
#10042=CYLINDRICAL_SURFACE('',#11029,2.5);
#10043=CYLINDRICAL_SURFACE('',#11030,17.5);
#10044=CYLINDRICAL_SURFACE('',#11031,2.50000000000001);
#10045=CYLINDRICAL_SURFACE('',#11032,2.5);
#10046=CYLINDRICAL_SURFACE('',#11033,3.);
#10047=CYLINDRICAL_SURFACE('',#11036,3.);
#10048=CYLINDRICAL_SURFACE('',#11038,3.);
#10049=CYLINDRICAL_SURFACE('',#11040,3.);
#10050=CYLINDRICAL_SURFACE('',#11042,9.49999999999999);
#10051=CYLINDRICAL_SURFACE('',#11044,9.49999999999999);
#10052=CYLINDRICAL_SURFACE('',#11045,9.49999999999999);
#10053=CYLINDRICAL_SURFACE('',#11046,9.49999999999999);
#10054=CYLINDRICAL_SURFACE('',#11047,9.49999999999999);
#10055=CYLINDRICAL_SURFACE('',#11048,9.49999999999999);
#10056=CYLINDRICAL_SURFACE('',#11049,9.49999999999999);
#10057=CYLINDRICAL_SURFACE('',#11055,7.49999999999999);
#10058=CYLINDRICAL_SURFACE('',#11060,7.99999999999999);
#10059=CYLINDRICAL_SURFACE('',#11063,7.5);
#10060=CYLINDRICAL_SURFACE('',#11065,9.49999999999999);
#10061=CYLINDRICAL_SURFACE('',#11085,7.5);
#10062=CYLINDRICAL_SURFACE('',#11088,15.);
#10063=CYLINDRICAL_SURFACE('',#11091,7.45);
#10064=CYLINDRICAL_SURFACE('',#11093,6.25);
#10065=CYLINDRICAL_SURFACE('',#11289,15.);
#10066=CYLINDRICAL_SURFACE('',#11338,43.5);
#10067=CYLINDRICAL_SURFACE('',#11339,43.5);
#10068=CYLINDRICAL_SURFACE('',#11340,43.5);
#10069=CYLINDRICAL_SURFACE('',#11341,43.5);
#10070=CYLINDRICAL_SURFACE('',#11342,43.5);
#10071=CYLINDRICAL_SURFACE('',#11343,43.5);
#10072=CYLINDRICAL_SURFACE('',#11344,43.5);
#10073=CYLINDRICAL_SURFACE('',#11345,43.5);
#10074=CYLINDRICAL_SURFACE('',#11346,43.5);
#10075=CYLINDRICAL_SURFACE('',#11347,43.5);
#10076=CYLINDRICAL_SURFACE('',#11348,43.5);
#10077=CYLINDRICAL_SURFACE('',#11349,43.5);
#10078=CYLINDRICAL_SURFACE('',#11350,43.5);
#10079=CYLINDRICAL_SURFACE('',#11351,43.5);
#10080=CYLINDRICAL_SURFACE('',#11352,43.5);
#10081=CYLINDRICAL_SURFACE('',#11353,43.5);
#10082=CYLINDRICAL_SURFACE('',#11354,43.5);
#10083=CYLINDRICAL_SURFACE('',#11355,43.5);
#10084=CYLINDRICAL_SURFACE('',#11356,43.5);
#10085=CYLINDRICAL_SURFACE('',#11357,43.5);
#10086=CYLINDRICAL_SURFACE('',#11358,43.5);
#10087=CYLINDRICAL_SURFACE('',#11359,43.5);
#10088=CYLINDRICAL_SURFACE('',#11360,43.5);
#10089=CYLINDRICAL_SURFACE('',#11361,43.5);
#10090=CYLINDRICAL_SURFACE('',#11362,43.5);
#10091=CYLINDRICAL_SURFACE('',#11363,43.5);
#10092=CYLINDRICAL_SURFACE('',#11364,43.5);
#10093=CYLINDRICAL_SURFACE('',#11365,43.5);
#10094=CYLINDRICAL_SURFACE('',#11366,43.5);
#10095=CYLINDRICAL_SURFACE('',#11367,43.5);
#10096=CYLINDRICAL_SURFACE('',#11368,43.5);
#10097=CYLINDRICAL_SURFACE('',#11369,43.5);
#10098=CYLINDRICAL_SURFACE('',#11370,43.5);
#10099=CYLINDRICAL_SURFACE('',#11371,43.5);
#10100=CYLINDRICAL_SURFACE('',#11372,43.5);
#10101=CYLINDRICAL_SURFACE('',#11373,43.5);
#10102=CYLINDRICAL_SURFACE('',#11374,43.5);
#10103=CYLINDRICAL_SURFACE('',#11375,43.5);
#10104=CYLINDRICAL_SURFACE('',#11376,43.5);
#10105=CYLINDRICAL_SURFACE('',#11377,43.5);
#10106=CYLINDRICAL_SURFACE('',#11378,43.5);
#10107=CYLINDRICAL_SURFACE('',#11379,43.5);
#10108=CYLINDRICAL_SURFACE('',#11380,43.5);
#10109=CYLINDRICAL_SURFACE('',#11381,43.5);
#10110=CYLINDRICAL_SURFACE('',#11382,43.5);
#10111=CYLINDRICAL_SURFACE('',#11383,43.5);
#10112=CYLINDRICAL_SURFACE('',#11384,43.5);
#10113=CYLINDRICAL_SURFACE('',#11385,43.5);
#10114=CYLINDRICAL_SURFACE('',#11386,43.5);
#10115=CYLINDRICAL_SURFACE('',#11387,43.5);
#10116=CYLINDRICAL_SURFACE('',#11388,43.5);
#10117=CYLINDRICAL_SURFACE('',#11389,43.5);
#10118=CYLINDRICAL_SURFACE('',#11390,43.5);
#10119=CYLINDRICAL_SURFACE('',#11391,43.5);
#10120=CYLINDRICAL_SURFACE('',#11392,43.5);
#10121=CYLINDRICAL_SURFACE('',#11393,43.5);
#10122=CYLINDRICAL_SURFACE('',#11394,43.5);
#10123=CYLINDRICAL_SURFACE('',#11395,43.5);
#10124=CYLINDRICAL_SURFACE('',#11396,43.5);
#10125=CYLINDRICAL_SURFACE('',#11397,43.5);
#10126=CYLINDRICAL_SURFACE('',#11398,43.5);
#10127=CYLINDRICAL_SURFACE('',#11399,43.5);
#10128=CYLINDRICAL_SURFACE('',#11400,43.5);
#10129=CYLINDRICAL_SURFACE('',#11401,43.5);
#10130=CYLINDRICAL_SURFACE('',#11402,43.5);
#10131=CYLINDRICAL_SURFACE('',#11403,43.5);
#10132=CYLINDRICAL_SURFACE('',#11404,43.5);
#10133=CYLINDRICAL_SURFACE('',#11405,43.5);
#10134=CYLINDRICAL_SURFACE('',#11406,43.5);
#10135=CYLINDRICAL_SURFACE('',#11407,43.5);
#10136=CYLINDRICAL_SURFACE('',#11408,43.5);
#10137=CYLINDRICAL_SURFACE('',#11409,43.5);
#10138=CYLINDRICAL_SURFACE('',#11410,43.5);
#10139=CYLINDRICAL_SURFACE('',#11411,43.5);
#10140=CYLINDRICAL_SURFACE('',#11412,43.5);
#10141=CYLINDRICAL_SURFACE('',#11413,43.5);
#10142=CYLINDRICAL_SURFACE('',#11414,43.5);
#10143=CYLINDRICAL_SURFACE('',#11415,43.5);
#10144=CYLINDRICAL_SURFACE('',#11416,43.5);
#10145=CYLINDRICAL_SURFACE('',#11417,43.5);
#10146=CYLINDRICAL_SURFACE('',#11418,43.5);
#10147=CYLINDRICAL_SURFACE('',#11419,43.5);
#10148=CYLINDRICAL_SURFACE('',#11420,43.5);
#10149=CYLINDRICAL_SURFACE('',#11421,43.5);
#10150=CYLINDRICAL_SURFACE('',#11422,43.5);
#10151=CYLINDRICAL_SURFACE('',#11423,43.5);
#10152=CYLINDRICAL_SURFACE('',#11424,43.5);
#10153=CYLINDRICAL_SURFACE('',#11425,43.5);
#10154=CYLINDRICAL_SURFACE('',#11608,4.);
#10155=CYLINDRICAL_SURFACE('',#11611,4.);
#10156=CYLINDRICAL_SURFACE('',#11614,2.5);
#10157=CYLINDRICAL_SURFACE('',#11617,2.5);
#10158=CYLINDRICAL_SURFACE('',#11620,2.5);
#10159=CYLINDRICAL_SURFACE('',#11623,2.5);
#10160=CYLINDRICAL_SURFACE('',#11626,3.);
#10161=CYLINDRICAL_SURFACE('',#11629,2.99999999999999);
#10162=CYLINDRICAL_SURFACE('',#11632,3.);
#10163=CYLINDRICAL_SURFACE('',#11635,3.);
#10164=CYLINDRICAL_SURFACE('',#11638,3.);
#10165=CYLINDRICAL_SURFACE('',#11641,3.);
#10166=CYLINDRICAL_SURFACE('',#11644,17.5);
#10167=CYLINDRICAL_SURFACE('',#11675,17.5);
#10168=CYLINDRICAL_SURFACE('',#11676,2.50000000000001);
#10169=CYLINDRICAL_SURFACE('',#11677,2.5);
#10170=CYLINDRICAL_SURFACE('',#11678,17.5);
#10171=CYLINDRICAL_SURFACE('',#11679,2.50000000000001);
#10172=CYLINDRICAL_SURFACE('',#11680,2.5);
#10173=CYLINDRICAL_SURFACE('',#11681,3.);
#10174=CYLINDRICAL_SURFACE('',#11684,3.);
#10175=CYLINDRICAL_SURFACE('',#11686,3.);
#10176=CYLINDRICAL_SURFACE('',#11688,3.);
#10177=CYLINDRICAL_SURFACE('',#11696,0.5);
#10178=CYLINDRICAL_SURFACE('',#11705,0.5);
#10179=CYLINDRICAL_SURFACE('',#11707,0.5);
#10180=CYLINDRICAL_SURFACE('',#11709,0.5);
#10181=CYLINDRICAL_SURFACE('',#11712,0.5);
#10182=CYLINDRICAL_SURFACE('',#11714,0.5);
#10183=CYLINDRICAL_SURFACE('',#11716,0.5);
#10184=CYLINDRICAL_SURFACE('',#11727,0.5);
#10185=CYLINDRICAL_SURFACE('',#11729,0.5);
#10186=CYLINDRICAL_SURFACE('',#11731,0.5);
#10187=CYLINDRICAL_SURFACE('',#11733,0.5);
#10188=CYLINDRICAL_SURFACE('',#11739,0.5);
#10189=CYLINDRICAL_SURFACE('',#11741,3.);
#10190=CYLINDRICAL_SURFACE('',#11744,3.);
#10191=CYLINDRICAL_SURFACE('',#11747,3.);
#10192=CYLINDRICAL_SURFACE('',#11750,3.00000000000001);
#10193=CYLINDRICAL_SURFACE('',#11753,3.);
#10194=CYLINDRICAL_SURFACE('',#11756,3.);
#10195=CYLINDRICAL_SURFACE('',#11759,7.6);
#10196=CYLINDRICAL_SURFACE('',#11762,30.);
#10197=CYLINDRICAL_SURFACE('',#11768,2.5);
#10198=CYLINDRICAL_SURFACE('',#11771,2.5);
#10199=CYLINDRICAL_SURFACE('',#11774,2.5);
#10200=CYLINDRICAL_SURFACE('',#11777,2.5);
#10201=CYLINDRICAL_SURFACE('',#11780,2.5);
#10202=CYLINDRICAL_SURFACE('',#11783,2.5);
#10203=CYLINDRICAL_SURFACE('',#11786,7.6);
#10204=CYLINDRICAL_SURFACE('',#11789,27.5);
#10205=CYLINDRICAL_SURFACE('',#11803,5.00000000000001);
#10206=CYLINDRICAL_SURFACE('',#11805,3.97500000000001);
#10207=CYLINDRICAL_SURFACE('',#11811,2.5);
#10208=CYLINDRICAL_SURFACE('',#11841,7.5);
#10209=CYLINDRICAL_SURFACE('',#11844,17.5);
#10210=ADVANCED_FACE('',(#1565),#10029,.F.);
#10211=ADVANCED_FACE('',(#1566),#10030,.F.);
#10212=ADVANCED_FACE('',(#1567),#10031,.F.);
#10213=ADVANCED_FACE('',(#1568),#10032,.F.);
#10214=ADVANCED_FACE('',(#1569),#10033,.F.);
#10215=ADVANCED_FACE('',(#1570),#10034,.F.);
#10216=ADVANCED_FACE('',(#1571),#10035,.F.);
#10217=ADVANCED_FACE('',(#1572),#10036,.F.);
#10218=ADVANCED_FACE('',(#1573),#10037,.F.);
#10219=ADVANCED_FACE('',(#1574),#10038,.F.);
#10220=ADVANCED_FACE('',(#1575),#10039,.F.);
#10221=ADVANCED_FACE('',(#1576),#1465,.T.);
#10222=ADVANCED_FACE('',(#1577),#1466,.T.);
#10223=ADVANCED_FACE('',(#1578),#1467,.T.);
#10224=ADVANCED_FACE('',(#1579),#1468,.T.);
#10225=ADVANCED_FACE('',(#1580),#1469,.T.);
#10226=ADVANCED_FACE('',(#1581,#1377,#1378),#1470,.F.);
#10227=ADVANCED_FACE('',(#1582),#1471,.T.);
#10228=ADVANCED_FACE('',(#1583,#1379,#1380),#1472,.F.);
#10229=ADVANCED_FACE('',(#1584),#1473,.F.);
#10230=ADVANCED_FACE('',(#1585),#1474,.F.);
#10231=ADVANCED_FACE('',(#1586,#1381,#1382),#1475,.T.);
#10232=ADVANCED_FACE('',(#1587),#1476,.T.);
#10233=ADVANCED_FACE('',(#1588,#1383,#1384),#1477,.T.);
#10234=ADVANCED_FACE('',(#1589),#1478,.T.);
#10235=ADVANCED_FACE('',(#1590,#1385,#1386,#1387,#1388,#1389,#1390,#1391),
#1479,.F.);
#10236=ADVANCED_FACE('',(#1591,#1392,#1393,#1394,#1395,#1396,#1397,#1398),
#1480,.T.);
#10237=ADVANCED_FACE('',(#1592),#10040,.F.);
#10238=ADVANCED_FACE('',(#1593),#10041,.F.);
#10239=ADVANCED_FACE('',(#1594),#10042,.F.);
#10240=ADVANCED_FACE('',(#1595),#10043,.F.);
#10241=ADVANCED_FACE('',(#1596),#10044,.F.);
#10242=ADVANCED_FACE('',(#1597),#10045,.F.);
#10243=ADVANCED_FACE('',(#1598),#10046,.T.);
#10244=ADVANCED_FACE('',(#1599),#10047,.T.);
#10245=ADVANCED_FACE('',(#1600),#10048,.T.);
#10246=ADVANCED_FACE('',(#1601),#10049,.T.);
#10247=ADVANCED_FACE('',(#1602),#10050,.T.);
#10248=ADVANCED_FACE('',(#1603),#10051,.T.);
#10249=ADVANCED_FACE('',(#1604),#10052,.T.);
#10250=ADVANCED_FACE('',(#1605),#10053,.T.);
#10251=ADVANCED_FACE('',(#1606),#10054,.T.);
#10252=ADVANCED_FACE('',(#1607),#10055,.T.);
#10253=ADVANCED_FACE('',(#1608),#10056,.T.);
#10254=ADVANCED_FACE('',(#1609),#592,.T.);
#10255=ADVANCED_FACE('',(#1610),#10057,.T.);
#10256=ADVANCED_FACE('',(#1611),#10058,.T.);
#10257=ADVANCED_FACE('',(#1612),#10059,.T.);
#10258=ADVANCED_FACE('',(#1613),#10060,.T.);
#10259=ADVANCED_FACE('',(#1614,#1399),#1481,.T.);
#10260=ADVANCED_FACE('',(#1615,#1400),#1482,.T.);
#10261=ADVANCED_FACE('',(#1616,#1401),#1483,.T.);
#10262=ADVANCED_FACE('',(#1617),#1484,.T.);
#10263=ADVANCED_FACE('',(#1618),#322,.F.);
#10264=ADVANCED_FACE('',(#1619),#323,.F.);
#10265=ADVANCED_FACE('',(#1620),#324,.F.);
#10266=ADVANCED_FACE('',(#1621),#1485,.F.);
#10267=ADVANCED_FACE('',(#1622),#325,.T.);
#10268=ADVANCED_FACE('',(#1623),#326,.T.);
#10269=ADVANCED_FACE('',(#1624),#327,.T.);
#10270=ADVANCED_FACE('',(#1625),#1486,.T.);
#10271=ADVANCED_FACE('',(#1626),#1487,.F.);
#10272=ADVANCED_FACE('',(#1627),#1488,.F.);
#10273=ADVANCED_FACE('',(#1628),#1489,.F.);
#10274=ADVANCED_FACE('',(#1629),#1490,.F.);
#10275=ADVANCED_FACE('',(#1630),#1491,.T.);
#10276=ADVANCED_FACE('',(#1631),#593,.T.);
#10277=ADVANCED_FACE('',(#1632),#10061,.T.);
#10278=ADVANCED_FACE('',(#1633),#10062,.T.);
#10279=ADVANCED_FACE('',(#1634),#10063,.T.);
#10280=ADVANCED_FACE('',(#1635),#10064,.T.);
#10281=ADVANCED_FACE('',(#1636),#1492,.T.);
#10282=ADVANCED_FACE('',(#1637),#1493,.T.);
#10283=ADVANCED_FACE('',(#1638),#1494,.F.);
#10284=ADVANCED_FACE('',(#1639),#1495,.T.);
#10285=ADVANCED_FACE('',(#1640),#1496,.T.);
#10286=ADVANCED_FACE('',(#1641,#1402),#1497,.T.);
#10287=ADVANCED_FACE('',(#1642,#1403),#1498,.F.);
#10288=ADVANCED_FACE('',(#1643,#1404),#1499,.T.);
#10289=ADVANCED_FACE('',(#1644),#1500,.T.);
#10290=ADVANCED_FACE('',(#1645),#1501,.T.);
#10291=ADVANCED_FACE('',(#1646),#1502,.F.);
#10292=ADVANCED_FACE('',(#1647),#1503,.F.);
#10293=ADVANCED_FACE('',(#1648),#183,.F.);
#10294=ADVANCED_FACE('',(#1649),#184,.F.);
#10295=ADVANCED_FACE('',(#1650),#185,.F.);
#10296=ADVANCED_FACE('',(#1651),#186,.F.);
#10297=ADVANCED_FACE('',(#1652),#187,.F.);
#10298=ADVANCED_FACE('',(#1653),#188,.F.);
#10299=ADVANCED_FACE('',(#1654),#189,.F.);
#10300=ADVANCED_FACE('',(#1655),#190,.F.);
#10301=ADVANCED_FACE('',(#1656),#191,.F.);
#10302=ADVANCED_FACE('',(#1657),#192,.F.);
#10303=ADVANCED_FACE('',(#1658),#193,.F.);
#10304=ADVANCED_FACE('',(#1659),#194,.F.);
#10305=ADVANCED_FACE('',(#1660),#195,.F.);
#10306=ADVANCED_FACE('',(#1661),#196,.F.);
#10307=ADVANCED_FACE('',(#1662),#197,.F.);
#10308=ADVANCED_FACE('',(#1663),#198,.F.);
#10309=ADVANCED_FACE('',(#1664),#199,.F.);
#10310=ADVANCED_FACE('',(#1665),#200,.F.);
#10311=ADVANCED_FACE('',(#1666),#201,.F.);
#10312=ADVANCED_FACE('',(#1667),#202,.F.);
#10313=ADVANCED_FACE('',(#1668),#203,.F.);
#10314=ADVANCED_FACE('',(#1669),#204,.F.);
#10315=ADVANCED_FACE('',(#1670),#205,.F.);
#10316=ADVANCED_FACE('',(#1671),#206,.F.);
#10317=ADVANCED_FACE('',(#1672),#207,.F.);
#10318=ADVANCED_FACE('',(#1673),#208,.F.);
#10319=ADVANCED_FACE('',(#1674),#209,.F.);
#10320=ADVANCED_FACE('',(#1675),#210,.F.);
#10321=ADVANCED_FACE('',(#1676),#211,.F.);
#10322=ADVANCED_FACE('',(#1677),#212,.F.);
#10323=ADVANCED_FACE('',(#1678),#213,.F.);
#10324=ADVANCED_FACE('',(#1679),#214,.F.);
#10325=ADVANCED_FACE('',(#1680),#215,.F.);
#10326=ADVANCED_FACE('',(#1681),#216,.F.);
#10327=ADVANCED_FACE('',(#1682),#217,.F.);
#10328=ADVANCED_FACE('',(#1683),#218,.F.);
#10329=ADVANCED_FACE('',(#1684),#219,.F.);
#10330=ADVANCED_FACE('',(#1685),#220,.F.);
#10331=ADVANCED_FACE('',(#1686),#221,.F.);
#10332=ADVANCED_FACE('',(#1687),#222,.F.);
#10333=ADVANCED_FACE('',(#1688),#223,.F.);
#10334=ADVANCED_FACE('',(#1689),#224,.F.);
#10335=ADVANCED_FACE('',(#1690),#225,.F.);
#10336=ADVANCED_FACE('',(#1691),#226,.F.);
#10337=ADVANCED_FACE('',(#1692),#594,.T.);
#10338=ADVANCED_FACE('',(#1693),#10065,.F.);
#10339=ADVANCED_FACE('',(#1694),#595,.T.);
#10340=ADVANCED_FACE('',(#1695),#10066,.T.);
#10341=ADVANCED_FACE('',(#1696),#10067,.T.);
#10342=ADVANCED_FACE('',(#1697),#10068,.T.);
#10343=ADVANCED_FACE('',(#1698),#10069,.T.);
#10344=ADVANCED_FACE('',(#1699),#10070,.T.);
#10345=ADVANCED_FACE('',(#1700),#10071,.T.);
#10346=ADVANCED_FACE('',(#1701),#10072,.T.);
#10347=ADVANCED_FACE('',(#1702),#10073,.T.);
#10348=ADVANCED_FACE('',(#1703),#10074,.T.);
#10349=ADVANCED_FACE('',(#1704),#10075,.T.);
#10350=ADVANCED_FACE('',(#1705),#10076,.T.);
#10351=ADVANCED_FACE('',(#1706),#10077,.T.);
#10352=ADVANCED_FACE('',(#1707),#10078,.T.);
#10353=ADVANCED_FACE('',(#1708),#10079,.T.);
#10354=ADVANCED_FACE('',(#1709),#10080,.T.);
#10355=ADVANCED_FACE('',(#1710),#10081,.T.);
#10356=ADVANCED_FACE('',(#1711),#10082,.T.);
#10357=ADVANCED_FACE('',(#1712),#10083,.T.);
#10358=ADVANCED_FACE('',(#1713),#10084,.T.);
#10359=ADVANCED_FACE('',(#1714),#10085,.T.);
#10360=ADVANCED_FACE('',(#1715),#10086,.T.);
#10361=ADVANCED_FACE('',(#1716),#10087,.T.);
#10362=ADVANCED_FACE('',(#1717),#10088,.T.);
#10363=ADVANCED_FACE('',(#1718),#10089,.T.);
#10364=ADVANCED_FACE('',(#1719),#10090,.T.);
#10365=ADVANCED_FACE('',(#1720),#10091,.T.);
#10366=ADVANCED_FACE('',(#1721),#10092,.T.);
#10367=ADVANCED_FACE('',(#1722),#10093,.T.);
#10368=ADVANCED_FACE('',(#1723),#10094,.T.);
#10369=ADVANCED_FACE('',(#1724),#10095,.T.);
#10370=ADVANCED_FACE('',(#1725),#10096,.T.);
#10371=ADVANCED_FACE('',(#1726),#10097,.T.);
#10372=ADVANCED_FACE('',(#1727),#10098,.T.);
#10373=ADVANCED_FACE('',(#1728),#10099,.T.);
#10374=ADVANCED_FACE('',(#1729),#10100,.T.);
#10375=ADVANCED_FACE('',(#1730),#10101,.T.);
#10376=ADVANCED_FACE('',(#1731),#10102,.T.);
#10377=ADVANCED_FACE('',(#1732),#10103,.T.);
#10378=ADVANCED_FACE('',(#1733),#10104,.T.);
#10379=ADVANCED_FACE('',(#1734),#10105,.T.);
#10380=ADVANCED_FACE('',(#1735),#10106,.T.);
#10381=ADVANCED_FACE('',(#1736),#10107,.T.);
#10382=ADVANCED_FACE('',(#1737),#10108,.T.);
#10383=ADVANCED_FACE('',(#1738),#10109,.T.);
#10384=ADVANCED_FACE('',(#1739),#10110,.T.);
#10385=ADVANCED_FACE('',(#1740),#10111,.T.);
#10386=ADVANCED_FACE('',(#1741),#10112,.T.);
#10387=ADVANCED_FACE('',(#1742),#10113,.T.);
#10388=ADVANCED_FACE('',(#1743),#10114,.T.);
#10389=ADVANCED_FACE('',(#1744),#10115,.T.);
#10390=ADVANCED_FACE('',(#1745),#10116,.T.);
#10391=ADVANCED_FACE('',(#1746),#10117,.T.);
#10392=ADVANCED_FACE('',(#1747),#10118,.T.);
#10393=ADVANCED_FACE('',(#1748),#10119,.T.);
#10394=ADVANCED_FACE('',(#1749),#10120,.T.);
#10395=ADVANCED_FACE('',(#1750),#10121,.T.);
#10396=ADVANCED_FACE('',(#1751),#10122,.T.);
#10397=ADVANCED_FACE('',(#1752),#10123,.T.);
#10398=ADVANCED_FACE('',(#1753),#10124,.T.);
#10399=ADVANCED_FACE('',(#1754),#10125,.T.);
#10400=ADVANCED_FACE('',(#1755),#10126,.T.);
#10401=ADVANCED_FACE('',(#1756),#10127,.T.);
#10402=ADVANCED_FACE('',(#1757),#10128,.T.);
#10403=ADVANCED_FACE('',(#1758),#10129,.T.);
#10404=ADVANCED_FACE('',(#1759),#10130,.T.);
#10405=ADVANCED_FACE('',(#1760),#10131,.T.);
#10406=ADVANCED_FACE('',(#1761),#10132,.T.);
#10407=ADVANCED_FACE('',(#1762),#10133,.T.);
#10408=ADVANCED_FACE('',(#1763),#10134,.T.);
#10409=ADVANCED_FACE('',(#1764),#10135,.T.);
#10410=ADVANCED_FACE('',(#1765),#10136,.T.);
#10411=ADVANCED_FACE('',(#1766),#10137,.T.);
#10412=ADVANCED_FACE('',(#1767),#10138,.T.);
#10413=ADVANCED_FACE('',(#1768),#10139,.T.);
#10414=ADVANCED_FACE('',(#1769),#10140,.T.);
#10415=ADVANCED_FACE('',(#1770),#10141,.T.);
#10416=ADVANCED_FACE('',(#1771),#10142,.T.);
#10417=ADVANCED_FACE('',(#1772),#10143,.T.);
#10418=ADVANCED_FACE('',(#1773),#10144,.T.);
#10419=ADVANCED_FACE('',(#1774),#10145,.T.);
#10420=ADVANCED_FACE('',(#1775),#10146,.T.);
#10421=ADVANCED_FACE('',(#1776),#10147,.T.);
#10422=ADVANCED_FACE('',(#1777),#10148,.T.);
#10423=ADVANCED_FACE('',(#1778),#10149,.T.);
#10424=ADVANCED_FACE('',(#1779),#10150,.T.);
#10425=ADVANCED_FACE('',(#1780),#10151,.T.);
#10426=ADVANCED_FACE('',(#1781),#10152,.T.);
#10427=ADVANCED_FACE('',(#1782),#10153,.T.);
#10428=ADVANCED_FACE('',(#1783,#1405),#1504,.T.);
#10429=ADVANCED_FACE('',(#1784,#1406),#1505,.F.);
#10430=ADVANCED_FACE('',(#1785),#1506,.T.);
#10431=ADVANCED_FACE('',(#1786),#1507,.F.);
#10432=ADVANCED_FACE('',(#1787),#1508,.F.);
#10433=ADVANCED_FACE('',(#1788),#328,.F.);
#10434=ADVANCED_FACE('',(#1789),#329,.F.);
#10435=ADVANCED_FACE('',(#1790),#330,.F.);
#10436=ADVANCED_FACE('',(#1791),#331,.T.);
#10437=ADVANCED_FACE('',(#1792),#332,.T.);
#10438=ADVANCED_FACE('',(#1793),#333,.T.);
#10439=ADVANCED_FACE('',(#1794),#334,.F.);
#10440=ADVANCED_FACE('',(#1795),#335,.F.);
#10441=ADVANCED_FACE('',(#1796),#336,.F.);
#10442=ADVANCED_FACE('',(#1797),#337,.F.);
#10443=ADVANCED_FACE('',(#1798),#338,.F.);
#10444=ADVANCED_FACE('',(#1799),#339,.F.);
#10445=ADVANCED_FACE('',(#1800),#340,.F.);
#10446=ADVANCED_FACE('',(#1801),#341,.F.);
#10447=ADVANCED_FACE('',(#1802),#342,.F.);
#10448=ADVANCED_FACE('',(#1803),#343,.F.);
#10449=ADVANCED_FACE('',(#1804),#344,.F.);
#10450=ADVANCED_FACE('',(#1805),#345,.F.);
#10451=ADVANCED_FACE('',(#1806),#346,.F.);
#10452=ADVANCED_FACE('',(#1807),#347,.F.);
#10453=ADVANCED_FACE('',(#1808),#348,.F.);
#10454=ADVANCED_FACE('',(#1809),#349,.F.);
#10455=ADVANCED_FACE('',(#1810),#350,.F.);
#10456=ADVANCED_FACE('',(#1811),#351,.F.);
#10457=ADVANCED_FACE('',(#1812),#352,.F.);
#10458=ADVANCED_FACE('',(#1813),#353,.F.);
#10459=ADVANCED_FACE('',(#1814),#354,.F.);
#10460=ADVANCED_FACE('',(#1815),#355,.F.);
#10461=ADVANCED_FACE('',(#1816),#356,.F.);
#10462=ADVANCED_FACE('',(#1817),#357,.F.);
#10463=ADVANCED_FACE('',(#1818),#358,.F.);
#10464=ADVANCED_FACE('',(#1819),#359,.F.);
#10465=ADVANCED_FACE('',(#1820),#360,.F.);
#10466=ADVANCED_FACE('',(#1821),#361,.F.);
#10467=ADVANCED_FACE('',(#1822),#362,.F.);
#10468=ADVANCED_FACE('',(#1823),#363,.F.);
#10469=ADVANCED_FACE('',(#1824),#364,.F.);
#10470=ADVANCED_FACE('',(#1825),#365,.F.);
#10471=ADVANCED_FACE('',(#1826),#366,.F.);
#10472=ADVANCED_FACE('',(#1827),#367,.F.);
#10473=ADVANCED_FACE('',(#1828),#368,.F.);
#10474=ADVANCED_FACE('',(#1829),#369,.F.);
#10475=ADVANCED_FACE('',(#1830),#370,.F.);
#10476=ADVANCED_FACE('',(#1831),#371,.F.);
#10477=ADVANCED_FACE('',(#1832),#372,.F.);
#10478=ADVANCED_FACE('',(#1833),#373,.F.);
#10479=ADVANCED_FACE('',(#1834),#374,.F.);
#10480=ADVANCED_FACE('',(#1835),#375,.F.);
#10481=ADVANCED_FACE('',(#1836),#376,.F.);
#10482=ADVANCED_FACE('',(#1837),#377,.F.);
#10483=ADVANCED_FACE('',(#1838),#378,.F.);
#10484=ADVANCED_FACE('',(#1839),#379,.F.);
#10485=ADVANCED_FACE('',(#1840),#380,.F.);
#10486=ADVANCED_FACE('',(#1841),#381,.F.);
#10487=ADVANCED_FACE('',(#1842),#382,.F.);
#10488=ADVANCED_FACE('',(#1843),#383,.F.);
#10489=ADVANCED_FACE('',(#1844),#384,.F.);
#10490=ADVANCED_FACE('',(#1845),#385,.F.);
#10491=ADVANCED_FACE('',(#1846),#386,.F.);
#10492=ADVANCED_FACE('',(#1847),#387,.F.);
#10493=ADVANCED_FACE('',(#1848),#388,.F.);
#10494=ADVANCED_FACE('',(#1849),#389,.F.);
#10495=ADVANCED_FACE('',(#1850),#390,.F.);
#10496=ADVANCED_FACE('',(#1851),#391,.F.);
#10497=ADVANCED_FACE('',(#1852),#392,.F.);
#10498=ADVANCED_FACE('',(#1853),#393,.F.);
#10499=ADVANCED_FACE('',(#1854),#394,.F.);
#10500=ADVANCED_FACE('',(#1855),#395,.F.);
#10501=ADVANCED_FACE('',(#1856),#396,.F.);
#10502=ADVANCED_FACE('',(#1857),#397,.F.);
#10503=ADVANCED_FACE('',(#1858),#398,.F.);
#10504=ADVANCED_FACE('',(#1859),#399,.F.);
#10505=ADVANCED_FACE('',(#1860),#400,.F.);
#10506=ADVANCED_FACE('',(#1861),#401,.F.);
#10507=ADVANCED_FACE('',(#1862),#402,.F.);
#10508=ADVANCED_FACE('',(#1863),#403,.F.);
#10509=ADVANCED_FACE('',(#1864),#404,.F.);
#10510=ADVANCED_FACE('',(#1865),#405,.F.);
#10511=ADVANCED_FACE('',(#1866),#406,.F.);
#10512=ADVANCED_FACE('',(#1867),#407,.F.);
#10513=ADVANCED_FACE('',(#1868),#408,.F.);
#10514=ADVANCED_FACE('',(#1869),#409,.F.);
#10515=ADVANCED_FACE('',(#1870),#410,.F.);
#10516=ADVANCED_FACE('',(#1871),#411,.F.);
#10517=ADVANCED_FACE('',(#1872),#412,.F.);
#10518=ADVANCED_FACE('',(#1873),#413,.F.);
#10519=ADVANCED_FACE('',(#1874),#414,.F.);
#10520=ADVANCED_FACE('',(#1875),#415,.F.);
#10521=ADVANCED_FACE('',(#1876),#416,.F.);
#10522=ADVANCED_FACE('',(#1877),#417,.F.);
#10523=ADVANCED_FACE('',(#1878),#418,.F.);
#10524=ADVANCED_FACE('',(#1879),#419,.F.);
#10525=ADVANCED_FACE('',(#1880),#420,.F.);
#10526=ADVANCED_FACE('',(#1881),#421,.F.);
#10527=ADVANCED_FACE('',(#1882),#422,.F.);
#10528=ADVANCED_FACE('',(#1883),#423,.F.);
#10529=ADVANCED_FACE('',(#1884),#424,.F.);
#10530=ADVANCED_FACE('',(#1885),#425,.F.);
#10531=ADVANCED_FACE('',(#1886),#426,.F.);
#10532=ADVANCED_FACE('',(#1887),#427,.F.);
#10533=ADVANCED_FACE('',(#1888),#428,.F.);
#10534=ADVANCED_FACE('',(#1889),#429,.F.);
#10535=ADVANCED_FACE('',(#1890),#430,.F.);
#10536=ADVANCED_FACE('',(#1891),#431,.F.);
#10537=ADVANCED_FACE('',(#1892),#432,.F.);
#10538=ADVANCED_FACE('',(#1893),#433,.F.);
#10539=ADVANCED_FACE('',(#1894),#434,.F.);
#10540=ADVANCED_FACE('',(#1895),#435,.F.);
#10541=ADVANCED_FACE('',(#1896),#436,.F.);
#10542=ADVANCED_FACE('',(#1897),#437,.F.);
#10543=ADVANCED_FACE('',(#1898),#438,.F.);
#10544=ADVANCED_FACE('',(#1899),#439,.F.);
#10545=ADVANCED_FACE('',(#1900),#440,.F.);
#10546=ADVANCED_FACE('',(#1901),#441,.F.);
#10547=ADVANCED_FACE('',(#1902),#442,.F.);
#10548=ADVANCED_FACE('',(#1903),#443,.F.);
#10549=ADVANCED_FACE('',(#1904),#444,.F.);
#10550=ADVANCED_FACE('',(#1905),#445,.F.);
#10551=ADVANCED_FACE('',(#1906),#446,.F.);
#10552=ADVANCED_FACE('',(#1907),#447,.F.);
#10553=ADVANCED_FACE('',(#1908),#448,.F.);
#10554=ADVANCED_FACE('',(#1909),#449,.F.);
#10555=ADVANCED_FACE('',(#1910),#450,.F.);
#10556=ADVANCED_FACE('',(#1911),#451,.F.);
#10557=ADVANCED_FACE('',(#1912),#452,.F.);
#10558=ADVANCED_FACE('',(#1913),#453,.F.);
#10559=ADVANCED_FACE('',(#1914),#454,.F.);
#10560=ADVANCED_FACE('',(#1915),#455,.F.);
#10561=ADVANCED_FACE('',(#1916),#456,.F.);
#10562=ADVANCED_FACE('',(#1917),#457,.F.);
#10563=ADVANCED_FACE('',(#1918),#458,.F.);
#10564=ADVANCED_FACE('',(#1919),#459,.F.);
#10565=ADVANCED_FACE('',(#1920),#460,.F.);
#10566=ADVANCED_FACE('',(#1921),#461,.F.);
#10567=ADVANCED_FACE('',(#1922),#462,.F.);
#10568=ADVANCED_FACE('',(#1923),#463,.T.);
#10569=ADVANCED_FACE('',(#1924),#464,.T.);
#10570=ADVANCED_FACE('',(#1925),#465,.T.);
#10571=ADVANCED_FACE('',(#1926),#466,.T.);
#10572=ADVANCED_FACE('',(#1927),#467,.T.);
#10573=ADVANCED_FACE('',(#1928),#468,.T.);
#10574=ADVANCED_FACE('',(#1929),#469,.T.);
#10575=ADVANCED_FACE('',(#1930),#470,.T.);
#10576=ADVANCED_FACE('',(#1931),#471,.T.);
#10577=ADVANCED_FACE('',(#1932),#472,.T.);
#10578=ADVANCED_FACE('',(#1933),#473,.T.);
#10579=ADVANCED_FACE('',(#1934),#474,.T.);
#10580=ADVANCED_FACE('',(#1935),#475,.T.);
#10581=ADVANCED_FACE('',(#1936),#476,.T.);
#10582=ADVANCED_FACE('',(#1937),#477,.T.);
#10583=ADVANCED_FACE('',(#1938),#478,.T.);
#10584=ADVANCED_FACE('',(#1939),#479,.T.);
#10585=ADVANCED_FACE('',(#1940),#480,.T.);
#10586=ADVANCED_FACE('',(#1941),#481,.T.);
#10587=ADVANCED_FACE('',(#1942),#482,.T.);
#10588=ADVANCED_FACE('',(#1943),#483,.T.);
#10589=ADVANCED_FACE('',(#1944),#484,.T.);
#10590=ADVANCED_FACE('',(#1945),#485,.T.);
#10591=ADVANCED_FACE('',(#1946),#486,.T.);
#10592=ADVANCED_FACE('',(#1947),#487,.T.);
#10593=ADVANCED_FACE('',(#1948),#488,.T.);
#10594=ADVANCED_FACE('',(#1949),#489,.T.);
#10595=ADVANCED_FACE('',(#1950),#490,.T.);
#10596=ADVANCED_FACE('',(#1951),#491,.T.);
#10597=ADVANCED_FACE('',(#1952),#492,.T.);
#10598=ADVANCED_FACE('',(#1953),#493,.T.);
#10599=ADVANCED_FACE('',(#1954),#494,.T.);
#10600=ADVANCED_FACE('',(#1955),#495,.T.);
#10601=ADVANCED_FACE('',(#1956),#496,.T.);
#10602=ADVANCED_FACE('',(#1957),#497,.T.);
#10603=ADVANCED_FACE('',(#1958),#498,.T.);
#10604=ADVANCED_FACE('',(#1959),#499,.T.);
#10605=ADVANCED_FACE('',(#1960),#500,.T.);
#10606=ADVANCED_FACE('',(#1961),#501,.T.);
#10607=ADVANCED_FACE('',(#1962),#502,.T.);
#10608=ADVANCED_FACE('',(#1963),#503,.T.);
#10609=ADVANCED_FACE('',(#1964),#504,.T.);
#10610=ADVANCED_FACE('',(#1965),#505,.T.);
#10611=ADVANCED_FACE('',(#1966),#506,.T.);
#10612=ADVANCED_FACE('',(#1967),#507,.T.);
#10613=ADVANCED_FACE('',(#1968),#508,.T.);
#10614=ADVANCED_FACE('',(#1969),#509,.T.);
#10615=ADVANCED_FACE('',(#1970),#510,.T.);
#10616=ADVANCED_FACE('',(#1971),#511,.T.);
#10617=ADVANCED_FACE('',(#1972),#512,.T.);
#10618=ADVANCED_FACE('',(#1973),#513,.T.);
#10619=ADVANCED_FACE('',(#1974),#514,.T.);
#10620=ADVANCED_FACE('',(#1975),#515,.T.);
#10621=ADVANCED_FACE('',(#1976),#516,.T.);
#10622=ADVANCED_FACE('',(#1977),#517,.T.);
#10623=ADVANCED_FACE('',(#1978),#518,.T.);
#10624=ADVANCED_FACE('',(#1979),#519,.T.);
#10625=ADVANCED_FACE('',(#1980),#520,.T.);
#10626=ADVANCED_FACE('',(#1981),#521,.T.);
#10627=ADVANCED_FACE('',(#1982),#522,.T.);
#10628=ADVANCED_FACE('',(#1983),#523,.T.);
#10629=ADVANCED_FACE('',(#1984),#524,.T.);
#10630=ADVANCED_FACE('',(#1985),#525,.T.);
#10631=ADVANCED_FACE('',(#1986),#526,.T.);
#10632=ADVANCED_FACE('',(#1987),#527,.T.);
#10633=ADVANCED_FACE('',(#1988),#528,.T.);
#10634=ADVANCED_FACE('',(#1989),#529,.T.);
#10635=ADVANCED_FACE('',(#1990),#530,.T.);
#10636=ADVANCED_FACE('',(#1991),#531,.T.);
#10637=ADVANCED_FACE('',(#1992),#532,.T.);
#10638=ADVANCED_FACE('',(#1993),#533,.T.);
#10639=ADVANCED_FACE('',(#1994),#534,.T.);
#10640=ADVANCED_FACE('',(#1995),#535,.T.);
#10641=ADVANCED_FACE('',(#1996),#536,.T.);
#10642=ADVANCED_FACE('',(#1997),#537,.T.);
#10643=ADVANCED_FACE('',(#1998),#538,.T.);
#10644=ADVANCED_FACE('',(#1999),#539,.T.);
#10645=ADVANCED_FACE('',(#2000),#540,.T.);
#10646=ADVANCED_FACE('',(#2001),#541,.T.);
#10647=ADVANCED_FACE('',(#2002),#542,.T.);
#10648=ADVANCED_FACE('',(#2003),#543,.T.);
#10649=ADVANCED_FACE('',(#2004),#544,.T.);
#10650=ADVANCED_FACE('',(#2005),#545,.T.);
#10651=ADVANCED_FACE('',(#2006),#546,.T.);
#10652=ADVANCED_FACE('',(#2007),#547,.T.);
#10653=ADVANCED_FACE('',(#2008),#548,.T.);
#10654=ADVANCED_FACE('',(#2009),#549,.T.);
#10655=ADVANCED_FACE('',(#2010),#550,.T.);
#10656=ADVANCED_FACE('',(#2011),#551,.T.);
#10657=ADVANCED_FACE('',(#2012),#552,.T.);
#10658=ADVANCED_FACE('',(#2013),#553,.T.);
#10659=ADVANCED_FACE('',(#2014),#554,.T.);
#10660=ADVANCED_FACE('',(#2015),#555,.T.);
#10661=ADVANCED_FACE('',(#2016),#556,.T.);
#10662=ADVANCED_FACE('',(#2017),#557,.T.);
#10663=ADVANCED_FACE('',(#2018),#558,.T.);
#10664=ADVANCED_FACE('',(#2019),#559,.T.);
#10665=ADVANCED_FACE('',(#2020),#560,.T.);
#10666=ADVANCED_FACE('',(#2021),#561,.T.);
#10667=ADVANCED_FACE('',(#2022),#562,.T.);
#10668=ADVANCED_FACE('',(#2023),#563,.T.);
#10669=ADVANCED_FACE('',(#2024),#564,.T.);
#10670=ADVANCED_FACE('',(#2025),#565,.T.);
#10671=ADVANCED_FACE('',(#2026),#566,.T.);
#10672=ADVANCED_FACE('',(#2027),#567,.T.);
#10673=ADVANCED_FACE('',(#2028),#568,.T.);
#10674=ADVANCED_FACE('',(#2029),#569,.T.);
#10675=ADVANCED_FACE('',(#2030),#570,.T.);
#10676=ADVANCED_FACE('',(#2031),#571,.T.);
#10677=ADVANCED_FACE('',(#2032),#572,.T.);
#10678=ADVANCED_FACE('',(#2033),#573,.T.);
#10679=ADVANCED_FACE('',(#2034),#574,.T.);
#10680=ADVANCED_FACE('',(#2035),#575,.T.);
#10681=ADVANCED_FACE('',(#2036),#576,.T.);
#10682=ADVANCED_FACE('',(#2037),#577,.T.);
#10683=ADVANCED_FACE('',(#2038),#578,.T.);
#10684=ADVANCED_FACE('',(#2039),#579,.T.);
#10685=ADVANCED_FACE('',(#2040),#580,.T.);
#10686=ADVANCED_FACE('',(#2041),#581,.T.);
#10687=ADVANCED_FACE('',(#2042),#582,.T.);
#10688=ADVANCED_FACE('',(#2043),#583,.T.);
#10689=ADVANCED_FACE('',(#2044),#584,.T.);
#10690=ADVANCED_FACE('',(#2045),#585,.T.);
#10691=ADVANCED_FACE('',(#2046),#586,.T.);
#10692=ADVANCED_FACE('',(#2047),#587,.T.);
#10693=ADVANCED_FACE('',(#2048),#588,.T.);
#10694=ADVANCED_FACE('',(#2049),#589,.T.);
#10695=ADVANCED_FACE('',(#2050),#590,.T.);
#10696=ADVANCED_FACE('',(#2051),#591,.T.);
#10697=ADVANCED_FACE('',(#2052),#10154,.F.);
#10698=ADVANCED_FACE('',(#2053),#10155,.F.);
#10699=ADVANCED_FACE('',(#2054),#10156,.F.);
#10700=ADVANCED_FACE('',(#2055),#10157,.F.);
#10701=ADVANCED_FACE('',(#2056),#10158,.F.);
#10702=ADVANCED_FACE('',(#2057),#10159,.F.);
#10703=ADVANCED_FACE('',(#2058),#10160,.F.);
#10704=ADVANCED_FACE('',(#2059),#10161,.F.);
#10705=ADVANCED_FACE('',(#2060),#10162,.F.);
#10706=ADVANCED_FACE('',(#2061),#10163,.F.);
#10707=ADVANCED_FACE('',(#2062),#10164,.F.);
#10708=ADVANCED_FACE('',(#2063),#10165,.F.);
#10709=ADVANCED_FACE('',(#2064),#10166,.F.);
#10710=ADVANCED_FACE('',(#2065),#1509,.T.);
#10711=ADVANCED_FACE('',(#2066),#1510,.T.);
#10712=ADVANCED_FACE('',(#2067),#1511,.T.);
#10713=ADVANCED_FACE('',(#2068),#1512,.T.);
#10714=ADVANCED_FACE('',(#2069),#1513,.T.);
#10715=ADVANCED_FACE('',(#2070,#1407,#1408),#1514,.F.);
#10716=ADVANCED_FACE('',(#2071),#1515,.T.);
#10717=ADVANCED_FACE('',(#2072,#1409,#1410),#1516,.F.);
#10718=ADVANCED_FACE('',(#2073),#1517,.F.);
#10719=ADVANCED_FACE('',(#2074,#1411),#1518,.F.);
#10720=ADVANCED_FACE('',(#2075,#1412,#1413),#1519,.T.);
#10721=ADVANCED_FACE('',(#2076,#1414),#1520,.T.);
#10722=ADVANCED_FACE('',(#2077,#1415,#1416),#1521,.T.);
#10723=ADVANCED_FACE('',(#2078),#1522,.T.);
#10724=ADVANCED_FACE('',(#2079,#1417,#1418,#1419,#1420,#1421,#1422,#1423,
#1424),#1523,.F.);
#10725=ADVANCED_FACE('',(#2080,#1425,#1426,#1427,#1428,#1429,#1430,#1431,
#1432),#1524,.T.);
#10726=ADVANCED_FACE('',(#2081),#10167,.F.);
#10727=ADVANCED_FACE('',(#2082),#10168,.F.);
#10728=ADVANCED_FACE('',(#2083),#10169,.F.);
#10729=ADVANCED_FACE('',(#2084),#10170,.F.);
#10730=ADVANCED_FACE('',(#2085),#10171,.F.);
#10731=ADVANCED_FACE('',(#2086),#10172,.F.);
#10732=ADVANCED_FACE('',(#2087),#10173,.T.);
#10733=ADVANCED_FACE('',(#2088),#10174,.T.);
#10734=ADVANCED_FACE('',(#2089),#10175,.T.);
#10735=ADVANCED_FACE('',(#2090),#10176,.T.);
#10736=ADVANCED_FACE('',(#2091),#1525,.F.);
#10737=ADVANCED_FACE('',(#2092),#1526,.F.);
#10738=ADVANCED_FACE('',(#2093),#1527,.F.);
#10739=ADVANCED_FACE('',(#2094),#1528,.F.);
#10740=ADVANCED_FACE('',(#2095),#1529,.F.);
#10741=ADVANCED_FACE('',(#2096),#1530,.T.);
#10742=ADVANCED_FACE('',(#2097),#10177,.T.);
#10743=ADVANCED_FACE('',(#2098),#175,.T.);
#10744=ADVANCED_FACE('',(#2099),#176,.T.);
#10745=ADVANCED_FACE('',(#2100),#10178,.T.);
#10746=ADVANCED_FACE('',(#2101),#10179,.T.);
#10747=ADVANCED_FACE('',(#2102),#10180,.T.);
#10748=ADVANCED_FACE('',(#2103),#10181,.T.);
#10749=ADVANCED_FACE('',(#2104),#10182,.T.);
#10750=ADVANCED_FACE('',(#2105),#10183,.T.);
#10751=ADVANCED_FACE('',(#2106),#177,.T.);
#10752=ADVANCED_FACE('',(#2107),#178,.T.);
#10753=ADVANCED_FACE('',(#2108),#179,.T.);
#10754=ADVANCED_FACE('',(#2109),#180,.T.);
#10755=ADVANCED_FACE('',(#2110),#10184,.T.);
#10756=ADVANCED_FACE('',(#2111),#10185,.T.);
#10757=ADVANCED_FACE('',(#2112),#10186,.T.);
#10758=ADVANCED_FACE('',(#2113),#10187,.T.);
#10759=ADVANCED_FACE('',(#2114),#181,.T.);
#10760=ADVANCED_FACE('',(#2115),#182,.T.);
#10761=ADVANCED_FACE('',(#2116),#10188,.T.);
#10762=ADVANCED_FACE('',(#2117),#10189,.F.);
#10763=ADVANCED_FACE('',(#2118),#10190,.F.);
#10764=ADVANCED_FACE('',(#2119),#10191,.F.);
#10765=ADVANCED_FACE('',(#2120),#10192,.F.);
#10766=ADVANCED_FACE('',(#2121),#10193,.F.);
#10767=ADVANCED_FACE('',(#2122),#10194,.F.);
#10768=ADVANCED_FACE('',(#2123),#10195,.F.);
#10769=ADVANCED_FACE('',(#2124),#10196,.T.);
#10770=ADVANCED_FACE('',(#2125,#1433,#1434,#1435,#1436,#1437,#1438,#1439),
#1531,.T.);
#10771=ADVANCED_FACE('',(#2126,#1440,#1441,#1442,#1443,#1444,#1445,#1446),
#1532,.F.);
#10772=ADVANCED_FACE('',(#2127),#10197,.F.);
#10773=ADVANCED_FACE('',(#2128),#10198,.F.);
#10774=ADVANCED_FACE('',(#2129),#10199,.F.);
#10775=ADVANCED_FACE('',(#2130),#10200,.F.);
#10776=ADVANCED_FACE('',(#2131),#10201,.F.);
#10777=ADVANCED_FACE('',(#2132),#10202,.F.);
#10778=ADVANCED_FACE('',(#2133),#10203,.F.);
#10779=ADVANCED_FACE('',(#2134),#10204,.T.);
#10780=ADVANCED_FACE('',(#2135,#1447,#1448,#1449,#1450,#1451,#1452,#1453),
#1533,.T.);
#10781=ADVANCED_FACE('',(#2136,#1454,#1455,#1456,#1457,#1458,#1459,#1460),
#1534,.F.);
#10782=ADVANCED_FACE('',(#2137),#596,.T.);
#10783=ADVANCED_FACE('',(#2138),#227,.T.);
#10784=ADVANCED_FACE('',(#2139),#10205,.T.);
#10785=ADVANCED_FACE('',(#2140),#10206,.T.);
#10786=ADVANCED_FACE('',(#2141),#1535,.T.);
#10787=ADVANCED_FACE('',(#2142),#1536,.T.);
#10788=ADVANCED_FACE('',(#2143,#1461),#1537,.F.);
#10789=ADVANCED_FACE('',(#2144),#10207,.T.);
#10790=ADVANCED_FACE('',(#2145),#1538,.T.);
#10791=ADVANCED_FACE('',(#2146),#1539,.T.);
#10792=ADVANCED_FACE('',(#2147),#1540,.T.);
#10793=ADVANCED_FACE('',(#2148),#1541,.T.);
#10794=ADVANCED_FACE('',(#2149),#1542,.T.);
#10795=ADVANCED_FACE('',(#2150),#1543,.T.);
#10796=ADVANCED_FACE('',(#2151,#1462),#1544,.F.);
#10797=ADVANCED_FACE('',(#2152),#1545,.T.);
#10798=ADVANCED_FACE('',(#2153),#1546,.T.);
#10799=ADVANCED_FACE('',(#2154),#1547,.T.);
#10800=ADVANCED_FACE('',(#2155),#1548,.T.);
#10801=ADVANCED_FACE('',(#2156),#1549,.T.);
#10802=ADVANCED_FACE('',(#2157),#1550,.T.);
#10803=ADVANCED_FACE('',(#2158),#1551,.T.);
#10804=ADVANCED_FACE('',(#2159),#1552,.T.);
#10805=ADVANCED_FACE('',(#2160),#1553,.T.);
#10806=ADVANCED_FACE('',(#2161),#1554,.T.);
#10807=ADVANCED_FACE('',(#2162),#1555,.T.);
#10808=ADVANCED_FACE('',(#2163),#1556,.F.);
#10809=ADVANCED_FACE('',(#2164),#1557,.F.);
#10810=ADVANCED_FACE('',(#2165),#1558,.F.);
#10811=ADVANCED_FACE('',(#2166),#1559,.T.);
#10812=ADVANCED_FACE('',(#2167),#1560,.T.);
#10813=ADVANCED_FACE('',(#2168),#1561,.F.);
#10814=ADVANCED_FACE('',(#2169),#1562,.F.);
#10815=ADVANCED_FACE('',(#2170),#10208,.F.);
#10816=ADVANCED_FACE('',(#2171),#10209,.T.);
#10817=ADVANCED_FACE('',(#2172,#1463),#1563,.F.);
#10818=ADVANCED_FACE('',(#2173,#1464),#1564,.F.);
#10819=CLOSED_SHELL('',(#10210,#10211,#10212,#10213,#10214,#10215,#10216,
#10217,#10218,#10219,#10220,#10221,#10222,#10223,#10224,#10225,#10226,#10227,
#10228,#10229,#10230,#10231,#10232,#10233,#10234,#10235,#10236,#10237,#10238,
#10239,#10240,#10241,#10242,#10243,#10244,#10245,#10246));
#10820=CLOSED_SHELL('',(#10247,#10248,#10249,#10250,#10251,#10252,#10253,
#10254,#10255,#10256,#10257,#10258,#10259,#10260,#10261,#10262,#10263,#10264,
#10265,#10266,#10267,#10268,#10269,#10270,#10271,#10272,#10273,#10274,#10275));
#10821=CLOSED_SHELL('',(#10276,#10277,#10278,#10279,#10280,#10281,#10282,
#10283,#10284,#10285,#10286,#10287,#10288,#10289,#10290,#10291,#10292));
#10822=CLOSED_SHELL('',(#10293,#10294,#10295,#10296,#10297,#10298,#10299,
#10300,#10301,#10302,#10303,#10304,#10305,#10306,#10307,#10308,#10309,#10310,
#10311,#10312,#10313,#10314,#10315,#10316,#10317,#10318,#10319,#10320,#10321,
#10322,#10323,#10324,#10325,#10326,#10327,#10328,#10329,#10330,#10331,#10332,
#10333,#10334,#10335,#10336,#10337,#10338,#10339,#10340,#10341,#10342,#10343,
#10344,#10345,#10346,#10347,#10348,#10349,#10350,#10351,#10352,#10353,#10354,
#10355,#10356,#10357,#10358,#10359,#10360,#10361,#10362,#10363,#10364,#10365,
#10366,#10367,#10368,#10369,#10370,#10371,#10372,#10373,#10374,#10375,#10376,
#10377,#10378,#10379,#10380,#10381,#10382,#10383,#10384,#10385,#10386,#10387,
#10388,#10389,#10390,#10391,#10392,#10393,#10394,#10395,#10396,#10397,#10398,
#10399,#10400,#10401,#10402,#10403,#10404,#10405,#10406,#10407,#10408,#10409,
#10410,#10411,#10412,#10413,#10414,#10415,#10416,#10417,#10418,#10419,#10420,
#10421,#10422,#10423,#10424,#10425,#10426,#10427,#10428,#10429,#10430,#10431,
#10432,#10433,#10434,#10435,#10436,#10437,#10438,#10439,#10440,#10441,#10442,
#10443,#10444,#10445,#10446,#10447,#10448,#10449,#10450,#10451,#10452,#10453,
#10454,#10455,#10456,#10457,#10458,#10459,#10460,#10461,#10462,#10463,#10464,
#10465,#10466,#10467,#10468,#10469,#10470,#10471,#10472,#10473,#10474,#10475,
#10476,#10477,#10478,#10479,#10480,#10481,#10482,#10483,#10484,#10485,#10486,
#10487,#10488,#10489,#10490,#10491,#10492,#10493,#10494,#10495,#10496,#10497,
#10498,#10499,#10500,#10501,#10502,#10503,#10504,#10505,#10506,#10507,#10508,
#10509,#10510,#10511,#10512,#10513,#10514,#10515,#10516,#10517,#10518,#10519,
#10520,#10521,#10522,#10523,#10524,#10525,#10526,#10527,#10528,#10529,#10530,
#10531,#10532,#10533,#10534,#10535,#10536,#10537,#10538,#10539,#10540,#10541,
#10542,#10543,#10544,#10545,#10546,#10547,#10548,#10549,#10550,#10551,#10552,
#10553,#10554,#10555,#10556,#10557,#10558,#10559,#10560,#10561,#10562,#10563,
#10564,#10565,#10566,#10567,#10568,#10569,#10570,#10571,#10572,#10573,#10574,
#10575,#10576,#10577,#10578,#10579,#10580,#10581,#10582,#10583,#10584,#10585,
#10586,#10587,#10588,#10589,#10590,#10591,#10592,#10593,#10594,#10595,#10596,
#10597,#10598,#10599,#10600,#10601,#10602,#10603,#10604,#10605,#10606,#10607,
#10608,#10609,#10610,#10611,#10612,#10613,#10614,#10615,#10616,#10617,#10618,
#10619,#10620,#10621,#10622,#10623,#10624,#10625,#10626,#10627,#10628,#10629,
#10630,#10631,#10632,#10633,#10634,#10635,#10636,#10637,#10638,#10639,#10640,
#10641,#10642,#10643,#10644,#10645,#10646,#10647,#10648,#10649,#10650,#10651,
#10652,#10653,#10654,#10655,#10656,#10657,#10658,#10659,#10660,#10661,#10662,
#10663,#10664,#10665,#10666,#10667,#10668,#10669,#10670,#10671,#10672,#10673,
#10674,#10675,#10676,#10677,#10678,#10679,#10680,#10681,#10682,#10683,#10684,
#10685,#10686,#10687,#10688,#10689,#10690,#10691,#10692,#10693,#10694,#10695,
#10696));
#10823=CLOSED_SHELL('',(#10697,#10698,#10699,#10700,#10701,#10702,#10703,
#10704,#10705,#10706,#10707,#10708,#10709,#10710,#10711,#10712,#10713,#10714,
#10715,#10716,#10717,#10718,#10719,#10720,#10721,#10722,#10723,#10724,#10725,
#10726,#10727,#10728,#10729,#10730,#10731,#10732,#10733,#10734,#10735));
#10824=CLOSED_SHELL('',(#10736,#10737,#10738,#10739,#10740,#10741,#10742,
#10743,#10744,#10745,#10746,#10747,#10748,#10749,#10750,#10751,#10752,#10753,
#10754,#10755,#10756,#10757,#10758,#10759,#10760,#10761));
#10825=CLOSED_SHELL('',(#10762,#10763,#10764,#10765,#10766,#10767,#10768,
#10769,#10770,#10771));
#10826=CLOSED_SHELL('',(#10772,#10773,#10774,#10775,#10776,#10777,#10778,
#10779,#10780,#10781));
#10827=CLOSED_SHELL('',(#10782,#10783,#10784,#10785,#10786,#10787,#10788));
#10828=CLOSED_SHELL('',(#10789,#10790,#10791,#10792,#10793,#10794,#10795,
#10796,#10797,#10798));
#10829=CLOSED_SHELL('',(#10799,#10800,#10801,#10802,#10803,#10804,#10805,
#10806,#10807,#10808,#10809,#10810,#10811,#10812,#10813,#10814));
#10830=CLOSED_SHELL('',(#10815,#10816,#10817,#10818));
#10831=DERIVED_UNIT_ELEMENT(#10855,1.);
#10832=DERIVED_UNIT_ELEMENT(#37883,-3.);
#10833=DERIVED_UNIT_ELEMENT(#10855,1.);
#10834=DERIVED_UNIT_ELEMENT(#37883,-3.);
#10835=DERIVED_UNIT_ELEMENT(#10855,1.);
#10836=DERIVED_UNIT_ELEMENT(#37883,-3.);
#10837=DERIVED_UNIT_ELEMENT(#10855,1.);
#10838=DERIVED_UNIT_ELEMENT(#37883,-3.);
#10839=DERIVED_UNIT_ELEMENT(#10855,1.);
#10840=DERIVED_UNIT_ELEMENT(#37883,-3.);
#10841=DERIVED_UNIT_ELEMENT(#10855,1.);
#10842=DERIVED_UNIT_ELEMENT(#37883,-3.);
#10843=DERIVED_UNIT_ELEMENT(#10855,1.);
#10844=DERIVED_UNIT_ELEMENT(#37883,-3.);
#10845=DERIVED_UNIT_ELEMENT(#10855,1.);
#10846=DERIVED_UNIT_ELEMENT(#37883,-3.);
#10847=DERIVED_UNIT_ELEMENT(#10855,1.);
#10848=DERIVED_UNIT_ELEMENT(#37883,-3.);
#10849=DERIVED_UNIT_ELEMENT(#10855,1.);
#10850=DERIVED_UNIT_ELEMENT(#37883,-3.);
#10851=DERIVED_UNIT_ELEMENT(#10855,1.);
#10852=DERIVED_UNIT_ELEMENT(#37883,-3.);
#10853=DERIVED_UNIT_ELEMENT(#10855,1.);
#10854=DERIVED_UNIT_ELEMENT(#37883,-3.);
#10855=(
MASS_UNIT()
NAMED_UNIT(*)
SI_UNIT(.KILO.,.GRAM.)
);
#10856=DERIVED_UNIT((#10831,#10832));
#10857=DERIVED_UNIT((#10833,#10834));
#10858=DERIVED_UNIT((#10835,#10836));
#10859=DERIVED_UNIT((#10837,#10838));
#10860=DERIVED_UNIT((#10839,#10840));
#10861=DERIVED_UNIT((#10841,#10842));
#10862=DERIVED_UNIT((#10843,#10844));
#10863=DERIVED_UNIT((#10845,#10846));
#10864=DERIVED_UNIT((#10847,#10848));
#10865=DERIVED_UNIT((#10849,#10850));
#10866=DERIVED_UNIT((#10851,#10852));
#10867=DERIVED_UNIT((#10853,#10854));
#10868=MEASURE_REPRESENTATION_ITEM('density measure',
POSITIVE_RATIO_MEASURE(7850.),#10856);
#10869=MEASURE_REPRESENTATION_ITEM('density measure',
POSITIVE_RATIO_MEASURE(7850.),#10857);
#10870=MEASURE_REPRESENTATION_ITEM('density measure',
POSITIVE_RATIO_MEASURE(7850.),#10858);
#10871=MEASURE_REPRESENTATION_ITEM('density measure',
POSITIVE_RATIO_MEASURE(7850.),#10859);
#10872=MEASURE_REPRESENTATION_ITEM('density measure',
POSITIVE_RATIO_MEASURE(7850.),#10860);
#10873=MEASURE_REPRESENTATION_ITEM('density measure',
POSITIVE_RATIO_MEASURE(7850.),#10861);
#10874=MEASURE_REPRESENTATION_ITEM('density measure',
POSITIVE_RATIO_MEASURE(7850.),#10862);
#10875=MEASURE_REPRESENTATION_ITEM('density measure',
POSITIVE_RATIO_MEASURE(7850.),#10863);
#10876=MEASURE_REPRESENTATION_ITEM('density measure',
POSITIVE_RATIO_MEASURE(7850.),#10864);
#10877=MEASURE_REPRESENTATION_ITEM('density measure',
POSITIVE_RATIO_MEASURE(7850.),#10865);
#10878=MEASURE_REPRESENTATION_ITEM('density measure',
POSITIVE_RATIO_MEASURE(7850.),#10866);
#10879=MEASURE_REPRESENTATION_ITEM('density measure',
POSITIVE_RATIO_MEASURE(7850.),#10867);
#10880=PROPERTY_DEFINITION_REPRESENTATION(#10940,#10904);
#10881=PROPERTY_DEFINITION_REPRESENTATION(#10941,#10905);
#10882=PROPERTY_DEFINITION_REPRESENTATION(#10942,#10906);
#10883=PROPERTY_DEFINITION_REPRESENTATION(#10943,#10907);
#10884=PROPERTY_DEFINITION_REPRESENTATION(#10944,#10908);
#10885=PROPERTY_DEFINITION_REPRESENTATION(#10945,#10909);
#10886=PROPERTY_DEFINITION_REPRESENTATION(#10946,#10910);
#10887=PROPERTY_DEFINITION_REPRESENTATION(#10947,#10911);
#10888=PROPERTY_DEFINITION_REPRESENTATION(#10948,#10912);
#10889=PROPERTY_DEFINITION_REPRESENTATION(#10949,#10913);
#10890=PROPERTY_DEFINITION_REPRESENTATION(#10950,#10914);
#10891=PROPERTY_DEFINITION_REPRESENTATION(#10951,#10915);
#10892=PROPERTY_DEFINITION_REPRESENTATION(#10952,#10916);
#10893=PROPERTY_DEFINITION_REPRESENTATION(#10953,#10917);
#10894=PROPERTY_DEFINITION_REPRESENTATION(#10954,#10918);
#10895=PROPERTY_DEFINITION_REPRESENTATION(#10955,#10919);
#10896=PROPERTY_DEFINITION_REPRESENTATION(#10956,#10920);
#10897=PROPERTY_DEFINITION_REPRESENTATION(#10957,#10921);
#10898=PROPERTY_DEFINITION_REPRESENTATION(#10958,#10922);
#10899=PROPERTY_DEFINITION_REPRESENTATION(#10959,#10923);
#10900=PROPERTY_DEFINITION_REPRESENTATION(#10960,#10924);
#10901=PROPERTY_DEFINITION_REPRESENTATION(#10961,#10925);
#10902=PROPERTY_DEFINITION_REPRESENTATION(#10962,#10926);
#10903=PROPERTY_DEFINITION_REPRESENTATION(#10963,#10927);
#10904=REPRESENTATION('material name',(#10928),#37869);
#10905=REPRESENTATION('density',(#10868),#37869);
#10906=REPRESENTATION('material name',(#10929),#37870);
#10907=REPRESENTATION('density',(#10869),#37870);
#10908=REPRESENTATION('material name',(#10930),#37871);
#10909=REPRESENTATION('density',(#10870),#37871);
#10910=REPRESENTATION('material name',(#10931),#37872);
#10911=REPRESENTATION('density',(#10871),#37872);
#10912=REPRESENTATION('material name',(#10932),#37873);
#10913=REPRESENTATION('density',(#10872),#37873);
#10914=REPRESENTATION('material name',(#10933),#37874);
#10915=REPRESENTATION('density',(#10873),#37874);
#10916=REPRESENTATION('material name',(#10934),#37875);
#10917=REPRESENTATION('density',(#10874),#37875);
#10918=REPRESENTATION('material name',(#10935),#37876);
#10919=REPRESENTATION('density',(#10875),#37876);
#10920=REPRESENTATION('material name',(#10936),#37877);
#10921=REPRESENTATION('density',(#10876),#37877);
#10922=REPRESENTATION('material name',(#10937),#37878);
#10923=REPRESENTATION('density',(#10877),#37878);
#10924=REPRESENTATION('material name',(#10938),#37879);
#10925=REPRESENTATION('density',(#10878),#37879);
#10926=REPRESENTATION('material name',(#10939),#37880);
#10927=REPRESENTATION('density',(#10879),#37880);
#10928=DESCRIPTIVE_REPRESENTATION_ITEM('Steel','Steel');
#10929=DESCRIPTIVE_REPRESENTATION_ITEM('Steel','Steel');
#10930=DESCRIPTIVE_REPRESENTATION_ITEM('Steel','Steel');
#10931=DESCRIPTIVE_REPRESENTATION_ITEM('Steel','Steel');
#10932=DESCRIPTIVE_REPRESENTATION_ITEM('Steel','Steel');
#10933=DESCRIPTIVE_REPRESENTATION_ITEM('Steel','Steel');
#10934=DESCRIPTIVE_REPRESENTATION_ITEM('Steel','Steel');
#10935=DESCRIPTIVE_REPRESENTATION_ITEM('Steel','Steel');
#10936=DESCRIPTIVE_REPRESENTATION_ITEM('Steel','Steel');
#10937=DESCRIPTIVE_REPRESENTATION_ITEM('Steel','Steel');
#10938=DESCRIPTIVE_REPRESENTATION_ITEM('Steel','Steel');
#10939=DESCRIPTIVE_REPRESENTATION_ITEM('Steel','Steel');
#10940=PROPERTY_DEFINITION('material property','material name',#37968);
#10941=PROPERTY_DEFINITION('material property','density of part',#37968);
#10942=PROPERTY_DEFINITION('material property','material name',#37969);
#10943=PROPERTY_DEFINITION('material property','density of part',#37969);
#10944=PROPERTY_DEFINITION('material property','material name',#37970);
#10945=PROPERTY_DEFINITION('material property','density of part',#37970);
#10946=PROPERTY_DEFINITION('material property','material name',#37971);
#10947=PROPERTY_DEFINITION('material property','density of part',#37971);
#10948=PROPERTY_DEFINITION('material property','material name',#37972);
#10949=PROPERTY_DEFINITION('material property','density of part',#37972);
#10950=PROPERTY_DEFINITION('material property','material name',#37973);
#10951=PROPERTY_DEFINITION('material property','density of part',#37973);
#10952=PROPERTY_DEFINITION('material property','material name',#37974);
#10953=PROPERTY_DEFINITION('material property','density of part',#37974);
#10954=PROPERTY_DEFINITION('material property','material name',#37975);
#10955=PROPERTY_DEFINITION('material property','density of part',#37975);
#10956=PROPERTY_DEFINITION('material property','material name',#37976);
#10957=PROPERTY_DEFINITION('material property','density of part',#37976);
#10958=PROPERTY_DEFINITION('material property','material name',#37977);
#10959=PROPERTY_DEFINITION('material property','density of part',#37977);
#10960=PROPERTY_DEFINITION('material property','material name',#37978);
#10961=PROPERTY_DEFINITION('material property','density of part',#37978);
#10962=PROPERTY_DEFINITION('material property','material name',#37979);
#10963=PROPERTY_DEFINITION('material property','density of part',#37979);
#10964=AXIS2_PLACEMENT_3D('',#14043,#11890,#11891);
#10965=AXIS2_PLACEMENT_3D('',#14044,#11892,#11893);
#10966=AXIS2_PLACEMENT_3D('',#14045,#11894,#11895);
#10967=AXIS2_PLACEMENT_3D('',#14047,#11896,#11897);
#10968=AXIS2_PLACEMENT_3D('',#14050,#11899,#11900);
#10969=AXIS2_PLACEMENT_3D('',#14051,#11901,#11902);
#10970=AXIS2_PLACEMENT_3D('',#14053,#11903,#11904);
#10971=AXIS2_PLACEMENT_3D('',#14056,#11906,#11907);
#10972=AXIS2_PLACEMENT_3D('',#14057,#11908,#11909);
#10973=AXIS2_PLACEMENT_3D('',#14059,#11910,#11911);
#10974=AXIS2_PLACEMENT_3D('',#14062,#11913,#11914);
#10975=AXIS2_PLACEMENT_3D('',#14063,#11915,#11916);
#10976=AXIS2_PLACEMENT_3D('',#14065,#11917,#11918);
#10977=AXIS2_PLACEMENT_3D('',#14068,#11920,#11921);
#10978=AXIS2_PLACEMENT_3D('',#14069,#11922,#11923);
#10979=AXIS2_PLACEMENT_3D('',#14071,#11924,#11925);
#10980=AXIS2_PLACEMENT_3D('',#14074,#11927,#11928);
#10981=AXIS2_PLACEMENT_3D('',#14075,#11929,#11930);
#10982=AXIS2_PLACEMENT_3D('',#14077,#11931,#11932);
#10983=AXIS2_PLACEMENT_3D('',#14080,#11934,#11935);
#10984=AXIS2_PLACEMENT_3D('',#14081,#11936,#11937);
#10985=AXIS2_PLACEMENT_3D('',#14083,#11938,#11939);
#10986=AXIS2_PLACEMENT_3D('',#14086,#11941,#11942);
#10987=AXIS2_PLACEMENT_3D('',#14087,#11943,#11944);
#10988=AXIS2_PLACEMENT_3D('',#14089,#11945,#11946);
#10989=AXIS2_PLACEMENT_3D('',#14092,#11948,#11949);
#10990=AXIS2_PLACEMENT_3D('',#14093,#11950,#11951);
#10991=AXIS2_PLACEMENT_3D('',#14095,#11952,#11953);
#10992=AXIS2_PLACEMENT_3D('',#14098,#11955,#11956);
#10993=AXIS2_PLACEMENT_3D('',#14099,#11957,#11958);
#10994=AXIS2_PLACEMENT_3D('',#14101,#11959,#11960);
#10995=AXIS2_PLACEMENT_3D('',#14104,#11962,#11963);
#10996=AXIS2_PLACEMENT_3D('',#14105,#11964,#11965);
#10997=AXIS2_PLACEMENT_3D('',#14107,#11966,#11967);
#10998=AXIS2_PLACEMENT_3D('',#14110,#11969,#11970);
#10999=AXIS2_PLACEMENT_3D('',#14111,#11971,#11972);
#11000=AXIS2_PLACEMENT_3D('',#14128,#11981,#11982);
#11001=AXIS2_PLACEMENT_3D('',#14137,#11987,#11988);
#11002=AXIS2_PLACEMENT_3D('',#14146,#11993,#11994);
#11003=AXIS2_PLACEMENT_3D('',#14155,#11999,#12000);
#11004=AXIS2_PLACEMENT_3D('',#14164,#12005,#12006);
#11005=AXIS2_PLACEMENT_3D('',#14173,#12011,#12012);
#11006=AXIS2_PLACEMENT_3D('',#14174,#12013,#12014);
#11007=AXIS2_PLACEMENT_3D('',#14175,#12015,#12016);
#11008=AXIS2_PLACEMENT_3D('',#14176,#12017,#12018);
#11009=AXIS2_PLACEMENT_3D('',#14190,#12026,#12027);
#11010=AXIS2_PLACEMENT_3D('',#14196,#12031,#12032);
#11011=AXIS2_PLACEMENT_3D('',#14197,#12033,#12034);
#11012=AXIS2_PLACEMENT_3D('',#14198,#12035,#12036);
#11013=AXIS2_PLACEMENT_3D('',#14199,#12037,#12038);
#11014=AXIS2_PLACEMENT_3D('',#14201,#12040,#12041);
#11015=AXIS2_PLACEMENT_3D('',#14203,#12043,#12044);
#11016=AXIS2_PLACEMENT_3D('',#14204,#12045,#12046);
#11017=AXIS2_PLACEMENT_3D('',#14205,#12047,#12048);
#11018=AXIS2_PLACEMENT_3D('',#14206,#12049,#12050);
#11019=AXIS2_PLACEMENT_3D('',#14212,#12054,#12055);
#11020=AXIS2_PLACEMENT_3D('',#14216,#12058,#12059);
#11021=AXIS2_PLACEMENT_3D('',#14217,#12060,#12061);
#11022=AXIS2_PLACEMENT_3D('',#14221,#12064,#12065);
#11023=AXIS2_PLACEMENT_3D('',#14222,#12066,#12067);
#11024=AXIS2_PLACEMENT_3D('',#14223,#12068,#12069);
#11025=AXIS2_PLACEMENT_3D('',#14225,#12071,#12072);
#11026=AXIS2_PLACEMENT_3D('',#14226,#12073,#12074);
#11027=AXIS2_PLACEMENT_3D('',#14235,#12079,#12080);
#11028=AXIS2_PLACEMENT_3D('',#14236,#12081,#12082);
#11029=AXIS2_PLACEMENT_3D('',#14237,#12083,#12084);
#11030=AXIS2_PLACEMENT_3D('',#14238,#12085,#12086);
#11031=AXIS2_PLACEMENT_3D('',#14239,#12087,#12088);
#11032=AXIS2_PLACEMENT_3D('',#14240,#12089,#12090);
#11033=AXIS2_PLACEMENT_3D('',#14241,#12091,#12092);
#11034=AXIS2_PLACEMENT_3D('',#14242,#12093,#12094);
#11035=AXIS2_PLACEMENT_3D('',#14243,#12095,#12096);
#11036=AXIS2_PLACEMENT_3D('',#14244,#12097,#12098);
#11037=AXIS2_PLACEMENT_3D('',#14245,#12099,#12100);
#11038=AXIS2_PLACEMENT_3D('',#14246,#12101,#12102);
#11039=AXIS2_PLACEMENT_3D('',#14247,#12103,#12104);
#11040=AXIS2_PLACEMENT_3D('',#14248,#12105,#12106);
#11041=AXIS2_PLACEMENT_3D('',#14249,#12107,#12108);
#11042=AXIS2_PLACEMENT_3D('',#14250,#12109,#12110);
#11043=AXIS2_PLACEMENT_3D('',#14300,#12114,#12115);
#11044=AXIS2_PLACEMENT_3D('',#14337,#12116,#12117);
#11045=AXIS2_PLACEMENT_3D('',#14415,#12119,#12120);
#11046=AXIS2_PLACEMENT_3D('',#14493,#12122,#12123);
#11047=AXIS2_PLACEMENT_3D('',#14574,#12125,#12126);
#11048=AXIS2_PLACEMENT_3D('',#14655,#12128,#12129);
#11049=AXIS2_PLACEMENT_3D('',#14731,#12131,#12132);
#11050=AXIS2_PLACEMENT_3D('',#14733,#12133,#12134);
#11051=AXIS2_PLACEMENT_3D('',#14818,#12138,#12139);
#11052=AXIS2_PLACEMENT_3D('',#14821,#12140,#12141);
#11053=AXIS2_PLACEMENT_3D('',#14822,#12142,#12143);
#11054=AXIS2_PLACEMENT_3D('',#14825,#12145,#12146);
#11055=AXIS2_PLACEMENT_3D('',#14826,#12147,#12148);
#11056=AXIS2_PLACEMENT_3D('',#14829,#12149,#12150);
#11057=AXIS2_PLACEMENT_3D('',#14833,#12152,#12153);
#11058=AXIS2_PLACEMENT_3D('',#14836,#12155,#12156);
#11059=AXIS2_PLACEMENT_3D('',#14838,#12157,#12158);
#11060=AXIS2_PLACEMENT_3D('',#14840,#12160,#12161);
#11061=AXIS2_PLACEMENT_3D('',#14842,#12162,#12163);
#11062=AXIS2_PLACEMENT_3D('',#14845,#12165,#12166);
#11063=AXIS2_PLACEMENT_3D('',#14846,#12167,#12168);
#11064=AXIS2_PLACEMENT_3D('',#14848,#12169,#12170);
#11065=AXIS2_PLACEMENT_3D('',#14850,#12172,#12173);
#11066=AXIS2_PLACEMENT_3D('',#14925,#12174,#12175);
#11067=AXIS2_PLACEMENT_3D('',#14926,#12176,#12177);
#11068=AXIS2_PLACEMENT_3D('',#14927,#12178,#12179);
#11069=AXIS2_PLACEMENT_3D('',#14928,#12180,#12181);
#11070=AXIS2_PLACEMENT_3D('',#14933,#12184,#12185);
#11071=AXIS2_PLACEMENT_3D('',#15728,#12187,#12188);
#11072=AXIS2_PLACEMENT_3D('',#16069,#12190,#12191);
#11073=AXIS2_PLACEMENT_3D('',#16073,#12193,#12194);
#11074=AXIS2_PLACEMENT_3D('',#17205,#12196,#12197);
#11075=AXIS2_PLACEMENT_3D('',#17211,#12201,#12202);
#11076=AXIS2_PLACEMENT_3D('',#17215,#12205,#12206);
#11077=AXIS2_PLACEMENT_3D('',#17219,#12209,#12210);
#11078=AXIS2_PLACEMENT_3D('',#17221,#12212,#12213);
#11079=AXIS2_PLACEMENT_3D('',#17222,#12214,#12215);
#11080=AXIS2_PLACEMENT_3D('',#17223,#12216,#12217);
#11081=AXIS2_PLACEMENT_3D('',#17224,#12218,#12219);
#11082=AXIS2_PLACEMENT_3D('',#17227,#12220,#12221);
#11083=AXIS2_PLACEMENT_3D('',#17228,#12222,#12223);
#11084=AXIS2_PLACEMENT_3D('',#17231,#12225,#12226);
#11085=AXIS2_PLACEMENT_3D('',#17232,#12227,#12228);
#11086=AXIS2_PLACEMENT_3D('',#17234,#12229,#12230);
#11087=AXIS2_PLACEMENT_3D('',#17237,#12232,#12233);
#11088=AXIS2_PLACEMENT_3D('',#17238,#12234,#12235);
#11089=AXIS2_PLACEMENT_3D('',#17241,#12236,#12237);
#11090=AXIS2_PLACEMENT_3D('',#17245,#12239,#12240);
#11091=AXIS2_PLACEMENT_3D('',#17247,#12242,#12243);
#11092=AXIS2_PLACEMENT_3D('',#17250,#12245,#12246);
#11093=AXIS2_PLACEMENT_3D('',#17251,#12247,#12248);
#11094=AXIS2_PLACEMENT_3D('',#17253,#12249,#12250);
#11095=AXIS2_PLACEMENT_3D('',#17257,#12252,#12253);
#11096=AXIS2_PLACEMENT_3D('',#17261,#12255,#12256);
#11097=AXIS2_PLACEMENT_3D('',#17264,#12258,#12259);
#11098=AXIS2_PLACEMENT_3D('',#17265,#12260,#12261);
#11099=AXIS2_PLACEMENT_3D('',#17271,#12265,#12266);
#11100=AXIS2_PLACEMENT_3D('',#17272,#12267,#12268);
#11101=AXIS2_PLACEMENT_3D('',#17278,#12272,#12273);
#11102=AXIS2_PLACEMENT_3D('',#17284,#12277,#12278);
#11103=AXIS2_PLACEMENT_3D('',#17287,#12281,#12282);
#11104=AXIS2_PLACEMENT_3D('',#17288,#12283,#12284);
#11105=AXIS2_PLACEMENT_3D('',#17289,#12285,#12286);
#11106=AXIS2_PLACEMENT_3D('',#17290,#12287,#12288);
#11107=AXIS2_PLACEMENT_3D('',#17296,#12292,#12293);
#11108=AXIS2_PLACEMENT_3D('',#17298,#12295,#12296);
#11109=AXIS2_PLACEMENT_3D('',#17300,#12298,#12299);
#11110=AXIS2_PLACEMENT_3D('',#17301,#12300,#12301);
#11111=AXIS2_PLACEMENT_3D('',#17302,#12302,#12303);
#11112=AXIS2_PLACEMENT_3D('',#17319,#12304,#12305);
#11113=AXIS2_PLACEMENT_3D('',#17342,#12306,#12307);
#11114=AXIS2_PLACEMENT_3D('',#17343,#12308,#12309);
#11115=AXIS2_PLACEMENT_3D('',#17360,#12310,#12311);
#11116=AXIS2_PLACEMENT_3D('',#17383,#12312,#12313);
#11117=AXIS2_PLACEMENT_3D('',#17384,#12314,#12315);
#11118=AXIS2_PLACEMENT_3D('',#17407,#12316,#12317);
#11119=AXIS2_PLACEMENT_3D('',#17430,#12318,#12319);
#11120=AXIS2_PLACEMENT_3D('',#17431,#12320,#12321);
#11121=AXIS2_PLACEMENT_3D('',#17448,#12322,#12323);
#11122=AXIS2_PLACEMENT_3D('',#17465,#12324,#12325);
#11123=AXIS2_PLACEMENT_3D('',#17466,#12326,#12327);
#11124=AXIS2_PLACEMENT_3D('',#17483,#12328,#12329);
#11125=AXIS2_PLACEMENT_3D('',#17506,#12330,#12331);
#11126=AXIS2_PLACEMENT_3D('',#17507,#12332,#12333);
#11127=AXIS2_PLACEMENT_3D('',#17524,#12334,#12335);
#11128=AXIS2_PLACEMENT_3D('',#17547,#12336,#12337);
#11129=AXIS2_PLACEMENT_3D('',#17548,#12338,#12339);
#11130=AXIS2_PLACEMENT_3D('',#17565,#12340,#12341);
#11131=AXIS2_PLACEMENT_3D('',#17588,#12342,#12343);
#11132=AXIS2_PLACEMENT_3D('',#17589,#12344,#12345);
#11133=AXIS2_PLACEMENT_3D('',#17606,#12346,#12347);
#11134=AXIS2_PLACEMENT_3D('',#17629,#12348,#12349);
#11135=AXIS2_PLACEMENT_3D('',#17630,#12350,#12351);
#11136=AXIS2_PLACEMENT_3D('',#17647,#12352,#12353);
#11137=AXIS2_PLACEMENT_3D('',#17670,#12354,#12355);
#11138=AXIS2_PLACEMENT_3D('',#17671,#12356,#12357);
#11139=AXIS2_PLACEMENT_3D('',#17688,#12358,#12359);
#11140=AXIS2_PLACEMENT_3D('',#17711,#12360,#12361);
#11141=AXIS2_PLACEMENT_3D('',#17712,#12362,#12363);
#11142=AXIS2_PLACEMENT_3D('',#17729,#12364,#12365);
#11143=AXIS2_PLACEMENT_3D('',#17752,#12366,#12367);
#11144=AXIS2_PLACEMENT_3D('',#17753,#12368,#12369);
#11145=AXIS2_PLACEMENT_3D('',#17776,#12370,#12371);
#11146=AXIS2_PLACEMENT_3D('',#17799,#12372,#12373);
#11147=AXIS2_PLACEMENT_3D('',#17800,#12374,#12375);
#11148=AXIS2_PLACEMENT_3D('',#17817,#12376,#12377);
#11149=AXIS2_PLACEMENT_3D('',#17834,#12378,#12379);
#11150=AXIS2_PLACEMENT_3D('',#17835,#12380,#12381);
#11151=AXIS2_PLACEMENT_3D('',#17852,#12382,#12383);
#11152=AXIS2_PLACEMENT_3D('',#17875,#12384,#12385);
#11153=AXIS2_PLACEMENT_3D('',#17876,#12386,#12387);
#11154=AXIS2_PLACEMENT_3D('',#17893,#12388,#12389);
#11155=AXIS2_PLACEMENT_3D('',#17916,#12390,#12391);
#11156=AXIS2_PLACEMENT_3D('',#17917,#12392,#12393);
#11157=AXIS2_PLACEMENT_3D('',#17934,#12394,#12395);
#11158=AXIS2_PLACEMENT_3D('',#17957,#12396,#12397);
#11159=AXIS2_PLACEMENT_3D('',#17958,#12398,#12399);
#11160=AXIS2_PLACEMENT_3D('',#17975,#12400,#12401);
#11161=AXIS2_PLACEMENT_3D('',#17998,#12402,#12403);
#11162=AXIS2_PLACEMENT_3D('',#17999,#12404,#12405);
#11163=AXIS2_PLACEMENT_3D('',#18016,#12406,#12407);
#11164=AXIS2_PLACEMENT_3D('',#18039,#12408,#12409);
#11165=AXIS2_PLACEMENT_3D('',#18040,#12410,#12411);
#11166=AXIS2_PLACEMENT_3D('',#18057,#12412,#12413);
#11167=AXIS2_PLACEMENT_3D('',#18080,#12414,#12415);
#11168=AXIS2_PLACEMENT_3D('',#18081,#12416,#12417);
#11169=AXIS2_PLACEMENT_3D('',#18098,#12418,#12419);
#11170=AXIS2_PLACEMENT_3D('',#18121,#12420,#12421);
#11171=AXIS2_PLACEMENT_3D('',#18122,#12422,#12423);
#11172=AXIS2_PLACEMENT_3D('',#18139,#12424,#12425);
#11173=AXIS2_PLACEMENT_3D('',#18162,#12426,#12427);
#11174=AXIS2_PLACEMENT_3D('',#18163,#12428,#12429);
#11175=AXIS2_PLACEMENT_3D('',#18180,#12430,#12431);
#11176=AXIS2_PLACEMENT_3D('',#18203,#12432,#12433);
#11177=AXIS2_PLACEMENT_3D('',#18204,#12434,#12435);
#11178=AXIS2_PLACEMENT_3D('',#18221,#12436,#12437);
#11179=AXIS2_PLACEMENT_3D('',#18244,#12438,#12439);
#11180=AXIS2_PLACEMENT_3D('',#18245,#12440,#12441);
#11181=AXIS2_PLACEMENT_3D('',#18262,#12442,#12443);
#11182=AXIS2_PLACEMENT_3D('',#18285,#12444,#12445);
#11183=AXIS2_PLACEMENT_3D('',#18286,#12446,#12447);
#11184=AXIS2_PLACEMENT_3D('',#18309,#12448,#12449);
#11185=AXIS2_PLACEMENT_3D('',#18332,#12450,#12451);
#11186=AXIS2_PLACEMENT_3D('',#18333,#12452,#12453);
#11187=AXIS2_PLACEMENT_3D('',#18356,#12454,#12455);
#11188=AXIS2_PLACEMENT_3D('',#18373,#12456,#12457);
#11189=AXIS2_PLACEMENT_3D('',#18374,#12458,#12459);
#11190=AXIS2_PLACEMENT_3D('',#18391,#12460,#12461);
#11191=AXIS2_PLACEMENT_3D('',#18408,#12462,#12463);
#11192=AXIS2_PLACEMENT_3D('',#18409,#12464,#12465);
#11193=AXIS2_PLACEMENT_3D('',#18426,#12466,#12467);
#11194=AXIS2_PLACEMENT_3D('',#18449,#12468,#12469);
#11195=AXIS2_PLACEMENT_3D('',#18450,#12470,#12471);
#11196=AXIS2_PLACEMENT_3D('',#18467,#12472,#12473);
#11197=AXIS2_PLACEMENT_3D('',#18490,#12474,#12475);
#11198=AXIS2_PLACEMENT_3D('',#18491,#12476,#12477);
#11199=AXIS2_PLACEMENT_3D('',#18508,#12478,#12479);
#11200=AXIS2_PLACEMENT_3D('',#18531,#12480,#12481);
#11201=AXIS2_PLACEMENT_3D('',#18532,#12482,#12483);
#11202=AXIS2_PLACEMENT_3D('',#18549,#12484,#12485);
#11203=AXIS2_PLACEMENT_3D('',#18572,#12486,#12487);
#11204=AXIS2_PLACEMENT_3D('',#18573,#12488,#12489);
#11205=AXIS2_PLACEMENT_3D('',#18590,#12490,#12491);
#11206=AXIS2_PLACEMENT_3D('',#18613,#12492,#12493);
#11207=AXIS2_PLACEMENT_3D('',#18614,#12494,#12495);
#11208=AXIS2_PLACEMENT_3D('',#18637,#12496,#12497);
#11209=AXIS2_PLACEMENT_3D('',#18660,#12498,#12499);
#11210=AXIS2_PLACEMENT_3D('',#18661,#12500,#12501);
#11211=AXIS2_PLACEMENT_3D('',#18684,#12502,#12503);
#11212=AXIS2_PLACEMENT_3D('',#18701,#12504,#12505);
#11213=AXIS2_PLACEMENT_3D('',#18702,#12506,#12507);
#11214=AXIS2_PLACEMENT_3D('',#18719,#12508,#12509);
#11215=AXIS2_PLACEMENT_3D('',#18736,#12510,#12511);
#11216=AXIS2_PLACEMENT_3D('',#18737,#12512,#12513);
#11217=AXIS2_PLACEMENT_3D('',#18754,#12514,#12515);
#11218=AXIS2_PLACEMENT_3D('',#18777,#12516,#12517);
#11219=AXIS2_PLACEMENT_3D('',#18778,#12518,#12519);
#11220=AXIS2_PLACEMENT_3D('',#18795,#12520,#12521);
#11221=AXIS2_PLACEMENT_3D('',#18818,#12522,#12523);
#11222=AXIS2_PLACEMENT_3D('',#18819,#12524,#12525);
#11223=AXIS2_PLACEMENT_3D('',#18836,#12526,#12527);
#11224=AXIS2_PLACEMENT_3D('',#18859,#12528,#12529);
#11225=AXIS2_PLACEMENT_3D('',#18860,#12530,#12531);
#11226=AXIS2_PLACEMENT_3D('',#18877,#12532,#12533);
#11227=AXIS2_PLACEMENT_3D('',#18900,#12534,#12535);
#11228=AXIS2_PLACEMENT_3D('',#18901,#12536,#12537);
#11229=AXIS2_PLACEMENT_3D('',#18918,#12538,#12539);
#11230=AXIS2_PLACEMENT_3D('',#18941,#12540,#12541);
#11231=AXIS2_PLACEMENT_3D('',#18942,#12542,#12543);
#11232=AXIS2_PLACEMENT_3D('',#18959,#12544,#12545);
#11233=AXIS2_PLACEMENT_3D('',#18982,#12546,#12547);
#11234=AXIS2_PLACEMENT_3D('',#18983,#12548,#12549);
#11235=AXIS2_PLACEMENT_3D('',#19000,#12550,#12551);
#11236=AXIS2_PLACEMENT_3D('',#19023,#12552,#12553);
#11237=AXIS2_PLACEMENT_3D('',#19024,#12554,#12555);
#11238=AXIS2_PLACEMENT_3D('',#19041,#12556,#12557);
#11239=AXIS2_PLACEMENT_3D('',#19058,#12558,#12559);
#11240=AXIS2_PLACEMENT_3D('',#19059,#12560,#12561);
#11241=AXIS2_PLACEMENT_3D('',#19082,#12562,#12563);
#11242=AXIS2_PLACEMENT_3D('',#19105,#12564,#12565);
#11243=AXIS2_PLACEMENT_3D('',#19106,#12566,#12567);
#11244=AXIS2_PLACEMENT_3D('',#19130,#12568,#12569);
#11245=AXIS2_PLACEMENT_3D('',#19159,#12570,#12571);
#11246=AXIS2_PLACEMENT_3D('',#19188,#12572,#12573);
#11247=AXIS2_PLACEMENT_3D('',#19217,#12574,#12575);
#11248=AXIS2_PLACEMENT_3D('',#19246,#12576,#12577);
#11249=AXIS2_PLACEMENT_3D('',#19275,#12578,#12579);
#11250=AXIS2_PLACEMENT_3D('',#19304,#12580,#12581);
#11251=AXIS2_PLACEMENT_3D('',#19333,#12582,#12583);
#11252=AXIS2_PLACEMENT_3D('',#19362,#12584,#12585);
#11253=AXIS2_PLACEMENT_3D('',#19391,#12586,#12587);
#11254=AXIS2_PLACEMENT_3D('',#19420,#12588,#12589);
#11255=AXIS2_PLACEMENT_3D('',#19449,#12590,#12591);
#11256=AXIS2_PLACEMENT_3D('',#19478,#12592,#12593);
#11257=AXIS2_PLACEMENT_3D('',#19507,#12594,#12595);
#11258=AXIS2_PLACEMENT_3D('',#19536,#12596,#12597);
#11259=AXIS2_PLACEMENT_3D('',#19565,#12598,#12599);
#11260=AXIS2_PLACEMENT_3D('',#19594,#12600,#12601);
#11261=AXIS2_PLACEMENT_3D('',#19623,#12602,#12603);
#11262=AXIS2_PLACEMENT_3D('',#19652,#12604,#12605);
#11263=AXIS2_PLACEMENT_3D('',#19681,#12606,#12607);
#11264=AXIS2_PLACEMENT_3D('',#19710,#12608,#12609);
#11265=AXIS2_PLACEMENT_3D('',#19739,#12610,#12611);
#11266=AXIS2_PLACEMENT_3D('',#19757,#12613,#12614);
#11267=AXIS2_PLACEMENT_3D('',#19778,#12615,#12616);
#11268=AXIS2_PLACEMENT_3D('',#19807,#12617,#12618);
#11269=AXIS2_PLACEMENT_3D('',#19836,#12619,#12620);
#11270=AXIS2_PLACEMENT_3D('',#19865,#12621,#12622);
#11271=AXIS2_PLACEMENT_3D('',#19894,#12623,#12624);
#11272=AXIS2_PLACEMENT_3D('',#19923,#12625,#12626);
#11273=AXIS2_PLACEMENT_3D('',#19952,#12627,#12628);
#11274=AXIS2_PLACEMENT_3D('',#19981,#12629,#12630);
#11275=AXIS2_PLACEMENT_3D('',#20010,#12631,#12632);
#11276=AXIS2_PLACEMENT_3D('',#20039,#12633,#12634);
#11277=AXIS2_PLACEMENT_3D('',#20068,#12635,#12636);
#11278=AXIS2_PLACEMENT_3D('',#20097,#12637,#12638);
#11279=AXIS2_PLACEMENT_3D('',#20126,#12639,#12640);
#11280=AXIS2_PLACEMENT_3D('',#20155,#12641,#12642);
#11281=AXIS2_PLACEMENT_3D('',#20184,#12643,#12644);
#11282=AXIS2_PLACEMENT_3D('',#20213,#12645,#12646);
#11283=AXIS2_PLACEMENT_3D('',#20242,#12647,#12648);
#11284=AXIS2_PLACEMENT_3D('',#20271,#12649,#12650);
#11285=AXIS2_PLACEMENT_3D('',#20300,#12651,#12652);
#11286=AXIS2_PLACEMENT_3D('',#20329,#12653,#12654);
#11287=AXIS2_PLACEMENT_3D('',#20358,#12655,#12656);
#11288=AXIS2_PLACEMENT_3D('',#20387,#12657,#12658);
#11289=AXIS2_PLACEMENT_3D('',#20395,#12659,#12660);
#11290=AXIS2_PLACEMENT_3D('',#20398,#12661,#12662);
#11291=AXIS2_PLACEMENT_3D('',#20402,#12664,#12665);
#11292=AXIS2_PLACEMENT_3D('',#20404,#12667,#12668);
#11293=AXIS2_PLACEMENT_3D('',#20428,#12669,#12670);
#11294=AXIS2_PLACEMENT_3D('',#20457,#12671,#12672);
#11295=AXIS2_PLACEMENT_3D('',#20486,#12673,#12674);
#11296=AXIS2_PLACEMENT_3D('',#20515,#12675,#12676);
#11297=AXIS2_PLACEMENT_3D('',#20544,#12677,#12678);
#11298=AXIS2_PLACEMENT_3D('',#20573,#12679,#12680);
#11299=AXIS2_PLACEMENT_3D('',#20602,#12681,#12682);
#11300=AXIS2_PLACEMENT_3D('',#20631,#12683,#12684);
#11301=AXIS2_PLACEMENT_3D('',#20660,#12685,#12686);
#11302=AXIS2_PLACEMENT_3D('',#20689,#12687,#12688);
#11303=AXIS2_PLACEMENT_3D('',#20718,#12689,#12690);
#11304=AXIS2_PLACEMENT_3D('',#20747,#12691,#12692);
#11305=AXIS2_PLACEMENT_3D('',#20776,#12693,#12694);
#11306=AXIS2_PLACEMENT_3D('',#20805,#12695,#12696);
#11307=AXIS2_PLACEMENT_3D('',#20834,#12697,#12698);
#11308=AXIS2_PLACEMENT_3D('',#20863,#12699,#12700);
#11309=AXIS2_PLACEMENT_3D('',#20892,#12701,#12702);
#11310=AXIS2_PLACEMENT_3D('',#20921,#12703,#12704);
#11311=AXIS2_PLACEMENT_3D('',#20950,#12705,#12706);
#11312=AXIS2_PLACEMENT_3D('',#20979,#12707,#12708);
#11313=AXIS2_PLACEMENT_3D('',#21008,#12709,#12710);
#11314=AXIS2_PLACEMENT_3D('',#21037,#12711,#12712);
#11315=AXIS2_PLACEMENT_3D('',#21059,#12714,#12715);
#11316=AXIS2_PLACEMENT_3D('',#21076,#12716,#12717);
#11317=AXIS2_PLACEMENT_3D('',#21105,#12718,#12719);
#11318=AXIS2_PLACEMENT_3D('',#21134,#12720,#12721);
#11319=AXIS2_PLACEMENT_3D('',#21163,#12722,#12723);
#11320=AXIS2_PLACEMENT_3D('',#21192,#12724,#12725);
#11321=AXIS2_PLACEMENT_3D('',#21221,#12726,#12727);
#11322=AXIS2_PLACEMENT_3D('',#21250,#12728,#12729);
#11323=AXIS2_PLACEMENT_3D('',#21279,#12730,#12731);
#11324=AXIS2_PLACEMENT_3D('',#21308,#12732,#12733);
#11325=AXIS2_PLACEMENT_3D('',#21337,#12734,#12735);
#11326=AXIS2_PLACEMENT_3D('',#21366,#12736,#12737);
#11327=AXIS2_PLACEMENT_3D('',#21395,#12738,#12739);
#11328=AXIS2_PLACEMENT_3D('',#21424,#12740,#12741);
#11329=AXIS2_PLACEMENT_3D('',#21453,#12742,#12743);
#11330=AXIS2_PLACEMENT_3D('',#21482,#12744,#12745);
#11331=AXIS2_PLACEMENT_3D('',#21511,#12746,#12747);
#11332=AXIS2_PLACEMENT_3D('',#21540,#12748,#12749);
#11333=AXIS2_PLACEMENT_3D('',#21569,#12750,#12751);
#11334=AXIS2_PLACEMENT_3D('',#21598,#12752,#12753);
#11335=AXIS2_PLACEMENT_3D('',#21627,#12754,#12755);
#11336=AXIS2_PLACEMENT_3D('',#21656,#12756,#12757);
#11337=AXIS2_PLACEMENT_3D('',#21685,#12758,#12759);
#11338=AXIS2_PLACEMENT_3D('',#21693,#12760,#12761);
#11339=AXIS2_PLACEMENT_3D('',#21706,#12762,#12763);
#11340=AXIS2_PLACEMENT_3D('',#21719,#12764,#12765);
#11341=AXIS2_PLACEMENT_3D('',#21732,#12766,#12767);
#11342=AXIS2_PLACEMENT_3D('',#21745,#12768,#12769);
#11343=AXIS2_PLACEMENT_3D('',#21758,#12770,#12771);
#11344=AXIS2_PLACEMENT_3D('',#21771,#12772,#12773);
#11345=AXIS2_PLACEMENT_3D('',#21784,#12774,#12775);
#11346=AXIS2_PLACEMENT_3D('',#21797,#12776,#12777);
#11347=AXIS2_PLACEMENT_3D('',#21810,#12778,#12779);
#11348=AXIS2_PLACEMENT_3D('',#21823,#12780,#12781);
#11349=AXIS2_PLACEMENT_3D('',#21836,#12782,#12783);
#11350=AXIS2_PLACEMENT_3D('',#21849,#12784,#12785);
#11351=AXIS2_PLACEMENT_3D('',#21862,#12786,#12787);
#11352=AXIS2_PLACEMENT_3D('',#21875,#12788,#12789);
#11353=AXIS2_PLACEMENT_3D('',#21888,#12790,#12791);
#11354=AXIS2_PLACEMENT_3D('',#21901,#12792,#12793);
#11355=AXIS2_PLACEMENT_3D('',#21914,#12794,#12795);
#11356=AXIS2_PLACEMENT_3D('',#21927,#12796,#12797);
#11357=AXIS2_PLACEMENT_3D('',#21940,#12798,#12799);
#11358=AXIS2_PLACEMENT_3D('',#21953,#12800,#12801);
#11359=AXIS2_PLACEMENT_3D('',#21966,#12802,#12803);
#11360=AXIS2_PLACEMENT_3D('',#21979,#12804,#12805);
#11361=AXIS2_PLACEMENT_3D('',#21992,#12806,#12807);
#11362=AXIS2_PLACEMENT_3D('',#22005,#12808,#12809);
#11363=AXIS2_PLACEMENT_3D('',#22018,#12810,#12811);
#11364=AXIS2_PLACEMENT_3D('',#22031,#12812,#12813);
#11365=AXIS2_PLACEMENT_3D('',#22044,#12814,#12815);
#11366=AXIS2_PLACEMENT_3D('',#22057,#12816,#12817);
#11367=AXIS2_PLACEMENT_3D('',#22070,#12818,#12819);
#11368=AXIS2_PLACEMENT_3D('',#22083,#12820,#12821);
#11369=AXIS2_PLACEMENT_3D('',#22096,#12822,#12823);
#11370=AXIS2_PLACEMENT_3D('',#22109,#12824,#12825);
#11371=AXIS2_PLACEMENT_3D('',#22122,#12826,#12827);
#11372=AXIS2_PLACEMENT_3D('',#22135,#12828,#12829);
#11373=AXIS2_PLACEMENT_3D('',#22148,#12830,#12831);
#11374=AXIS2_PLACEMENT_3D('',#22161,#12832,#12833);
#11375=AXIS2_PLACEMENT_3D('',#22174,#12834,#12835);
#11376=AXIS2_PLACEMENT_3D('',#22187,#12836,#12837);
#11377=AXIS2_PLACEMENT_3D('',#22200,#12838,#12839);
#11378=AXIS2_PLACEMENT_3D('',#22213,#12840,#12841);
#11379=AXIS2_PLACEMENT_3D('',#22226,#12842,#12843);
#11380=AXIS2_PLACEMENT_3D('',#22239,#12844,#12845);
#11381=AXIS2_PLACEMENT_3D('',#22252,#12846,#12847);
#11382=AXIS2_PLACEMENT_3D('',#22265,#12848,#12849);
#11383=AXIS2_PLACEMENT_3D('',#22278,#12850,#12851);
#11384=AXIS2_PLACEMENT_3D('',#22291,#12852,#12853);
#11385=AXIS2_PLACEMENT_3D('',#22304,#12854,#12855);
#11386=AXIS2_PLACEMENT_3D('',#22317,#12856,#12857);
#11387=AXIS2_PLACEMENT_3D('',#22330,#12858,#12859);
#11388=AXIS2_PLACEMENT_3D('',#22343,#12860,#12861);
#11389=AXIS2_PLACEMENT_3D('',#22356,#12862,#12863);
#11390=AXIS2_PLACEMENT_3D('',#22369,#12864,#12865);
#11391=AXIS2_PLACEMENT_3D('',#22382,#12866,#12867);
#11392=AXIS2_PLACEMENT_3D('',#22395,#12868,#12869);
#11393=AXIS2_PLACEMENT_3D('',#22408,#12870,#12871);
#11394=AXIS2_PLACEMENT_3D('',#22421,#12872,#12873);
#11395=AXIS2_PLACEMENT_3D('',#22434,#12874,#12875);
#11396=AXIS2_PLACEMENT_3D('',#22447,#12876,#12877);
#11397=AXIS2_PLACEMENT_3D('',#22460,#12878,#12879);
#11398=AXIS2_PLACEMENT_3D('',#22473,#12880,#12881);
#11399=AXIS2_PLACEMENT_3D('',#22486,#12882,#12883);
#11400=AXIS2_PLACEMENT_3D('',#22499,#12884,#12885);
#11401=AXIS2_PLACEMENT_3D('',#22512,#12886,#12887);
#11402=AXIS2_PLACEMENT_3D('',#22525,#12888,#12889);
#11403=AXIS2_PLACEMENT_3D('',#22538,#12890,#12891);
#11404=AXIS2_PLACEMENT_3D('',#22551,#12892,#12893);
#11405=AXIS2_PLACEMENT_3D('',#22564,#12894,#12895);
#11406=AXIS2_PLACEMENT_3D('',#22577,#12896,#12897);
#11407=AXIS2_PLACEMENT_3D('',#22590,#12898,#12899);
#11408=AXIS2_PLACEMENT_3D('',#22603,#12900,#12901);
#11409=AXIS2_PLACEMENT_3D('',#22616,#12902,#12903);
#11410=AXIS2_PLACEMENT_3D('',#22629,#12904,#12905);
#11411=AXIS2_PLACEMENT_3D('',#22642,#12906,#12907);
#11412=AXIS2_PLACEMENT_3D('',#22655,#12908,#12909);
#11413=AXIS2_PLACEMENT_3D('',#22668,#12910,#12911);
#11414=AXIS2_PLACEMENT_3D('',#22681,#12912,#12913);
#11415=AXIS2_PLACEMENT_3D('',#22694,#12914,#12915);
#11416=AXIS2_PLACEMENT_3D('',#22707,#12916,#12917);
#11417=AXIS2_PLACEMENT_3D('',#22720,#12918,#12919);
#11418=AXIS2_PLACEMENT_3D('',#22733,#12920,#12921);
#11419=AXIS2_PLACEMENT_3D('',#22746,#12922,#12923);
#11420=AXIS2_PLACEMENT_3D('',#22759,#12924,#12925);
#11421=AXIS2_PLACEMENT_3D('',#22772,#12926,#12927);
#11422=AXIS2_PLACEMENT_3D('',#22785,#12928,#12929);
#11423=AXIS2_PLACEMENT_3D('',#22798,#12930,#12931);
#11424=AXIS2_PLACEMENT_3D('',#22811,#12932,#12933);
#11425=AXIS2_PLACEMENT_3D('',#22824,#12934,#12935);
#11426=AXIS2_PLACEMENT_3D('',#22837,#12936,#12937);
#11427=AXIS2_PLACEMENT_3D('',#22843,#12941,#12942);
#11428=AXIS2_PLACEMENT_3D('',#22849,#12946,#12947);
#11429=AXIS2_PLACEMENT_3D('',#22851,#12949,#12950);
#11430=AXIS2_PLACEMENT_3D('',#22853,#12952,#12953);
#11431=AXIS2_PLACEMENT_3D('',#22944,#12954,#12955);
#11432=AXIS2_PLACEMENT_3D('',#22946,#12956,#12957);
#11433=AXIS2_PLACEMENT_3D('',#22988,#12958,#12959);
#11434=AXIS2_PLACEMENT_3D('',#23025,#12960,#12961);
#11435=AXIS2_PLACEMENT_3D('',#23223,#12962,#12963);
#11436=AXIS2_PLACEMENT_3D('',#23318,#12964,#12965);
#11437=AXIS2_PLACEMENT_3D('',#23356,#12966,#12967);
#11438=AXIS2_PLACEMENT_3D('',#23357,#12968,#12969);
#11439=AXIS2_PLACEMENT_3D('',#23395,#12970,#12971);
#11440=AXIS2_PLACEMENT_3D('',#23490,#12972,#12973);
#11441=AXIS2_PLACEMENT_3D('',#23528,#12974,#12975);
#11442=AXIS2_PLACEMENT_3D('',#23529,#12976,#12977);
#11443=AXIS2_PLACEMENT_3D('',#23567,#12978,#12979);
#11444=AXIS2_PLACEMENT_3D('',#23615,#12980,#12981);
#11445=AXIS2_PLACEMENT_3D('',#23653,#12982,#12983);
#11446=AXIS2_PLACEMENT_3D('',#23654,#12984,#12985);
#11447=AXIS2_PLACEMENT_3D('',#23692,#12986,#12987);
#11448=AXIS2_PLACEMENT_3D('',#23787,#12988,#12989);
#11449=AXIS2_PLACEMENT_3D('',#23825,#12990,#12991);
#11450=AXIS2_PLACEMENT_3D('',#23826,#12992,#12993);
#11451=AXIS2_PLACEMENT_3D('',#23864,#12994,#12995);
#11452=AXIS2_PLACEMENT_3D('',#23959,#12996,#12997);
#11453=AXIS2_PLACEMENT_3D('',#23997,#12998,#12999);
#11454=AXIS2_PLACEMENT_3D('',#23998,#13000,#13001);
#11455=AXIS2_PLACEMENT_3D('',#24036,#13002,#13003);
#11456=AXIS2_PLACEMENT_3D('',#24131,#13004,#13005);
#11457=AXIS2_PLACEMENT_3D('',#24169,#13006,#13007);
#11458=AXIS2_PLACEMENT_3D('',#24170,#13008,#13009);
#11459=AXIS2_PLACEMENT_3D('',#24208,#13010,#13011);
#11460=AXIS2_PLACEMENT_3D('',#24303,#13012,#13013);
#11461=AXIS2_PLACEMENT_3D('',#24341,#13014,#13015);
#11462=AXIS2_PLACEMENT_3D('',#24342,#13016,#13017);
#11463=AXIS2_PLACEMENT_3D('',#24380,#13018,#13019);
#11464=AXIS2_PLACEMENT_3D('',#24475,#13020,#13021);
#11465=AXIS2_PLACEMENT_3D('',#24513,#13022,#13023);
#11466=AXIS2_PLACEMENT_3D('',#24514,#13024,#13025);
#11467=AXIS2_PLACEMENT_3D('',#24552,#13026,#13027);
#11468=AXIS2_PLACEMENT_3D('',#24647,#13028,#13029);
#11469=AXIS2_PLACEMENT_3D('',#24685,#13030,#13031);
#11470=AXIS2_PLACEMENT_3D('',#24686,#13032,#13033);
#11471=AXIS2_PLACEMENT_3D('',#24724,#13034,#13035);
#11472=AXIS2_PLACEMENT_3D('',#24819,#13036,#13037);
#11473=AXIS2_PLACEMENT_3D('',#24857,#13038,#13039);
#11474=AXIS2_PLACEMENT_3D('',#24858,#13040,#13041);
#11475=AXIS2_PLACEMENT_3D('',#24896,#13042,#13043);
#11476=AXIS2_PLACEMENT_3D('',#24991,#13044,#13045);
#11477=AXIS2_PLACEMENT_3D('',#25029,#13046,#13047);
#11478=AXIS2_PLACEMENT_3D('',#25030,#13048,#13049);
#11479=AXIS2_PLACEMENT_3D('',#25068,#13050,#13051);
#11480=AXIS2_PLACEMENT_3D('',#25116,#13052,#13053);
#11481=AXIS2_PLACEMENT_3D('',#25154,#13054,#13055);
#11482=AXIS2_PLACEMENT_3D('',#25155,#13056,#13057);
#11483=AXIS2_PLACEMENT_3D('',#25193,#13058,#13059);
#11484=AXIS2_PLACEMENT_3D('',#25288,#13060,#13061);
#11485=AXIS2_PLACEMENT_3D('',#25326,#13062,#13063);
#11486=AXIS2_PLACEMENT_3D('',#25327,#13064,#13065);
#11487=AXIS2_PLACEMENT_3D('',#25365,#13066,#13067);
#11488=AXIS2_PLACEMENT_3D('',#25460,#13068,#13069);
#11489=AXIS2_PLACEMENT_3D('',#25498,#13070,#13071);
#11490=AXIS2_PLACEMENT_3D('',#25499,#13072,#13073);
#11491=AXIS2_PLACEMENT_3D('',#25542,#13074,#13075);
#11492=AXIS2_PLACEMENT_3D('',#25580,#13076,#13077);
#11493=AXIS2_PLACEMENT_3D('',#25623,#13078,#13079);
#11494=AXIS2_PLACEMENT_3D('',#25624,#13080,#13081);
#11495=AXIS2_PLACEMENT_3D('',#25662,#13082,#13083);
#11496=AXIS2_PLACEMENT_3D('',#25757,#13084,#13085);
#11497=AXIS2_PLACEMENT_3D('',#25795,#13086,#13087);
#11498=AXIS2_PLACEMENT_3D('',#25796,#13088,#13089);
#11499=AXIS2_PLACEMENT_3D('',#25834,#13090,#13091);
#11500=AXIS2_PLACEMENT_3D('',#25929,#13092,#13093);
#11501=AXIS2_PLACEMENT_3D('',#25967,#13094,#13095);
#11502=AXIS2_PLACEMENT_3D('',#25968,#13096,#13097);
#11503=AXIS2_PLACEMENT_3D('',#26006,#13098,#13099);
#11504=AXIS2_PLACEMENT_3D('',#26101,#13100,#13101);
#11505=AXIS2_PLACEMENT_3D('',#26139,#13102,#13103);
#11506=AXIS2_PLACEMENT_3D('',#26140,#13104,#13105);
#11507=AXIS2_PLACEMENT_3D('',#26178,#13106,#13107);
#11508=AXIS2_PLACEMENT_3D('',#26273,#13108,#13109);
#11509=AXIS2_PLACEMENT_3D('',#26311,#13110,#13111);
#11510=AXIS2_PLACEMENT_3D('',#26312,#13112,#13113);
#11511=AXIS2_PLACEMENT_3D('',#26350,#13114,#13115);
#11512=AXIS2_PLACEMENT_3D('',#26445,#13116,#13117);
#11513=AXIS2_PLACEMENT_3D('',#26483,#13118,#13119);
#11514=AXIS2_PLACEMENT_3D('',#26484,#13120,#13121);
#11515=AXIS2_PLACEMENT_3D('',#26522,#13122,#13123);
#11516=AXIS2_PLACEMENT_3D('',#26617,#13124,#13125);
#11517=AXIS2_PLACEMENT_3D('',#26655,#13126,#13127);
#11518=AXIS2_PLACEMENT_3D('',#26656,#13128,#13129);
#11519=AXIS2_PLACEMENT_3D('',#26694,#13130,#13131);
#11520=AXIS2_PLACEMENT_3D('',#26789,#13132,#13133);
#11521=AXIS2_PLACEMENT_3D('',#26827,#13134,#13135);
#11522=AXIS2_PLACEMENT_3D('',#26828,#13136,#13137);
#11523=AXIS2_PLACEMENT_3D('',#26866,#13138,#13139);
#11524=AXIS2_PLACEMENT_3D('',#26961,#13140,#13141);
#11525=AXIS2_PLACEMENT_3D('',#26999,#13142,#13143);
#11526=AXIS2_PLACEMENT_3D('',#27000,#13144,#13145);
#11527=AXIS2_PLACEMENT_3D('',#27038,#13146,#13147);
#11528=AXIS2_PLACEMENT_3D('',#27133,#13148,#13149);
#11529=AXIS2_PLACEMENT_3D('',#27171,#13150,#13151);
#11530=AXIS2_PLACEMENT_3D('',#27172,#13152,#13153);
#11531=AXIS2_PLACEMENT_3D('',#27210,#13154,#13155);
#11532=AXIS2_PLACEMENT_3D('',#27258,#13156,#13157);
#11533=AXIS2_PLACEMENT_3D('',#27296,#13158,#13159);
#11534=AXIS2_PLACEMENT_3D('',#27297,#13160,#13161);
#11535=AXIS2_PLACEMENT_3D('',#27335,#13162,#13163);
#11536=AXIS2_PLACEMENT_3D('',#27383,#13164,#13165);
#11537=AXIS2_PLACEMENT_3D('',#27421,#13166,#13167);
#11538=AXIS2_PLACEMENT_3D('',#27422,#13168,#13169);
#11539=AXIS2_PLACEMENT_3D('',#27460,#13170,#13171);
#11540=AXIS2_PLACEMENT_3D('',#27555,#13172,#13173);
#11541=AXIS2_PLACEMENT_3D('',#27593,#13174,#13175);
#11542=AXIS2_PLACEMENT_3D('',#27594,#13176,#13177);
#11543=AXIS2_PLACEMENT_3D('',#27632,#13178,#13179);
#11544=AXIS2_PLACEMENT_3D('',#27727,#13180,#13181);
#11545=AXIS2_PLACEMENT_3D('',#27765,#13182,#13183);
#11546=AXIS2_PLACEMENT_3D('',#27766,#13184,#13185);
#11547=AXIS2_PLACEMENT_3D('',#27804,#13186,#13187);
#11548=AXIS2_PLACEMENT_3D('',#27899,#13188,#13189);
#11549=AXIS2_PLACEMENT_3D('',#27937,#13190,#13191);
#11550=AXIS2_PLACEMENT_3D('',#27938,#13192,#13193);
#11551=AXIS2_PLACEMENT_3D('',#27976,#13194,#13195);
#11552=AXIS2_PLACEMENT_3D('',#28071,#13196,#13197);
#11553=AXIS2_PLACEMENT_3D('',#28109,#13198,#13199);
#11554=AXIS2_PLACEMENT_3D('',#28110,#13200,#13201);
#11555=AXIS2_PLACEMENT_3D('',#28148,#13202,#13203);
#11556=AXIS2_PLACEMENT_3D('',#28243,#13204,#13205);
#11557=AXIS2_PLACEMENT_3D('',#28281,#13206,#13207);
#11558=AXIS2_PLACEMENT_3D('',#28282,#13208,#13209);
#11559=AXIS2_PLACEMENT_3D('',#28320,#13210,#13211);
#11560=AXIS2_PLACEMENT_3D('',#28415,#13212,#13213);
#11561=AXIS2_PLACEMENT_3D('',#28453,#13214,#13215);
#11562=AXIS2_PLACEMENT_3D('',#28454,#13216,#13217);
#11563=AXIS2_PLACEMENT_3D('',#28492,#13218,#13219);
#11564=AXIS2_PLACEMENT_3D('',#28540,#13220,#13221);
#11565=AXIS2_PLACEMENT_3D('',#28578,#13222,#13223);
#11566=AXIS2_PLACEMENT_3D('',#28579,#13224,#13225);
#11567=AXIS2_PLACEMENT_3D('',#28617,#13226,#13227);
#11568=AXIS2_PLACEMENT_3D('',#28665,#13228,#13229);
#11569=AXIS2_PLACEMENT_3D('',#28703,#13230,#13231);
#11570=AXIS2_PLACEMENT_3D('',#28704,#13232,#13233);
#11571=AXIS2_PLACEMENT_3D('',#28742,#13234,#13235);
#11572=AXIS2_PLACEMENT_3D('',#28837,#13236,#13237);
#11573=AXIS2_PLACEMENT_3D('',#28875,#13238,#13239);
#11574=AXIS2_PLACEMENT_3D('',#28876,#13240,#13241);
#11575=AXIS2_PLACEMENT_3D('',#28914,#13242,#13243);
#11576=AXIS2_PLACEMENT_3D('',#29009,#13244,#13245);
#11577=AXIS2_PLACEMENT_3D('',#29047,#13246,#13247);
#11578=AXIS2_PLACEMENT_3D('',#29048,#13248,#13249);
#11579=AXIS2_PLACEMENT_3D('',#29091,#13250,#13251);
#11580=AXIS2_PLACEMENT_3D('',#29129,#13252,#13253);
#11581=AXIS2_PLACEMENT_3D('',#29172,#13254,#13255);
#11582=AXIS2_PLACEMENT_3D('',#29173,#13256,#13257);
#11583=AXIS2_PLACEMENT_3D('',#29211,#13258,#13259);
#11584=AXIS2_PLACEMENT_3D('',#29306,#13260,#13261);
#11585=AXIS2_PLACEMENT_3D('',#29344,#13262,#13263);
#11586=AXIS2_PLACEMENT_3D('',#29345,#13264,#13265);
#11587=AXIS2_PLACEMENT_3D('',#29383,#13266,#13267);
#11588=AXIS2_PLACEMENT_3D('',#29478,#13268,#13269);
#11589=AXIS2_PLACEMENT_3D('',#29516,#13270,#13271);
#11590=AXIS2_PLACEMENT_3D('',#29517,#13272,#13273);
#11591=AXIS2_PLACEMENT_3D('',#29555,#13274,#13275);
#11592=AXIS2_PLACEMENT_3D('',#29650,#13276,#13277);
#11593=AXIS2_PLACEMENT_3D('',#29688,#13278,#13279);
#11594=AXIS2_PLACEMENT_3D('',#29689,#13280,#13281);
#11595=AXIS2_PLACEMENT_3D('',#29727,#13282,#13283);
#11596=AXIS2_PLACEMENT_3D('',#29822,#13284,#13285);
#11597=AXIS2_PLACEMENT_3D('',#29860,#13286,#13287);
#11598=AXIS2_PLACEMENT_3D('',#29861,#13288,#13289);
#11599=AXIS2_PLACEMENT_3D('',#29899,#13290,#13291);
#11600=AXIS2_PLACEMENT_3D('',#29994,#13292,#13293);
#11601=AXIS2_PLACEMENT_3D('',#30032,#13294,#13295);
#11602=AXIS2_PLACEMENT_3D('',#30033,#13296,#13297);
#11603=AXIS2_PLACEMENT_3D('',#30071,#13298,#13299);
#11604=AXIS2_PLACEMENT_3D('',#30119,#13300,#13301);
#11605=AXIS2_PLACEMENT_3D('',#30157,#13302,#13303);
#11606=AXIS2_PLACEMENT_3D('',#30158,#13304,#13305);
#11607=AXIS2_PLACEMENT_3D('',#37221,#13306,#13307);
#11608=AXIS2_PLACEMENT_3D('',#37222,#13308,#13309);
#11609=AXIS2_PLACEMENT_3D('',#37224,#13310,#13311);
#11610=AXIS2_PLACEMENT_3D('',#37227,#13313,#13314);
#11611=AXIS2_PLACEMENT_3D('',#37228,#13315,#13316);
#11612=AXIS2_PLACEMENT_3D('',#37230,#13317,#13318);
#11613=AXIS2_PLACEMENT_3D('',#37233,#13320,#13321);
#11614=AXIS2_PLACEMENT_3D('',#37234,#13322,#13323);
#11615=AXIS2_PLACEMENT_3D('',#37236,#13324,#13325);
#11616=AXIS2_PLACEMENT_3D('',#37239,#13327,#13328);
#11617=AXIS2_PLACEMENT_3D('',#37240,#13329,#13330);
#11618=AXIS2_PLACEMENT_3D('',#37242,#13331,#13332);
#11619=AXIS2_PLACEMENT_3D('',#37245,#13334,#13335);
#11620=AXIS2_PLACEMENT_3D('',#37246,#13336,#13337);
#11621=AXIS2_PLACEMENT_3D('',#37248,#13338,#13339);
#11622=AXIS2_PLACEMENT_3D('',#37251,#13341,#13342);
#11623=AXIS2_PLACEMENT_3D('',#37252,#13343,#13344);
#11624=AXIS2_PLACEMENT_3D('',#37254,#13345,#13346);
#11625=AXIS2_PLACEMENT_3D('',#37257,#13348,#13349);
#11626=AXIS2_PLACEMENT_3D('',#37258,#13350,#13351);
#11627=AXIS2_PLACEMENT_3D('',#37260,#13352,#13353);
#11628=AXIS2_PLACEMENT_3D('',#37263,#13355,#13356);
#11629=AXIS2_PLACEMENT_3D('',#37264,#13357,#13358);
#11630=AXIS2_PLACEMENT_3D('',#37266,#13359,#13360);
#11631=AXIS2_PLACEMENT_3D('',#37269,#13362,#13363);
#11632=AXIS2_PLACEMENT_3D('',#37270,#13364,#13365);
#11633=AXIS2_PLACEMENT_3D('',#37272,#13366,#13367);
#11634=AXIS2_PLACEMENT_3D('',#37275,#13369,#13370);
#11635=AXIS2_PLACEMENT_3D('',#37276,#13371,#13372);
#11636=AXIS2_PLACEMENT_3D('',#37278,#13373,#13374);
#11637=AXIS2_PLACEMENT_3D('',#37281,#13376,#13377);
#11638=AXIS2_PLACEMENT_3D('',#37282,#13378,#13379);
#11639=AXIS2_PLACEMENT_3D('',#37284,#13380,#13381);
#11640=AXIS2_PLACEMENT_3D('',#37287,#13383,#13384);
#11641=AXIS2_PLACEMENT_3D('',#37288,#13385,#13386);
#11642=AXIS2_PLACEMENT_3D('',#37290,#13387,#13388);
#11643=AXIS2_PLACEMENT_3D('',#37293,#13390,#13391);
#11644=AXIS2_PLACEMENT_3D('',#37294,#13392,#13393);
#11645=AXIS2_PLACEMENT_3D('',#37296,#13394,#13395);
#11646=AXIS2_PLACEMENT_3D('',#37299,#13397,#13398);
#11647=AXIS2_PLACEMENT_3D('',#37300,#13399,#13400);
#11648=AXIS2_PLACEMENT_3D('',#37317,#13409,#13410);
#11649=AXIS2_PLACEMENT_3D('',#37326,#13415,#13416);
#11650=AXIS2_PLACEMENT_3D('',#37335,#13421,#13422);
#11651=AXIS2_PLACEMENT_3D('',#37344,#13427,#13428);
#11652=AXIS2_PLACEMENT_3D('',#37353,#13433,#13434);
#11653=AXIS2_PLACEMENT_3D('',#37356,#13436,#13437);
#11654=AXIS2_PLACEMENT_3D('',#37357,#13438,#13439);
#11655=AXIS2_PLACEMENT_3D('',#37359,#13440,#13441);
#11656=AXIS2_PLACEMENT_3D('',#37365,#13445,#13446);
#11657=AXIS2_PLACEMENT_3D('',#37379,#13454,#13455);
#11658=AXIS2_PLACEMENT_3D('',#37382,#13457,#13458);
#11659=AXIS2_PLACEMENT_3D('',#37383,#13459,#13460);
#11660=AXIS2_PLACEMENT_3D('',#37384,#13461,#13462);
#11661=AXIS2_PLACEMENT_3D('',#37388,#13465,#13466);
#11662=AXIS2_PLACEMENT_3D('',#37390,#13468,#13469);
#11663=AXIS2_PLACEMENT_3D('',#37392,#13471,#13472);
#11664=AXIS2_PLACEMENT_3D('',#37393,#13473,#13474);
#11665=AXIS2_PLACEMENT_3D('',#37399,#13478,#13479);
#11666=AXIS2_PLACEMENT_3D('',#37400,#13480,#13481);
#11667=AXIS2_PLACEMENT_3D('',#37401,#13482,#13483);
#11668=AXIS2_PLACEMENT_3D('',#37405,#13486,#13487);
#11669=AXIS2_PLACEMENT_3D('',#37406,#13488,#13489);
#11670=AXIS2_PLACEMENT_3D('',#37407,#13490,#13491);
#11671=AXIS2_PLACEMENT_3D('',#37408,#13492,#13493);
#11672=AXIS2_PLACEMENT_3D('',#37412,#13496,#13497);
#11673=AXIS2_PLACEMENT_3D('',#37414,#13499,#13500);
#11674=AXIS2_PLACEMENT_3D('',#37415,#13501,#13502);
#11675=AXIS2_PLACEMENT_3D('',#37424,#13507,#13508);
#11676=AXIS2_PLACEMENT_3D('',#37425,#13509,#13510);
#11677=AXIS2_PLACEMENT_3D('',#37426,#13511,#13512);
#11678=AXIS2_PLACEMENT_3D('',#37427,#13513,#13514);
#11679=AXIS2_PLACEMENT_3D('',#37428,#13515,#13516);
#11680=AXIS2_PLACEMENT_3D('',#37429,#13517,#13518);
#11681=AXIS2_PLACEMENT_3D('',#37430,#13519,#13520);
#11682=AXIS2_PLACEMENT_3D('',#37431,#13521,#13522);
#11683=AXIS2_PLACEMENT_3D('',#37432,#13523,#13524);
#11684=AXIS2_PLACEMENT_3D('',#37433,#13525,#13526);
#11685=AXIS2_PLACEMENT_3D('',#37434,#13527,#13528);
#11686=AXIS2_PLACEMENT_3D('',#37435,#13529,#13530);
#11687=AXIS2_PLACEMENT_3D('',#37436,#13531,#13532);
#11688=AXIS2_PLACEMENT_3D('',#37437,#13533,#13534);
#11689=AXIS2_PLACEMENT_3D('',#37438,#13535,#13536);
#11690=AXIS2_PLACEMENT_3D('',#37439,#13537,#13538);
#11691=AXIS2_PLACEMENT_3D('',#37448,#13543,#13544);
#11692=AXIS2_PLACEMENT_3D('',#37457,#13549,#13550);
#11693=AXIS2_PLACEMENT_3D('',#37466,#13555,#13556);
#11694=AXIS2_PLACEMENT_3D('',#37475,#13561,#13562);
#11695=AXIS2_PLACEMENT_3D('',#37484,#13567,#13568);
#11696=AXIS2_PLACEMENT_3D('',#37493,#13573,#13574);
#11697=AXIS2_PLACEMENT_3D('',#37494,#13575,#13576);
#11698=AXIS2_PLACEMENT_3D('',#37495,#13577,#13578);
#11699=AXIS2_PLACEMENT_3D('',#37496,#13579,#13580);
#11700=AXIS2_PLACEMENT_3D('',#37497,#13581,#13582);
#11701=AXIS2_PLACEMENT_3D('',#37498,#13583,#13584);
#11702=AXIS2_PLACEMENT_3D('',#37499,#13585,#13586);
#11703=AXIS2_PLACEMENT_3D('',#37500,#13587,#13588);
#11704=AXIS2_PLACEMENT_3D('',#37501,#13589,#13590);
#11705=AXIS2_PLACEMENT_3D('',#37502,#13591,#13592);
#11706=AXIS2_PLACEMENT_3D('',#37503,#13593,#13594);
#11707=AXIS2_PLACEMENT_3D('',#37504,#13595,#13596);
#11708=AXIS2_PLACEMENT_3D('',#37505,#13597,#13598);
#11709=AXIS2_PLACEMENT_3D('',#37506,#13599,#13600);
#11710=AXIS2_PLACEMENT_3D('',#37507,#13601,#13602);
#11711=AXIS2_PLACEMENT_3D('',#37508,#13603,#13604);
#11712=AXIS2_PLACEMENT_3D('',#37509,#13605,#13606);
#11713=AXIS2_PLACEMENT_3D('',#37510,#13607,#13608);
#11714=AXIS2_PLACEMENT_3D('',#37511,#13609,#13610);
#11715=AXIS2_PLACEMENT_3D('',#37512,#13611,#13612);
#11716=AXIS2_PLACEMENT_3D('',#37513,#13613,#13614);
#11717=AXIS2_PLACEMENT_3D('',#37514,#13615,#13616);
#11718=AXIS2_PLACEMENT_3D('',#37515,#13617,#13618);
#11719=AXIS2_PLACEMENT_3D('',#37516,#13619,#13620);
#11720=AXIS2_PLACEMENT_3D('',#37517,#13621,#13622);
#11721=AXIS2_PLACEMENT_3D('',#37518,#13623,#13624);
#11722=AXIS2_PLACEMENT_3D('',#37519,#13625,#13626);
#11723=AXIS2_PLACEMENT_3D('',#37520,#13627,#13628);
#11724=AXIS2_PLACEMENT_3D('',#37521,#13629,#13630);
#11725=AXIS2_PLACEMENT_3D('',#37522,#13631,#13632);
#11726=AXIS2_PLACEMENT_3D('',#37523,#13633,#13634);
#11727=AXIS2_PLACEMENT_3D('',#37524,#13635,#13636);
#11728=AXIS2_PLACEMENT_3D('',#37525,#13637,#13638);
#11729=AXIS2_PLACEMENT_3D('',#37526,#13639,#13640);
#11730=AXIS2_PLACEMENT_3D('',#37527,#13641,#13642);
#11731=AXIS2_PLACEMENT_3D('',#37528,#13643,#13644);
#11732=AXIS2_PLACEMENT_3D('',#37529,#13645,#13646);
#11733=AXIS2_PLACEMENT_3D('',#37530,#13647,#13648);
#11734=AXIS2_PLACEMENT_3D('',#37531,#13649,#13650);
#11735=AXIS2_PLACEMENT_3D('',#37532,#13651,#13652);
#11736=AXIS2_PLACEMENT_3D('',#37533,#13653,#13654);
#11737=AXIS2_PLACEMENT_3D('',#37534,#13655,#13656);
#11738=AXIS2_PLACEMENT_3D('',#37535,#13657,#13658);
#11739=AXIS2_PLACEMENT_3D('',#37536,#13659,#13660);
#11740=AXIS2_PLACEMENT_3D('',#37537,#13661,#13662);
#11741=AXIS2_PLACEMENT_3D('',#37538,#13663,#13664);
#11742=AXIS2_PLACEMENT_3D('',#37540,#13665,#13666);
#11743=AXIS2_PLACEMENT_3D('',#37543,#13668,#13669);
#11744=AXIS2_PLACEMENT_3D('',#37544,#13670,#13671);
#11745=AXIS2_PLACEMENT_3D('',#37546,#13672,#13673);
#11746=AXIS2_PLACEMENT_3D('',#37549,#13675,#13676);
#11747=AXIS2_PLACEMENT_3D('',#37550,#13677,#13678);
#11748=AXIS2_PLACEMENT_3D('',#37552,#13679,#13680);
#11749=AXIS2_PLACEMENT_3D('',#37555,#13682,#13683);
#11750=AXIS2_PLACEMENT_3D('',#37556,#13684,#13685);
#11751=AXIS2_PLACEMENT_3D('',#37558,#13686,#13687);
#11752=AXIS2_PLACEMENT_3D('',#37561,#13689,#13690);
#11753=AXIS2_PLACEMENT_3D('',#37562,#13691,#13692);
#11754=AXIS2_PLACEMENT_3D('',#37564,#13693,#13694);
#11755=AXIS2_PLACEMENT_3D('',#37567,#13696,#13697);
#11756=AXIS2_PLACEMENT_3D('',#37568,#13698,#13699);
#11757=AXIS2_PLACEMENT_3D('',#37570,#13700,#13701);
#11758=AXIS2_PLACEMENT_3D('',#37573,#13703,#13704);
#11759=AXIS2_PLACEMENT_3D('',#37574,#13705,#13706);
#11760=AXIS2_PLACEMENT_3D('',#37576,#13707,#13708);
#11761=AXIS2_PLACEMENT_3D('',#37579,#13710,#13711);
#11762=AXIS2_PLACEMENT_3D('',#37580,#13712,#13713);
#11763=AXIS2_PLACEMENT_3D('',#37582,#13714,#13715);
#11764=AXIS2_PLACEMENT_3D('',#37585,#13717,#13718);
#11765=AXIS2_PLACEMENT_3D('',#37586,#13719,#13720);
#11766=AXIS2_PLACEMENT_3D('',#37587,#13721,#13722);
#11767=AXIS2_PLACEMENT_3D('',#37588,#13723,#13724);
#11768=AXIS2_PLACEMENT_3D('',#37589,#13725,#13726);
#11769=AXIS2_PLACEMENT_3D('',#37591,#13727,#13728);
#11770=AXIS2_PLACEMENT_3D('',#37594,#13730,#13731);
#11771=AXIS2_PLACEMENT_3D('',#37595,#13732,#13733);
#11772=AXIS2_PLACEMENT_3D('',#37597,#13734,#13735);
#11773=AXIS2_PLACEMENT_3D('',#37600,#13737,#13738);
#11774=AXIS2_PLACEMENT_3D('',#37601,#13739,#13740);
#11775=AXIS2_PLACEMENT_3D('',#37603,#13741,#13742);
#11776=AXIS2_PLACEMENT_3D('',#37606,#13744,#13745);
#11777=AXIS2_PLACEMENT_3D('',#37607,#13746,#13747);
#11778=AXIS2_PLACEMENT_3D('',#37609,#13748,#13749);
#11779=AXIS2_PLACEMENT_3D('',#37612,#13751,#13752);
#11780=AXIS2_PLACEMENT_3D('',#37613,#13753,#13754);
#11781=AXIS2_PLACEMENT_3D('',#37615,#13755,#13756);
#11782=AXIS2_PLACEMENT_3D('',#37618,#13758,#13759);
#11783=AXIS2_PLACEMENT_3D('',#37619,#13760,#13761);
#11784=AXIS2_PLACEMENT_3D('',#37621,#13762,#13763);
#11785=AXIS2_PLACEMENT_3D('',#37624,#13765,#13766);
#11786=AXIS2_PLACEMENT_3D('',#37625,#13767,#13768);
#11787=AXIS2_PLACEMENT_3D('',#37627,#13769,#13770);
#11788=AXIS2_PLACEMENT_3D('',#37630,#13772,#13773);
#11789=AXIS2_PLACEMENT_3D('',#37631,#13774,#13775);
#11790=AXIS2_PLACEMENT_3D('',#37633,#13776,#13777);
#11791=AXIS2_PLACEMENT_3D('',#37636,#13779,#13780);
#11792=AXIS2_PLACEMENT_3D('',#37637,#13781,#13782);
#11793=AXIS2_PLACEMENT_3D('',#37638,#13783,#13784);
#11794=AXIS2_PLACEMENT_3D('',#37639,#13785,#13786);
#11795=AXIS2_PLACEMENT_3D('',#37640,#13787,#13788);
#11796=AXIS2_PLACEMENT_3D('',#37642,#13789,#13790);
#11797=AXIS2_PLACEMENT_3D('',#37645,#13792,#13793);
#11798=AXIS2_PLACEMENT_3D('',#37646,#13794,#13795);
#11799=AXIS2_PLACEMENT_3D('',#37648,#13796,#13797);
#11800=AXIS2_PLACEMENT_3D('',#37650,#13798,#13799);
#11801=AXIS2_PLACEMENT_3D('',#37652,#13800,#13801);
#11802=AXIS2_PLACEMENT_3D('',#37653,#13802,#13803);
#11803=AXIS2_PLACEMENT_3D('',#37654,#13804,#13805);
#11804=AXIS2_PLACEMENT_3D('',#37656,#13806,#13807);
#11805=AXIS2_PLACEMENT_3D('',#37658,#13809,#13810);
#11806=AXIS2_PLACEMENT_3D('',#37660,#13811,#13812);
#11807=AXIS2_PLACEMENT_3D('',#37662,#13814,#13815);
#11808=AXIS2_PLACEMENT_3D('',#37663,#13816,#13817);
#11809=AXIS2_PLACEMENT_3D('',#37664,#13818,#13819);
#11810=AXIS2_PLACEMENT_3D('',#37665,#13820,#13821);
#11811=AXIS2_PLACEMENT_3D('',#37666,#13822,#13823);
#11812=AXIS2_PLACEMENT_3D('',#37668,#13824,#13825);
#11813=AXIS2_PLACEMENT_3D('',#37671,#13827,#13828);
#11814=AXIS2_PLACEMENT_3D('',#37672,#13829,#13830);
#11815=AXIS2_PLACEMENT_3D('',#37681,#13835,#13836);
#11816=AXIS2_PLACEMENT_3D('',#37687,#13840,#13841);
#11817=AXIS2_PLACEMENT_3D('',#37693,#13845,#13846);
#11818=AXIS2_PLACEMENT_3D('',#37699,#13850,#13851);
#11819=AXIS2_PLACEMENT_3D('',#37705,#13855,#13856);
#11820=AXIS2_PLACEMENT_3D('',#37708,#13859,#13860);
#11821=AXIS2_PLACEMENT_3D('',#37709,#13861,#13862);
#11822=AXIS2_PLACEMENT_3D('',#37710,#13863,#13864);
#11823=AXIS2_PLACEMENT_3D('',#37711,#13865,#13866);
#11824=AXIS2_PLACEMENT_3D('',#37712,#13867,#13868);
#11825=AXIS2_PLACEMENT_3D('',#37721,#13873,#13874);
#11826=AXIS2_PLACEMENT_3D('',#37730,#13879,#13880);
#11827=AXIS2_PLACEMENT_3D('',#37739,#13885,#13886);
#11828=AXIS2_PLACEMENT_3D('',#37748,#13891,#13892);
#11829=AXIS2_PLACEMENT_3D('',#37754,#13896,#13897);
#11830=AXIS2_PLACEMENT_3D('',#37760,#13901,#13902);
#11831=AXIS2_PLACEMENT_3D('',#37769,#13907,#13908);
#11832=AXIS2_PLACEMENT_3D('',#37778,#13913,#13914);
#11833=AXIS2_PLACEMENT_3D('',#37785,#13921,#13922);
#11834=AXIS2_PLACEMENT_3D('',#37792,#13929,#13930);
#11835=AXIS2_PLACEMENT_3D('',#37793,#13931,#13932);
#11836=AXIS2_PLACEMENT_3D('',#37794,#13933,#13934);
#11837=AXIS2_PLACEMENT_3D('',#37795,#13935,#13936);
#11838=AXIS2_PLACEMENT_3D('',#37796,#13937,#13938);
#11839=AXIS2_PLACEMENT_3D('',#37797,#13939,#13940);
#11840=AXIS2_PLACEMENT_3D('',#37798,#13941,#13942);
#11841=AXIS2_PLACEMENT_3D('',#37799,#13943,#13944);
#11842=AXIS2_PLACEMENT_3D('',#37801,#13945,#13946);
#11843=AXIS2_PLACEMENT_3D('',#37804,#13948,#13949);
#11844=AXIS2_PLACEMENT_3D('',#37805,#13950,#13951);
#11845=AXIS2_PLACEMENT_3D('',#37807,#13952,#13953);
#11846=AXIS2_PLACEMENT_3D('',#37810,#13955,#13956);
#11847=AXIS2_PLACEMENT_3D('',#37811,#13957,#13958);
#11848=AXIS2_PLACEMENT_3D('',#37812,#13959,#13960);
#11849=AXIS2_PLACEMENT_3D('',#37813,#13961,#13962);
#11850=AXIS2_PLACEMENT_3D('',#37814,#13963,#13964);
#11851=AXIS2_PLACEMENT_3D('',#37815,#13965,#13966);
#11852=AXIS2_PLACEMENT_3D('',#37816,#13967,#13968);
#11853=AXIS2_PLACEMENT_3D('',#37817,#13969,#13970);
#11854=AXIS2_PLACEMENT_3D('',#37818,#13971,#13972);
#11855=AXIS2_PLACEMENT_3D('',#37819,#13973,#13974);
#11856=AXIS2_PLACEMENT_3D('',#37820,#13975,#13976);
#11857=AXIS2_PLACEMENT_3D('',#37821,#13977,#13978);
#11858=AXIS2_PLACEMENT_3D('',#37822,#13979,#13980);
#11859=AXIS2_PLACEMENT_3D('',#37823,#13981,#13982);
#11860=AXIS2_PLACEMENT_3D('',#37824,#13983,#13984);
#11861=AXIS2_PLACEMENT_3D('',#37825,#13985,#13986);
#11862=AXIS2_PLACEMENT_3D('',#37826,#13987,#13988);
#11863=AXIS2_PLACEMENT_3D('',#37827,#13989,#13990);
#11864=AXIS2_PLACEMENT_3D('',#37828,#13991,#13992);
#11865=AXIS2_PLACEMENT_3D('',#37829,#13993,#13994);
#11866=AXIS2_PLACEMENT_3D('',#37830,#13995,#13996);
#11867=AXIS2_PLACEMENT_3D('',#37831,#13997,#13998);
#11868=AXIS2_PLACEMENT_3D('',#37832,#13999,#14000);
#11869=AXIS2_PLACEMENT_3D('',#37833,#14001,#14002);
#11870=AXIS2_PLACEMENT_3D('',#37834,#14003,#14004);
#11871=AXIS2_PLACEMENT_3D('',#37835,#14005,#14006);
#11872=AXIS2_PLACEMENT_3D('',#37836,#14007,#14008);
#11873=AXIS2_PLACEMENT_3D('',#37837,#14009,#14010);
#11874=AXIS2_PLACEMENT_3D('',#37838,#14011,#14012);
#11875=AXIS2_PLACEMENT_3D('',#37839,#14013,#14014);
#11876=AXIS2_PLACEMENT_3D('',#37840,#14015,#14016);
#11877=AXIS2_PLACEMENT_3D('',#37841,#14017,#14018);
#11878=AXIS2_PLACEMENT_3D('',#37842,#14019,#14020);
#11879=AXIS2_PLACEMENT_3D('',#37843,#14021,#14022);
#11880=AXIS2_PLACEMENT_3D('',#37844,#14023,#14024);
#11881=AXIS2_PLACEMENT_3D('',#37845,#14025,#14026);
#11882=AXIS2_PLACEMENT_3D('',#37846,#14027,#14028);
#11883=AXIS2_PLACEMENT_3D('',#37847,#14029,#14030);
#11884=AXIS2_PLACEMENT_3D('',#37848,#14031,#14032);
#11885=AXIS2_PLACEMENT_3D('',#37849,#14033,#14034);
#11886=AXIS2_PLACEMENT_3D('',#37850,#14035,#14036);
#11887=AXIS2_PLACEMENT_3D('',#37851,#14037,#14038);
#11888=AXIS2_PLACEMENT_3D('',#37852,#14039,#14040);
#11889=AXIS2_PLACEMENT_3D('',#37853,#14041,#14042);
#11890=DIRECTION('axis',(0.,0.,1.));
#11891=DIRECTION('refdir',(1.,0.,0.));
#11892=DIRECTION('axis',(0.,0.,1.));
#11893=DIRECTION('refdir',(1.,0.,0.));
#11894=DIRECTION('center_axis',(1.,0.,0.));
#11895=DIRECTION('ref_axis',(0.,0.,-1.));
#11896=DIRECTION('center_axis',(-1.,0.,0.));
#11897=DIRECTION('ref_axis',(0.,0.,1.));
#11898=DIRECTION('',(1.,0.,0.));
#11899=DIRECTION('center_axis',(1.,0.,0.));
#11900=DIRECTION('ref_axis',(0.,0.,-1.));
#11901=DIRECTION('center_axis',(1.,0.,0.));
#11902=DIRECTION('ref_axis',(0.,0.,-1.));
#11903=DIRECTION('center_axis',(-1.,0.,0.));
#11904=DIRECTION('ref_axis',(0.,0.,1.));
#11905=DIRECTION('',(1.,0.,0.));
#11906=DIRECTION('center_axis',(1.,0.,0.));
#11907=DIRECTION('ref_axis',(0.,0.,-1.));
#11908=DIRECTION('center_axis',(1.,0.,0.));
#11909=DIRECTION('ref_axis',(0.,0.,-1.));
#11910=DIRECTION('center_axis',(1.,0.,0.));
#11911=DIRECTION('ref_axis',(0.,0.,-1.));
#11912=DIRECTION('',(1.,0.,0.));
#11913=DIRECTION('center_axis',(1.,0.,0.));
#11914=DIRECTION('ref_axis',(0.,0.,-1.));
#11915=DIRECTION('center_axis',(1.,0.,0.));
#11916=DIRECTION('ref_axis',(0.,0.,-1.));
#11917=DIRECTION('center_axis',(1.,0.,0.));
#11918=DIRECTION('ref_axis',(0.,0.,-1.));
#11919=DIRECTION('',(1.,0.,0.));
#11920=DIRECTION('center_axis',(1.,0.,0.));
#11921=DIRECTION('ref_axis',(0.,0.,-1.));
#11922=DIRECTION('center_axis',(0.,0.,1.));
#11923=DIRECTION('ref_axis',(1.,0.,0.));
#11924=DIRECTION('center_axis',(0.,0.,1.));
#11925=DIRECTION('ref_axis',(1.,0.,0.));
#11926=DIRECTION('',(0.,0.,1.));
#11927=DIRECTION('center_axis',(0.,0.,1.));
#11928=DIRECTION('ref_axis',(1.,0.,0.));
#11929=DIRECTION('center_axis',(0.,0.,1.));
#11930=DIRECTION('ref_axis',(1.,0.,0.));
#11931=DIRECTION('center_axis',(0.,0.,1.));
#11932=DIRECTION('ref_axis',(1.,0.,0.));
#11933=DIRECTION('',(0.,0.,1.));
#11934=DIRECTION('center_axis',(0.,0.,1.));
#11935=DIRECTION('ref_axis',(1.,0.,0.));
#11936=DIRECTION('center_axis',(0.,0.,1.));
#11937=DIRECTION('ref_axis',(1.,0.,0.));
#11938=DIRECTION('center_axis',(0.,0.,1.));
#11939=DIRECTION('ref_axis',(1.,0.,0.));
#11940=DIRECTION('',(0.,0.,1.));
#11941=DIRECTION('center_axis',(0.,0.,1.));
#11942=DIRECTION('ref_axis',(1.,0.,0.));
#11943=DIRECTION('center_axis',(0.,0.,1.));
#11944=DIRECTION('ref_axis',(1.,0.,0.));
#11945=DIRECTION('center_axis',(0.,0.,1.));
#11946=DIRECTION('ref_axis',(1.,0.,0.));
#11947=DIRECTION('',(0.,0.,1.));
#11948=DIRECTION('center_axis',(0.,0.,1.));
#11949=DIRECTION('ref_axis',(1.,0.,0.));
#11950=DIRECTION('center_axis',(0.,0.,1.));
#11951=DIRECTION('ref_axis',(1.,0.,0.));
#11952=DIRECTION('center_axis',(0.,0.,1.));
#11953=DIRECTION('ref_axis',(1.,0.,0.));
#11954=DIRECTION('',(0.,0.,1.));
#11955=DIRECTION('center_axis',(0.,0.,1.));
#11956=DIRECTION('ref_axis',(1.,0.,0.));
#11957=DIRECTION('center_axis',(0.,0.,1.));
#11958=DIRECTION('ref_axis',(1.,0.,0.));
#11959=DIRECTION('center_axis',(0.,0.,1.));
#11960=DIRECTION('ref_axis',(1.,0.,0.));
#11961=DIRECTION('',(0.,0.,1.));
#11962=DIRECTION('center_axis',(0.,0.,1.));
#11963=DIRECTION('ref_axis',(1.,0.,0.));
#11964=DIRECTION('center_axis',(0.,0.,1.));
#11965=DIRECTION('ref_axis',(1.,0.,0.));
#11966=DIRECTION('center_axis',(0.,0.,1.));
#11967=DIRECTION('ref_axis',(1.,0.,0.));
#11968=DIRECTION('',(0.,0.,1.));
#11969=DIRECTION('center_axis',(0.,0.,1.));
#11970=DIRECTION('ref_axis',(1.,0.,0.));
#11971=DIRECTION('center_axis',(0.,0.,-1.));
#11972=DIRECTION('ref_axis',(-1.,0.,0.));
#11973=DIRECTION('',(1.,0.,0.));
#11974=DIRECTION('',(0.,-1.,0.));
#11975=DIRECTION('',(-1.,0.,0.));
#11976=DIRECTION('',(0.,1.,0.));
#11977=DIRECTION('',(1.,0.,0.));
#11978=DIRECTION('',(0.,1.,0.));
#11979=DIRECTION('',(-1.,0.,0.));
#11980=DIRECTION('',(0.,-1.,0.));
#11981=DIRECTION('center_axis',(0.,0.,-1.));
#11982=DIRECTION('ref_axis',(-1.,0.,0.));
#11983=DIRECTION('',(-1.,0.,0.));
#11984=DIRECTION('',(0.,1.,0.));
#11985=DIRECTION('',(1.,0.,0.));
#11986=DIRECTION('',(0.,1.,0.));
#11987=DIRECTION('center_axis',(0.,0.,-1.));
#11988=DIRECTION('ref_axis',(-1.,0.,0.));
#11989=DIRECTION('',(1.,0.,0.));
#11990=DIRECTION('',(0.,1.,0.));
#11991=DIRECTION('',(-1.,0.,0.));
#11992=DIRECTION('',(0.,1.,0.));
#11993=DIRECTION('center_axis',(0.,0.,-1.));
#11994=DIRECTION('ref_axis',(-1.,0.,0.));
#11995=DIRECTION('',(1.,0.,0.));
#11996=DIRECTION('',(0.,-1.,0.));
#11997=DIRECTION('',(-1.,0.,0.));
#11998=DIRECTION('',(0.,-1.,0.));
#11999=DIRECTION('center_axis',(0.,0.,-1.));
#12000=DIRECTION('ref_axis',(-1.,0.,0.));
#12001=DIRECTION('',(-1.,0.,0.));
#12002=DIRECTION('',(0.,-1.,0.));
#12003=DIRECTION('',(1.,0.,0.));
#12004=DIRECTION('',(0.,-1.,0.));
#12005=DIRECTION('center_axis',(-1.,0.,0.));
#12006=DIRECTION('ref_axis',(0.,0.,1.));
#12007=DIRECTION('',(0.,0.,-1.));
#12008=DIRECTION('',(0.,-1.,0.));
#12009=DIRECTION('',(0.,0.,-1.));
#12010=DIRECTION('',(0.,1.,0.));
#12011=DIRECTION('center_axis',(1.,0.,0.));
#12012=DIRECTION('ref_axis',(0.,0.,-1.));
#12013=DIRECTION('center_axis',(1.,0.,0.));
#12014=DIRECTION('ref_axis',(0.,0.,-1.));
#12015=DIRECTION('center_axis',(1.,0.,0.));
#12016=DIRECTION('ref_axis',(0.,0.,-1.));
#12017=DIRECTION('center_axis',(0.,0.,-1.));
#12018=DIRECTION('ref_axis',(-1.,0.,0.));
#12019=DIRECTION('',(-1.,0.,0.));
#12020=DIRECTION('',(1.,0.,0.));
#12021=DIRECTION('',(0.,-1.,0.));
#12022=DIRECTION('',(-1.,0.,0.));
#12023=DIRECTION('',(0.,-1.,0.));
#12024=DIRECTION('',(1.,-1.33440267382831E-16,0.));
#12025=DIRECTION('',(0.,1.,0.));
#12026=DIRECTION('center_axis',(1.,0.,0.));
#12027=DIRECTION('ref_axis',(0.,0.,-1.));
#12028=DIRECTION('',(0.,0.,-1.));
#12029=DIRECTION('',(0.,1.,0.));
#12030=DIRECTION('',(0.,0.,-1.));
#12031=DIRECTION('center_axis',(1.,0.,0.));
#12032=DIRECTION('ref_axis',(0.,0.,-1.));
#12033=DIRECTION('center_axis',(1.,0.,0.));
#12034=DIRECTION('ref_axis',(0.,0.,-1.));
#12035=DIRECTION('center_axis',(1.,0.,0.));
#12036=DIRECTION('ref_axis',(0.,0.,-1.));
#12037=DIRECTION('center_axis',(0.,1.,0.));
#12038=DIRECTION('ref_axis',(0.,0.,1.));
#12039=DIRECTION('',(-1.,0.,0.));
#12040=DIRECTION('center_axis',(0.,-1.,0.));
#12041=DIRECTION('ref_axis',(0.,0.,-1.));
#12042=DIRECTION('',(1.,0.,0.));
#12043=DIRECTION('center_axis',(-1.,0.,0.));
#12044=DIRECTION('ref_axis',(0.,0.,1.));
#12045=DIRECTION('center_axis',(-1.,0.,0.));
#12046=DIRECTION('ref_axis',(0.,0.,1.));
#12047=DIRECTION('center_axis',(-1.,0.,0.));
#12048=DIRECTION('ref_axis',(0.,0.,1.));
#12049=DIRECTION('center_axis',(-1.,0.,0.));
#12050=DIRECTION('ref_axis',(0.,0.,1.));
#12051=DIRECTION('',(0.,0.,-1.));
#12052=DIRECTION('',(0.,1.,0.));
#12053=DIRECTION('',(0.,0.,-1.));
#12054=DIRECTION('center_axis',(0.,-1.,0.));
#12055=DIRECTION('ref_axis',(0.,0.,-1.));
#12056=DIRECTION('',(-1.,0.,0.));
#12057=DIRECTION('',(0.,0.,-1.));
#12058=DIRECTION('center_axis',(1.,0.,0.));
#12059=DIRECTION('ref_axis',(0.,0.,-1.));
#12060=DIRECTION('center_axis',(1.,0.,0.));
#12061=DIRECTION('ref_axis',(0.,0.,-1.));
#12062=DIRECTION('',(0.,-1.,0.));
#12063=DIRECTION('',(0.,0.,-1.));
#12064=DIRECTION('center_axis',(1.,0.,0.));
#12065=DIRECTION('ref_axis',(0.,0.,-1.));
#12066=DIRECTION('center_axis',(1.,0.,0.));
#12067=DIRECTION('ref_axis',(0.,0.,-1.));
#12068=DIRECTION('center_axis',(1.33440267382831E-16,1.,0.));
#12069=DIRECTION('ref_axis',(-1.,1.33440267382831E-16,0.));
#12070=DIRECTION('',(1.,-1.33440267382831E-16,0.));
#12071=DIRECTION('center_axis',(0.,0.,1.));
#12072=DIRECTION('ref_axis',(1.,0.,0.));
#12073=DIRECTION('center_axis',(0.,0.,1.));
#12074=DIRECTION('ref_axis',(1.,0.,0.));
#12075=DIRECTION('',(-1.,0.,0.));
#12076=DIRECTION('',(0.,-1.,0.));
#12077=DIRECTION('',(1.,0.,0.));
#12078=DIRECTION('',(0.,1.,0.));
#12079=DIRECTION('center_axis',(1.,0.,0.));
#12080=DIRECTION('ref_axis',(0.,1.22464679914735E-16,1.));
#12081=DIRECTION('center_axis',(1.,0.,0.));
#12082=DIRECTION('ref_axis',(0.,1.22464679914735E-16,1.));
#12083=DIRECTION('center_axis',(1.,0.,0.));
#12084=DIRECTION('ref_axis',(0.,1.22464679914735E-16,1.));
#12085=DIRECTION('center_axis',(1.,0.,0.));
#12086=DIRECTION('ref_axis',(0.,1.22464679914735E-16,1.));
#12087=DIRECTION('center_axis',(1.,0.,0.));
#12088=DIRECTION('ref_axis',(0.,1.22464679914735E-16,1.));
#12089=DIRECTION('center_axis',(1.,0.,0.));
#12090=DIRECTION('ref_axis',(0.,1.22464679914735E-16,1.));
#12091=DIRECTION('center_axis',(0.,-1.,0.));
#12092=DIRECTION('ref_axis',(0.,0.,-1.));
#12093=DIRECTION('center_axis',(-0.707106781186549,-0.707106781186546,-1.50457204420145E-15));
#12094=DIRECTION('ref_axis',(0.707106781186546,-0.707106781186549,-9.86517477994685E-14));
#12095=DIRECTION('center_axis',(-0.707106781186548,0.707106781186548,0.));
#12096=DIRECTION('ref_axis',(0.707106781186548,0.707106781186548,-2.92621452477431E-13));
#12097=DIRECTION('center_axis',(1.,0.,0.));
#12098=DIRECTION('ref_axis',(0.,0.,-1.));
#12099=DIRECTION('center_axis',(-0.70710678118655,-0.707106781186545,5.06083323958671E-15));
#12100=DIRECTION('ref_axis',(0.707106781186545,-0.70710678118655,1.41538849381609E-13));
#12101=DIRECTION('center_axis',(-1.,0.,0.));
#12102=DIRECTION('ref_axis',(0.,0.,1.));
#12103=DIRECTION('center_axis',(-0.707106781186552,0.707106781186543,6.56540528378815E-15));
#12104=DIRECTION('ref_axis',(0.707106781186543,0.707106781186552,2.52973120306771E-13));
#12105=DIRECTION('center_axis',(0.,1.,0.));
#12106=DIRECTION('ref_axis',(0.,0.,1.));
#12107=DIRECTION('axis',(0.,0.,1.));
#12108=DIRECTION('refdir',(1.,0.,0.));
#12109=DIRECTION('center_axis',(1.,1.34590614515444E-16,0.));
#12110=DIRECTION('ref_axis',(-1.34590614515444E-16,1.,0.));
#12111=DIRECTION('',(-1.,-1.34590614515444E-16,0.));
#12112=DIRECTION('',(-1.,-1.34590614515444E-16,0.));
#12113=DIRECTION('',(-1.,-1.34590614515444E-16,0.));
#12114=DIRECTION('center_axis',(1.,1.34590614515444E-16,0.));
#12115=DIRECTION('ref_axis',(-1.34590614515444E-16,1.,0.));
#12116=DIRECTION('center_axis',(1.,1.34590614515444E-16,0.));
#12117=DIRECTION('ref_axis',(-1.34590614515444E-16,1.,0.));
#12118=DIRECTION('',(-1.,-1.34590614515444E-16,0.));
#12119=DIRECTION('center_axis',(1.,1.34590614515444E-16,0.));
#12120=DIRECTION('ref_axis',(-1.34590614515444E-16,1.,0.));
#12121=DIRECTION('',(-1.,-1.34590614515444E-16,0.));
#12122=DIRECTION('center_axis',(1.,1.34590614515444E-16,0.));
#12123=DIRECTION('ref_axis',(-1.34590614515444E-16,1.,0.));
#12124=DIRECTION('',(-1.,-1.34590614515444E-16,0.));
#12125=DIRECTION('center_axis',(1.,1.34590614515444E-16,0.));
#12126=DIRECTION('ref_axis',(-1.34590614515444E-16,1.,0.));
#12127=DIRECTION('',(-1.,-1.34590614515444E-16,0.));
#12128=DIRECTION('center_axis',(1.,1.34590614515444E-16,0.));
#12129=DIRECTION('ref_axis',(-1.34590614515444E-16,1.,0.));
#12130=DIRECTION('',(-1.,-1.34590614515444E-16,0.));
#12131=DIRECTION('center_axis',(1.,1.34590614515444E-16,0.));
#12132=DIRECTION('ref_axis',(-1.34590614515444E-16,1.,0.));
#12133=DIRECTION('center_axis',(1.,1.34590614515444E-16,0.));
#12134=DIRECTION('ref_axis',(-1.34590614515444E-16,1.,0.));
#12135=DIRECTION('',(-1.,-1.34590614515444E-16,0.));
#12136=DIRECTION('',(-1.,-1.34590614515444E-16,0.));
#12137=DIRECTION('',(-1.,-1.34590614515444E-16,0.));
#12138=DIRECTION('center_axis',(1.,2.36658271566304E-30,0.));
#12139=DIRECTION('ref_axis',(0.,0.,-1.));
#12140=DIRECTION('center_axis',(1.,2.36658271566304E-30,0.));
#12141=DIRECTION('ref_axis',(8.21073318940323E-45,-3.46944695195362E-15,
1.));
#12142=DIRECTION('center_axis',(1.,2.36658271566304E-30,0.));
#12143=DIRECTION('ref_axis',(8.21073318940323E-45,-3.46944695195362E-15,
1.));
#12144=DIRECTION('',(-0.707106781186551,8.65956056235472E-17,-0.707106781186544));
#12145=DIRECTION('center_axis',(-1.,-1.34590614515444E-16,0.));
#12146=DIRECTION('ref_axis',(1.34590614515444E-16,-1.,0.));
#12147=DIRECTION('center_axis',(1.,1.34590614515444E-16,0.));
#12148=DIRECTION('ref_axis',(-1.34590614515444E-16,1.,0.));
#12149=DIRECTION('center_axis',(1.,2.36658271566304E-30,0.));
#12150=DIRECTION('ref_axis',(-1.25897908904183E-44,5.31981865966221E-15,
1.));
#12151=DIRECTION('',(-1.,-1.34590614515444E-16,0.));
#12152=DIRECTION('center_axis',(1.,1.34590614515444E-16,0.));
#12153=DIRECTION('ref_axis',(-1.34590614515444E-16,1.,0.));
#12154=DIRECTION('',(-1.,-1.34590614515444E-16,0.));
#12155=DIRECTION('center_axis',(1.,1.34590614515444E-16,0.));
#12156=DIRECTION('ref_axis',(-1.34590614515444E-16,1.,0.));
#12157=DIRECTION('center_axis',(1.,1.34590614515444E-16,0.));
#12158=DIRECTION('ref_axis',(-1.34590614515444E-16,1.,0.));
#12159=DIRECTION('',(1.,1.34590614515444E-16,0.));
#12160=DIRECTION('center_axis',(1.,1.34590614515444E-16,0.));
#12161=DIRECTION('ref_axis',(-1.34590614515444E-16,1.,0.));
#12162=DIRECTION('center_axis',(1.,1.34590614515444E-16,0.));
#12163=DIRECTION('ref_axis',(-1.34590614515444E-16,1.,0.));
#12164=DIRECTION('',(-1.,-1.34590614515444E-16,0.));
#12165=DIRECTION('center_axis',(1.,1.34590614515444E-16,0.));
#12166=DIRECTION('ref_axis',(-1.34590614515444E-16,1.,0.));
#12167=DIRECTION('center_axis',(1.,1.34590614515444E-16,0.));
#12168=DIRECTION('ref_axis',(-1.34590614515444E-16,1.,0.));
#12169=DIRECTION('center_axis',(1.,1.34590614515444E-16,0.));
#12170=DIRECTION('ref_axis',(-1.34590614515444E-16,1.,0.));
#12171=DIRECTION('',(-1.,-1.34590614515444E-16,0.));
#12172=DIRECTION('center_axis',(1.,1.34590614515444E-16,0.));
#12173=DIRECTION('ref_axis',(-1.34590614515444E-16,1.,0.));
#12174=DIRECTION('center_axis',(-1.,-1.3459061451544E-16,0.));
#12175=DIRECTION('ref_axis',(1.3459061451544E-16,-1.,0.));
#12176=DIRECTION('center_axis',(1.,1.3459061451544E-16,0.));
#12177=DIRECTION('ref_axis',(-1.3459061451544E-16,1.,0.));
#12178=DIRECTION('center_axis',(1.,1.3459061451544E-16,0.));
#12179=DIRECTION('ref_axis',(-1.3459061451544E-16,1.,0.));
#12180=DIRECTION('center_axis',(0.,0.,-1.));
#12181=DIRECTION('ref_axis',(-1.,-2.36658271566304E-30,0.));
#12182=DIRECTION('',(0.241125309054894,-0.970493990364279,0.));
#12183=DIRECTION('',(0.241125309054894,0.970493990364279,5.55111512312579E-17));
#12184=DIRECTION('center_axis',(0.,0.,-1.));
#12185=DIRECTION('ref_axis',(0.970493990364279,0.241125309054894,0.));
#12186=DIRECTION('',(-0.241125309054894,-0.970493990364279,-5.55111512312578E-17));
#12187=DIRECTION('center_axis',(0.,0.,1.));
#12188=DIRECTION('ref_axis',(0.970493990364279,0.241125309054895,0.));
#12189=DIRECTION('',(-0.241125309054895,0.970493990364279,-5.55111512312579E-17));
#12190=DIRECTION('center_axis',(0.,0.,-1.));
#12191=DIRECTION('ref_axis',(-1.,-2.36658271566304E-30,0.));
#12192=DIRECTION('',(0.241125309054894,-0.970493990364279,0.));
#12193=DIRECTION('center_axis',(0.,0.,-1.));
#12194=DIRECTION('ref_axis',(0.970493990364278,0.241125309054898,0.));
#12195=DIRECTION('',(0.241125309054894,0.970493990364279,5.55111512312579E-17));
#12196=DIRECTION('center_axis',(1.,1.3459061451544E-16,0.));
#12197=DIRECTION('ref_axis',(-1.3459061451544E-16,1.,0.));
#12198=DIRECTION('',(1.57772181044202E-30,1.,0.));
#12199=DIRECTION('',(3.94430452610506E-31,0.,-1.));
#12200=DIRECTION('',(-1.57772181044202E-30,-1.,0.));
#12201=DIRECTION('center_axis',(0.,0.,-1.));
#12202=DIRECTION('ref_axis',(-1.,-2.36658271566304E-30,0.));
#12203=DIRECTION('',(1.57772181044202E-30,1.,0.));
#12204=DIRECTION('',(1.,1.34590614515444E-16,0.));
#12205=DIRECTION('center_axis',(1.34590614515444E-16,-1.,0.));
#12206=DIRECTION('ref_axis',(1.,1.34590614515444E-16,0.));
#12207=DIRECTION('',(3.94430452610506E-31,0.,-1.));
#12208=DIRECTION('',(1.,1.34590614515444E-16,0.));
#12209=DIRECTION('center_axis',(0.,0.,1.));
#12210=DIRECTION('ref_axis',(1.,2.36658271566304E-30,0.));
#12211=DIRECTION('',(-1.57772181044202E-30,-1.,0.));
#12212=DIRECTION('center_axis',(-1.,-2.36658271566304E-30,0.));
#12213=DIRECTION('ref_axis',(0.,0.,1.));
#12214=DIRECTION('center_axis',(-1.,-1.3459061451544E-16,0.));
#12215=DIRECTION('ref_axis',(1.3459061451544E-16,-1.,0.));
#12216=DIRECTION('axis',(0.,0.,1.));
#12217=DIRECTION('refdir',(1.,0.,0.));
#12218=DIRECTION('center_axis',(1.,0.,5.91645678915759E-31));
#12219=DIRECTION('ref_axis',(5.91645678915759E-31,-1.28868988380477E-29,
-1.));
#12220=DIRECTION('center_axis',(1.,0.,5.91645678915759E-31));
#12221=DIRECTION('ref_axis',(-5.91645678915759E-31,1.29257043247465E-29,
1.));
#12222=DIRECTION('center_axis',(1.,0.,5.91645678915759E-31));
#12223=DIRECTION('ref_axis',(-5.91645678915759E-31,1.29257043247465E-29,
1.));
#12224=DIRECTION('',(-0.707106781186556,8.65956056235392E-17,-0.707106781186539));
#12225=DIRECTION('center_axis',(-1.,0.,-5.91645678915759E-31));
#12226=DIRECTION('ref_axis',(-5.91645678915759E-31,1.28868988380477E-29,
1.));
#12227=DIRECTION('center_axis',(-1.,0.,-5.91645678915759E-31));
#12228=DIRECTION('ref_axis',(-5.91645678915759E-31,1.29422492262822E-29,
1.));
#12229=DIRECTION('center_axis',(1.,0.,5.91645678915759E-31));
#12230=DIRECTION('ref_axis',(5.91645678915759E-31,-1.29422492262822E-29,
-1.));
#12231=DIRECTION('',(1.,0.,5.91645678915759E-31));
#12232=DIRECTION('center_axis',(1.,0.,5.91645678915759E-31));
#12233=DIRECTION('ref_axis',(5.91645678915759E-31,-1.29422492262822E-29,
-1.));
#12234=DIRECTION('center_axis',(-1.,0.,-5.91645678915759E-31));
#12235=DIRECTION('ref_axis',(7.00649232162409E-46,-1.,-1.07187543957222E-15));
#12236=DIRECTION('center_axis',(1.,0.,5.91645678915759E-31));
#12237=DIRECTION('ref_axis',(5.91645678915759E-31,-1.28395329625816E-29,
-1.));
#12238=DIRECTION('',(-1.,0.,-5.91645678915759E-31));
#12239=DIRECTION('center_axis',(1.,0.,5.91645678915759E-31));
#12240=DIRECTION('ref_axis',(5.91645678915759E-31,-1.28395329625816E-29,
-1.));
#12241=DIRECTION('',(-1.,0.,-5.91645678915759E-31));
#12242=DIRECTION('center_axis',(-1.,0.,-5.91645678915759E-31));
#12243=DIRECTION('ref_axis',(-5.91645678915759E-31,1.28868988380477E-29,
1.));
#12244=DIRECTION('',(1.,0.,5.91645678915759E-31));
#12245=DIRECTION('center_axis',(-1.,0.,-5.91645678915759E-31));
#12246=DIRECTION('ref_axis',(-5.91645678915759E-31,1.29257043247465E-29,
1.));
#12247=DIRECTION('center_axis',(-1.,0.,-5.91645678915759E-31));
#12248=DIRECTION('ref_axis',(-5.91645678915759E-31,1.28868988380477E-29,
1.));
#12249=DIRECTION('center_axis',(1.,0.,5.91645678915759E-31));
#12250=DIRECTION('ref_axis',(5.91645678915759E-31,-1.28189897098414E-29,
-1.));
#12251=DIRECTION('',(1.,0.,5.91645678915759E-31));
#12252=DIRECTION('center_axis',(1.,0.,5.91645678915759E-31));
#12253=DIRECTION('ref_axis',(5.91645678915759E-31,-1.28868988380477E-29,
-1.));
#12254=DIRECTION('',(1.,0.,5.91645678915759E-31));
#12255=DIRECTION('center_axis',(1.,0.,5.91645678915759E-31));
#12256=DIRECTION('ref_axis',(5.91645678915759E-31,-1.28189897098414E-29,
-1.));
#12257=DIRECTION('',(1.,0.,5.91645678915759E-31));
#12258=DIRECTION('center_axis',(1.,0.,5.91645678915759E-31));
#12259=DIRECTION('ref_axis',(5.91645678915759E-31,-1.28868988380477E-29,
-1.));
#12260=DIRECTION('center_axis',(1.,-1.52489560243109E-59,-5.91645678915759E-31));
#12261=DIRECTION('ref_axis',(-5.91645678915759E-31,-1.28868988380477E-29,
-1.));
#12262=DIRECTION('',(-3.94430452610506E-31,2.22044604925018E-16,-1.));
#12263=DIRECTION('',(0.,1.,1.28868988380477E-29));
#12264=DIRECTION('',(0.,1.,1.28868988380477E-29));
#12265=DIRECTION('center_axis',(-1.,1.52489560243109E-59,5.91645678915759E-31));
#12266=DIRECTION('ref_axis',(5.91645678915759E-31,1.28868988380477E-29,
1.));
#12267=DIRECTION('center_axis',(-5.91645678915759E-31,1.28868988380477E-29,
1.));
#12268=DIRECTION('ref_axis',(1.,5.52714787526044E-76,5.91645678915759E-31));
#12269=DIRECTION('',(0.,1.,1.28868988380477E-29));
#12270=DIRECTION('',(0.,1.,1.28868988380477E-29));
#12271=DIRECTION('',(-1.,0.,-5.91645678915759E-31));
#12272=DIRECTION('center_axis',(-5.91645678915759E-31,1.28868988380477E-29,
1.));
#12273=DIRECTION('ref_axis',(1.,5.52714787526044E-76,5.91645678915759E-31));
#12274=DIRECTION('',(0.,1.,1.28868988380477E-29));
#12275=DIRECTION('',(-1.,0.,-5.91645678915759E-31));
#12276=DIRECTION('',(0.,1.,1.28868988380477E-29));
#12277=DIRECTION('center_axis',(-1.52489560243109E-59,1.,-1.28868988380477E-29));
#12278=DIRECTION('ref_axis',(5.91645678915759E-31,1.28868988380477E-29,
1.));
#12279=DIRECTION('',(-5.91645678915759E-31,-1.28868988380477E-29,-1.));
#12280=DIRECTION('',(-5.91645678915759E-31,-1.28868988380477E-29,-1.));
#12281=DIRECTION('center_axis',(1.,-1.52489560243109E-59,-5.91645678915759E-31));
#12282=DIRECTION('ref_axis',(-5.91645678915759E-31,-1.28868988380477E-29,
-1.));
#12283=DIRECTION('center_axis',(1.,-1.52489560243109E-59,-5.91645678915759E-31));
#12284=DIRECTION('ref_axis',(-5.91645678915759E-31,-1.28868988380477E-29,
-1.));
#12285=DIRECTION('center_axis',(1.,-1.52489560243109E-59,-5.91645678915759E-31));
#12286=DIRECTION('ref_axis',(-5.91645678915759E-31,-1.28868988380477E-29,
-1.));
#12287=DIRECTION('center_axis',(1.,-1.52489560243109E-59,-5.91645678915759E-31));
#12288=DIRECTION('ref_axis',(-5.91645678915759E-31,-1.28868988380477E-29,
-1.));
#12289=DIRECTION('',(0.,1.,1.28868988380477E-29));
#12290=DIRECTION('',(-3.94430452610506E-31,2.22044604925018E-16,-1.));
#12291=DIRECTION('',(0.,1.,1.28868988380477E-29));
#12292=DIRECTION('center_axis',(5.91645678915759E-31,-1.28868988380477E-29,
-1.));
#12293=DIRECTION('ref_axis',(-1.,-5.52714787526044E-76,-5.91645678915759E-31));
#12294=DIRECTION('',(1.,0.,5.91645678915759E-31));
#12295=DIRECTION('center_axis',(5.91645678915759E-31,-1.28868988380477E-29,
-1.));
#12296=DIRECTION('ref_axis',(-1.,-5.52714787526044E-76,-5.91645678915759E-31));
#12297=DIRECTION('',(1.,0.,5.91645678915759E-31));
#12298=DIRECTION('center_axis',(1.01610171333826E-59,-1.,-2.22044604925018E-16));
#12299=DIRECTION('ref_axis',(-3.94430452610506E-31,2.22044604925018E-16,
-1.));
#12300=DIRECTION('axis',(0.,0.,1.));
#12301=DIRECTION('refdir',(1.,0.,0.));
#12302=DIRECTION('center_axis',(7.09974814698911E-30,-7.88860905221012E-30,
1.));
#12303=DIRECTION('ref_axis',(1.,-2.12941982799268E-29,-7.09343725974734E-30));
#12304=DIRECTION('center_axis',(-7.09974814698911E-30,7.88860905221012E-30,
-1.));
#12305=DIRECTION('ref_axis',(1.,-2.12959150172473E-29,-7.09974814698911E-30));
#12306=DIRECTION('center_axis',(7.09974814698911E-30,-7.88860905221012E-30,
1.));
#12307=DIRECTION('ref_axis',(-1.,2.12959150172473E-29,7.09974814698911E-30));
#12308=DIRECTION('center_axis',(7.09974814698911E-30,-7.88860905221012E-30,
1.));
#12309=DIRECTION('ref_axis',(1.,-2.12941982799268E-29,-7.09343725974734E-30));
#12310=DIRECTION('center_axis',(-7.09974814698911E-30,7.88860905221012E-30,
-1.));
#12311=DIRECTION('ref_axis',(1.,-2.12959150172473E-29,-7.09974814698911E-30));
#12312=DIRECTION('center_axis',(7.09974814698911E-30,-7.88860905221012E-30,
1.));
#12313=DIRECTION('ref_axis',(-1.,2.12959150172473E-29,7.09974814698911E-30));
#12314=DIRECTION('center_axis',(7.09974814698911E-30,-7.88860905221012E-30,
1.));
#12315=DIRECTION('ref_axis',(1.,-2.12941982799268E-29,-7.09343725974734E-30));
#12316=DIRECTION('center_axis',(-7.09974814698911E-30,7.88860905221012E-30,
-1.));
#12317=DIRECTION('ref_axis',(1.,-2.12959150172473E-29,-7.09974814698911E-30));
#12318=DIRECTION('center_axis',(7.09974814698911E-30,-7.88860905221012E-30,
1.));
#12319=DIRECTION('ref_axis',(-1.,2.12959150172473E-29,7.09974814698911E-30));
#12320=DIRECTION('center_axis',(7.09974814698911E-30,-7.88860905221012E-30,
1.));
#12321=DIRECTION('ref_axis',(1.,-2.12941982799268E-29,-7.09343725974734E-30));
#12322=DIRECTION('center_axis',(-7.09974814698911E-30,7.88860905221012E-30,
-1.));
#12323=DIRECTION('ref_axis',(1.,1.95399252334027E-14,-7.09974814698895E-30));
#12324=DIRECTION('center_axis',(7.09974814698911E-30,-7.88860905221012E-30,
1.));
#12325=DIRECTION('ref_axis',(-1.,-5.32907051820073E-15,7.09974814698906E-30));
#12326=DIRECTION('center_axis',(7.09974814698911E-30,-7.88860905221012E-30,
1.));
#12327=DIRECTION('ref_axis',(1.,-2.12941982799268E-29,-7.09343725974734E-30));
#12328=DIRECTION('center_axis',(-7.09974814698911E-30,7.88860905221012E-30,
-1.));
#12329=DIRECTION('ref_axis',(1.,2.1316282072803E-14,-7.09974814698894E-30));
#12330=DIRECTION('center_axis',(7.09974814698911E-30,-7.88860905221012E-30,
1.));
#12331=DIRECTION('ref_axis',(-1.,2.6645352591004E-15,7.09974814698913E-30));
#12332=DIRECTION('center_axis',(7.09974814698911E-30,-7.88860905221012E-30,
1.));
#12333=DIRECTION('ref_axis',(1.,-2.12941982799268E-29,-7.09343725974734E-30));
#12334=DIRECTION('center_axis',(-7.09974814698911E-30,7.88860905221012E-30,
-1.));
#12335=DIRECTION('ref_axis',(1.,-2.1316282072803E-14,-7.09974814698928E-30));
#12336=DIRECTION('center_axis',(7.09974814698911E-30,-7.88860905221012E-30,
1.));
#12337=DIRECTION('ref_axis',(-1.,1.77635683940027E-15,7.09974814698912E-30));
#12338=DIRECTION('center_axis',(7.09974814698911E-30,-7.88860905221012E-30,
1.));
#12339=DIRECTION('ref_axis',(1.,-2.12941982799268E-29,-7.09343725974734E-30));
#12340=DIRECTION('center_axis',(-7.09974814698911E-30,7.88860905221012E-30,
-1.));
#12341=DIRECTION('ref_axis',(1.,-2.12959150172473E-29,-7.09974814698911E-30));
#12342=DIRECTION('center_axis',(7.09974814698911E-30,-7.88860905221012E-30,
1.));
#12343=DIRECTION('ref_axis',(-1.,-2.66453525910035E-15,7.09974814698909E-30));
#12344=DIRECTION('center_axis',(7.09974814698911E-30,-7.88860905221012E-30,
1.));
#12345=DIRECTION('ref_axis',(1.,-2.12941982799268E-29,-7.09343725974734E-30));
#12346=DIRECTION('center_axis',(-7.09974814698911E-30,7.88860905221012E-30,
-1.));
#12347=DIRECTION('ref_axis',(1.,-2.12959150172473E-29,-7.09974814698911E-30));
#12348=DIRECTION('center_axis',(7.09974814698911E-30,-7.88860905221012E-30,
1.));
#12349=DIRECTION('ref_axis',(-1.,8.88178419700147E-16,7.09974814698911E-30));
#12350=DIRECTION('center_axis',(7.09974814698911E-30,-7.88860905221012E-30,
1.));
#12351=DIRECTION('ref_axis',(1.,-2.12941982799268E-29,-7.09343725974734E-30));
#12352=DIRECTION('center_axis',(-7.09974814698911E-30,7.88860905221012E-30,
-1.));
#12353=DIRECTION('ref_axis',(1.,-2.12959150172473E-29,-7.09974814698911E-30));
#12354=DIRECTION('center_axis',(7.09974814698911E-30,-7.88860905221012E-30,
1.));
#12355=DIRECTION('ref_axis',(-1.,2.12959150172473E-29,7.09974814698911E-30));
#12356=DIRECTION('center_axis',(7.09974814698911E-30,-7.88860905221012E-30,
1.));
#12357=DIRECTION('ref_axis',(1.,-2.12941982799268E-29,-7.09343725974734E-30));
#12358=DIRECTION('center_axis',(-7.09974814698911E-30,7.88860905221012E-30,
-1.));
#12359=DIRECTION('ref_axis',(1.,-2.12959150172473E-29,-7.09974814698911E-30));
#12360=DIRECTION('center_axis',(7.09974814698911E-30,-7.88860905221012E-30,
1.));
#12361=DIRECTION('ref_axis',(-1.,8.88178419700147E-16,7.09974814698911E-30));
#12362=DIRECTION('center_axis',(7.09974814698911E-30,-7.88860905221012E-30,
1.));
#12363=DIRECTION('ref_axis',(1.,-2.12941982799268E-29,-7.09343725974734E-30));
#12364=DIRECTION('center_axis',(-7.09974814698911E-30,7.88860905221012E-30,
-1.));
#12365=DIRECTION('ref_axis',(1.,-2.12959150172473E-29,-7.09974814698911E-30));
#12366=DIRECTION('center_axis',(7.09974814698911E-30,-7.88860905221012E-30,
1.));
#12367=DIRECTION('ref_axis',(-1.,2.12959150172473E-29,7.09974814698911E-30));
#12368=DIRECTION('center_axis',(7.09974814698911E-30,-7.88860905221012E-30,
1.));
#12369=DIRECTION('ref_axis',(1.,-2.12941982799268E-29,-7.09343725974734E-30));
#12370=DIRECTION('center_axis',(-7.09974814698911E-30,7.88860905221012E-30,
-1.));
#12371=DIRECTION('ref_axis',(1.,-2.12959150172473E-29,-7.09974814698911E-30));
#12372=DIRECTION('center_axis',(7.09974814698911E-30,-7.88860905221012E-30,
1.));
#12373=DIRECTION('ref_axis',(-1.,-8.5265128291212E-14,7.09974814698844E-30));
#12374=DIRECTION('center_axis',(7.09974814698911E-30,-7.88860905221012E-30,
1.));
#12375=DIRECTION('ref_axis',(1.,-2.12941982799268E-29,-7.09343725974734E-30));
#12376=DIRECTION('center_axis',(-7.09974814698911E-30,7.88860905221012E-30,
-1.));
#12377=DIRECTION('ref_axis',(1.,-2.12959150172473E-29,-7.09974814698911E-30));
#12378=DIRECTION('center_axis',(7.09974814698911E-30,-7.88860905221012E-30,
1.));
#12379=DIRECTION('ref_axis',(-1.,-1.77635683940025E-14,7.09974814698897E-30));
#12380=DIRECTION('center_axis',(7.09974814698911E-30,-7.88860905221012E-30,
1.));
#12381=DIRECTION('ref_axis',(1.,-2.12941982799268E-29,-7.09343725974734E-30));
#12382=DIRECTION('center_axis',(-7.09974814698911E-30,7.88860905221012E-30,
-1.));
#12383=DIRECTION('ref_axis',(1.,-2.12959150172473E-29,-7.09974814698911E-30));
#12384=DIRECTION('center_axis',(7.09974814698911E-30,-7.88860905221012E-30,
1.));
#12385=DIRECTION('ref_axis',(-1.,-4.17443857259059E-14,7.09974814698878E-30));
#12386=DIRECTION('center_axis',(7.09974814698911E-30,-7.88860905221012E-30,
1.));
#12387=DIRECTION('ref_axis',(1.,-2.12941982799268E-29,-7.09343725974734E-30));
#12388=DIRECTION('center_axis',(-7.09974814698911E-30,7.88860905221012E-30,
-1.));
#12389=DIRECTION('ref_axis',(1.,-2.12959150172473E-29,-7.09974814698911E-30));
#12390=DIRECTION('center_axis',(7.09974814698911E-30,-7.88860905221012E-30,
1.));
#12391=DIRECTION('ref_axis',(-1.,1.01252339845814E-13,7.0997481469899E-30));
#12392=DIRECTION('center_axis',(7.09974814698911E-30,-7.88860905221012E-30,
1.));
#12393=DIRECTION('ref_axis',(1.,-2.12941982799268E-29,-7.09343725974734E-30));
#12394=DIRECTION('center_axis',(-7.09974814698911E-30,7.88860905221012E-30,
-1.));
#12395=DIRECTION('ref_axis',(1.,-2.12959150172473E-29,-7.09974814698911E-30));
#12396=DIRECTION('center_axis',(7.09974814698911E-30,-7.88860905221012E-30,
1.));
#12397=DIRECTION('ref_axis',(-1.,-1.33226762955019E-14,7.099748146989E-30));
#12398=DIRECTION('center_axis',(7.09974814698911E-30,-7.88860905221012E-30,
1.));
#12399=DIRECTION('ref_axis',(1.,-2.12941982799268E-29,-7.09343725974734E-30));
#12400=DIRECTION('center_axis',(-7.09974814698911E-30,7.88860905221012E-30,
-1.));
#12401=DIRECTION('ref_axis',(1.,-2.12959150172473E-29,-7.09974814698911E-30));
#12402=DIRECTION('center_axis',(7.09974814698911E-30,-7.88860905221012E-30,
1.));
#12403=DIRECTION('ref_axis',(-1.,2.57571741713037E-14,7.09974814698931E-30));
#12404=DIRECTION('center_axis',(7.09974814698911E-30,-7.88860905221012E-30,
1.));
#12405=DIRECTION('ref_axis',(1.,-2.12941982799268E-29,-7.09343725974734E-30));
#12406=DIRECTION('center_axis',(-7.09974814698911E-30,7.88860905221012E-30,
-1.));
#12407=DIRECTION('ref_axis',(1.,-2.12959150172473E-29,-7.09974814698911E-30));
#12408=DIRECTION('center_axis',(7.09974814698911E-30,-7.88860905221012E-30,
1.));
#12409=DIRECTION('ref_axis',(-1.,3.73034936274053E-14,7.0997481469894E-30));
#12410=DIRECTION('center_axis',(7.09974814698911E-30,-7.88860905221012E-30,
1.));
#12411=DIRECTION('ref_axis',(1.,-2.12941982799268E-29,-7.09343725974734E-30));
#12412=DIRECTION('center_axis',(-7.09974814698911E-30,7.88860905221012E-30,
-1.));
#12413=DIRECTION('ref_axis',(1.,-2.12959150172473E-29,-7.09974814698911E-30));
#12414=DIRECTION('center_axis',(7.09974814698911E-30,-7.88860905221012E-30,
1.));
#12415=DIRECTION('ref_axis',(-1.,-2.48689957516035E-14,7.09974814698891E-30));
#12416=DIRECTION('center_axis',(7.09974814698911E-30,-7.88860905221012E-30,
1.));
#12417=DIRECTION('ref_axis',(1.,-2.12941982799268E-29,-7.09343725974734E-30));
#12418=DIRECTION('center_axis',(-7.09974814698911E-30,7.88860905221012E-30,
-1.));
#12419=DIRECTION('ref_axis',(1.,-2.12959150172473E-29,-7.09974814698911E-30));
#12420=DIRECTION('center_axis',(7.09974814698911E-30,-7.88860905221012E-30,
1.));
#12421=DIRECTION('ref_axis',(-1.,2.12959150172473E-29,7.09974814698911E-30));
#12422=DIRECTION('center_axis',(7.09974814698911E-30,-7.88860905221012E-30,
1.));
#12423=DIRECTION('ref_axis',(1.,-2.12941982799268E-29,-7.09343725974734E-30));
#12424=DIRECTION('center_axis',(-7.09974814698911E-30,7.88860905221012E-30,
-1.));
#12425=DIRECTION('ref_axis',(1.,6.3948846218409E-14,-7.0997481469886E-30));
#12426=DIRECTION('center_axis',(7.09974814698911E-30,-7.88860905221012E-30,
1.));
#12427=DIRECTION('ref_axis',(-1.,4.61852778244065E-14,7.09974814698947E-30));
#12428=DIRECTION('center_axis',(7.09974814698911E-30,-7.88860905221012E-30,
1.));
#12429=DIRECTION('ref_axis',(1.,-2.12941982799268E-29,-7.09343725974734E-30));
#12430=DIRECTION('center_axis',(-7.09974814698911E-30,7.88860905221012E-30,
-1.));
#12431=DIRECTION('ref_axis',(1.,2.1316282072803E-14,-7.09974814698894E-30));
#12432=DIRECTION('center_axis',(7.09974814698911E-30,-7.88860905221012E-30,
1.));
#12433=DIRECTION('ref_axis',(-1.,2.22044604925032E-14,7.09974814698928E-30));
#12434=DIRECTION('center_axis',(7.09974814698911E-30,-7.88860905221012E-30,
1.));
#12435=DIRECTION('ref_axis',(1.,-2.12941982799268E-29,-7.09343725974734E-30));
#12436=DIRECTION('center_axis',(-7.09974814698911E-30,7.88860905221012E-30,
-1.));
#12437=DIRECTION('ref_axis',(1.,2.22044604925031E-14,-7.09974814698893E-30));
#12438=DIRECTION('center_axis',(7.09974814698911E-30,-7.88860905221012E-30,
1.));
#12439=DIRECTION('ref_axis',(-1.,2.12959150172473E-29,7.09974814698911E-30));
#12440=DIRECTION('center_axis',(7.09974814698911E-30,-7.88860905221012E-30,
1.));
#12441=DIRECTION('ref_axis',(1.,-2.12941982799268E-29,-7.09343725974734E-30));
#12442=DIRECTION('center_axis',(-7.09974814698911E-30,7.88860905221012E-30,
-1.));
#12443=DIRECTION('ref_axis',(1.,-4.52970994047064E-14,-7.09974814698946E-30));
#12444=DIRECTION('center_axis',(7.09974814698911E-30,-7.88860905221012E-30,
1.));
#12445=DIRECTION('ref_axis',(-1.,2.12959150172473E-29,7.09974814698911E-30));
#12446=DIRECTION('center_axis',(7.09974814698911E-30,-7.88860905221012E-30,
1.));
#12447=DIRECTION('ref_axis',(1.,-2.12941982799268E-29,-7.09343725974734E-30));
#12448=DIRECTION('center_axis',(-7.09974814698911E-30,7.88860905221012E-30,
-1.));
#12449=DIRECTION('ref_axis',(1.,4.70734562441066E-14,-7.09974814698873E-30));
#12450=DIRECTION('center_axis',(7.09974814698911E-30,-7.88860905221012E-30,
1.));
#12451=DIRECTION('ref_axis',(-1.,4.08562073062058E-14,7.09974814698943E-30));
#12452=DIRECTION('center_axis',(7.09974814698911E-30,-7.88860905221012E-30,
1.));
#12453=DIRECTION('ref_axis',(1.,-2.12941982799268E-29,-7.09343725974734E-30));
#12454=DIRECTION('center_axis',(-7.09974814698911E-30,7.88860905221012E-30,
-1.));
#12455=DIRECTION('ref_axis',(1.,-4.88498130835069E-14,-7.09974814698949E-30));
#12456=DIRECTION('center_axis',(7.09974814698911E-30,-7.88860905221012E-30,
1.));
#12457=DIRECTION('ref_axis',(-1.,-3.90798504668055E-14,7.0997481469888E-30));
#12458=DIRECTION('center_axis',(7.09974814698911E-30,-7.88860905221012E-30,
1.));
#12459=DIRECTION('ref_axis',(1.,-2.12941982799268E-29,-7.09343725974734E-30));
#12460=DIRECTION('center_axis',(-7.09974814698911E-30,7.88860905221012E-30,
-1.));
#12461=DIRECTION('ref_axis',(1.,-2.12959150172473E-29,-7.09974814698911E-30));
#12462=DIRECTION('center_axis',(7.09974814698911E-30,-7.88860905221012E-30,
1.));
#12463=DIRECTION('ref_axis',(-1.,-7.63833440942108E-14,7.0997481469885E-30));
#12464=DIRECTION('center_axis',(7.09974814698911E-30,-7.88860905221012E-30,
1.));
#12465=DIRECTION('ref_axis',(1.,-2.12941982799268E-29,-7.09343725974734E-30));
#12466=DIRECTION('center_axis',(-7.09974814698911E-30,7.88860905221012E-30,
-1.));
#12467=DIRECTION('ref_axis',(1.,5.15143483426073E-14,-7.0997481469887E-30));
#12468=DIRECTION('center_axis',(7.09974814698911E-30,-7.88860905221012E-30,
1.));
#12469=DIRECTION('ref_axis',(-1.,2.12959150172473E-29,7.09974814698911E-30));
#12470=DIRECTION('center_axis',(7.09974814698911E-30,-7.88860905221012E-30,
1.));
#12471=DIRECTION('ref_axis',(1.,-2.12941982799268E-29,-7.09343725974734E-30));
#12472=DIRECTION('center_axis',(-7.09974814698911E-30,7.88860905221012E-30,
-1.));
#12473=DIRECTION('ref_axis',(1.,-7.90478793533112E-14,-7.09974814698973E-30));
#12474=DIRECTION('center_axis',(7.09974814698911E-30,-7.88860905221012E-30,
1.));
#12475=DIRECTION('ref_axis',(-1.,2.12959150172473E-29,7.09974814698911E-30));
#12476=DIRECTION('center_axis',(7.09974814698911E-30,-7.88860905221012E-30,
1.));
#12477=DIRECTION('ref_axis',(1.,-2.12941982799268E-29,-7.09343725974734E-30));
#12478=DIRECTION('center_axis',(-7.09974814698911E-30,7.88860905221012E-30,
-1.));
#12479=DIRECTION('ref_axis',(1.,4.70734562441066E-14,-7.09974814698873E-30));
#12480=DIRECTION('center_axis',(7.09974814698911E-30,-7.88860905221012E-30,
1.));
#12481=DIRECTION('ref_axis',(-1.,2.12959150172473E-29,7.09974814698911E-30));
#12482=DIRECTION('center_axis',(7.09974814698911E-30,-7.88860905221012E-30,
1.));
#12483=DIRECTION('ref_axis',(1.,-2.12941982799268E-29,-7.09343725974734E-30));
#12484=DIRECTION('center_axis',(-7.09974814698911E-30,7.88860905221012E-30,
-1.));
#12485=DIRECTION('ref_axis',(1.,-2.75335310107039E-14,-7.09974814698932E-30));
#12486=DIRECTION('center_axis',(7.09974814698911E-30,-7.88860905221012E-30,
1.));
#12487=DIRECTION('ref_axis',(-1.,3.28626015289047E-14,7.09974814698937E-30));
#12488=DIRECTION('center_axis',(7.09974814698911E-30,-7.88860905221012E-30,
1.));
#12489=DIRECTION('ref_axis',(1.,-2.12941982799268E-29,-7.09343725974734E-30));
#12490=DIRECTION('center_axis',(-7.09974814698911E-30,7.88860905221012E-30,
-1.));
#12491=DIRECTION('ref_axis',(1.,-1.4210854715202E-14,-7.09974814698922E-30));
#12492=DIRECTION('center_axis',(7.09974814698911E-30,-7.88860905221012E-30,
1.));
#12493=DIRECTION('ref_axis',(-1.,2.12959150172473E-29,7.09974814698911E-30));
#12494=DIRECTION('center_axis',(7.09974814698911E-30,-7.88860905221012E-30,
1.));
#12495=DIRECTION('ref_axis',(1.,-2.12941982799268E-29,-7.09343725974734E-30));
#12496=DIRECTION('center_axis',(-7.09974814698911E-30,7.88860905221012E-30,
-1.));
#12497=DIRECTION('ref_axis',(1.,-1.59872115546023E-14,-7.09974814698923E-30));
#12498=DIRECTION('center_axis',(7.09974814698911E-30,-7.88860905221012E-30,
1.));
#12499=DIRECTION('ref_axis',(-1.,2.12959150172473E-29,7.09974814698911E-30));
#12500=DIRECTION('center_axis',(7.09974814698911E-30,-7.88860905221012E-30,
1.));
#12501=DIRECTION('ref_axis',(1.,-2.12941982799268E-29,-7.09343725974734E-30));
#12502=DIRECTION('center_axis',(-7.09974814698911E-30,7.88860905221012E-30,
-1.));
#12503=DIRECTION('ref_axis',(1.,-2.12959150172473E-29,-7.09974814698911E-30));
#12504=DIRECTION('center_axis',(7.09974814698911E-30,-7.88860905221012E-30,
1.));
#12505=DIRECTION('ref_axis',(-1.,-2.8421709430404E-14,7.09974814698888E-30));
#12506=DIRECTION('center_axis',(7.09974814698911E-30,-7.88860905221012E-30,
1.));
#12507=DIRECTION('ref_axis',(1.,-2.12941982799268E-29,-7.09343725974734E-30));
#12508=DIRECTION('center_axis',(-7.09974814698911E-30,7.88860905221012E-30,
-1.));
#12509=DIRECTION('ref_axis',(1.,8.88178419700104E-16,-7.0997481469891E-30));
#12510=DIRECTION('center_axis',(7.09974814698911E-30,-7.88860905221012E-30,
1.));
#12511=DIRECTION('ref_axis',(-1.,2.75335310107039E-14,7.09974814698932E-30));
#12512=DIRECTION('center_axis',(7.09974814698911E-30,-7.88860905221012E-30,
1.));
#12513=DIRECTION('ref_axis',(1.,-2.12941982799268E-29,-7.09343725974734E-30));
#12514=DIRECTION('center_axis',(-7.09974814698911E-30,7.88860905221012E-30,
-1.));
#12515=DIRECTION('ref_axis',(1.,8.88178419700104E-16,-7.0997481469891E-30));
#12516=DIRECTION('center_axis',(7.09974814698911E-30,-7.88860905221012E-30,
1.));
#12517=DIRECTION('ref_axis',(-1.,2.12959150172473E-29,7.09974814698911E-30));
#12518=DIRECTION('center_axis',(7.09974814698911E-30,-7.88860905221012E-30,
1.));
#12519=DIRECTION('ref_axis',(1.,-2.12941982799268E-29,-7.09343725974734E-30));
#12520=DIRECTION('center_axis',(-7.09974814698911E-30,7.88860905221012E-30,
-1.));
#12521=DIRECTION('ref_axis',(1.,-8.88178419700147E-16,-7.09974814698911E-30));
#12522=DIRECTION('center_axis',(7.09974814698911E-30,-7.88860905221012E-30,
1.));
#12523=DIRECTION('ref_axis',(-1.,2.12959150172473E-29,7.09974814698911E-30));
#12524=DIRECTION('center_axis',(7.09974814698911E-30,-7.88860905221012E-30,
1.));
#12525=DIRECTION('ref_axis',(1.,-2.12941982799268E-29,-7.09343725974734E-30));
#12526=DIRECTION('center_axis',(-7.09974814698911E-30,7.88860905221012E-30,
-1.));
#12527=DIRECTION('ref_axis',(1.,-2.12959150172473E-29,-7.09974814698911E-30));
#12528=DIRECTION('center_axis',(7.09974814698911E-30,-7.88860905221012E-30,
1.));
#12529=DIRECTION('ref_axis',(-1.,2.12959150172473E-29,7.09974814698911E-30));
#12530=DIRECTION('center_axis',(7.09974814698911E-30,-7.88860905221012E-30,
1.));
#12531=DIRECTION('ref_axis',(1.,-2.12941982799268E-29,-7.09343725974734E-30));
#12532=DIRECTION('center_axis',(-7.09974814698911E-30,7.88860905221012E-30,
-1.));
#12533=DIRECTION('ref_axis',(1.,1.77635683940023E-15,-7.09974814698909E-30));
#12534=DIRECTION('center_axis',(7.09974814698911E-30,-7.88860905221012E-30,
1.));
#12535=DIRECTION('ref_axis',(-1.,2.12959150172473E-29,7.09974814698911E-30));
#12536=DIRECTION('center_axis',(7.09974814698911E-30,-7.88860905221012E-30,
1.));
#12537=DIRECTION('ref_axis',(1.,-2.12941982799268E-29,-7.09343725974734E-30));
#12538=DIRECTION('center_axis',(-7.09974814698911E-30,7.88860905221012E-30,
-1.));
#12539=DIRECTION('ref_axis',(1.,-2.12959150172473E-29,-7.09974814698911E-30));
#12540=DIRECTION('center_axis',(7.09974814698911E-30,-7.88860905221012E-30,
1.));
#12541=DIRECTION('ref_axis',(-1.,-2.04281036531029E-14,7.09974814698895E-30));
#12542=DIRECTION('center_axis',(7.09974814698911E-30,-7.88860905221012E-30,
1.));
#12543=DIRECTION('ref_axis',(1.,-2.12941982799268E-29,-7.09343725974734E-30));
#12544=DIRECTION('center_axis',(-7.09974814698911E-30,7.88860905221012E-30,
-1.));
#12545=DIRECTION('ref_axis',(1.,-2.12959150172473E-29,-7.09974814698911E-30));
#12546=DIRECTION('center_axis',(7.09974814698911E-30,-7.88860905221012E-30,
1.));
#12547=DIRECTION('ref_axis',(-1.,2.12959150172473E-29,7.09974814698911E-30));
#12548=DIRECTION('center_axis',(7.09974814698911E-30,-7.88860905221012E-30,
1.));
#12549=DIRECTION('ref_axis',(1.,-2.12941982799268E-29,-7.09343725974734E-30));
#12550=DIRECTION('center_axis',(-7.09974814698911E-30,7.88860905221012E-30,
-1.));
#12551=DIRECTION('ref_axis',(1.,-2.12959150172473E-29,-7.09974814698911E-30));
#12552=DIRECTION('center_axis',(7.09974814698911E-30,-7.88860905221012E-30,
1.));
#12553=DIRECTION('ref_axis',(-1.,8.88178419700128E-15,7.09974814698918E-30));
#12554=DIRECTION('center_axis',(7.09974814698911E-30,-7.88860905221012E-30,
1.));
#12555=DIRECTION('ref_axis',(1.,-2.12941982799268E-29,-7.09343725974734E-30));
#12556=DIRECTION('center_axis',(-7.09974814698911E-30,7.88860905221012E-30,
-1.));
#12557=DIRECTION('ref_axis',(1.,-2.12959150172473E-29,-7.09974814698911E-30));
#12558=DIRECTION('center_axis',(7.09974814698911E-30,-7.88860905221012E-30,
1.));
#12559=DIRECTION('ref_axis',(-1.,2.12959150172473E-29,7.09974814698911E-30));
#12560=DIRECTION('center_axis',(7.09974814698911E-30,-7.88860905221012E-30,
1.));
#12561=DIRECTION('ref_axis',(1.,-2.12941982799268E-29,-7.09343725974734E-30));
#12562=DIRECTION('center_axis',(-7.09974814698911E-30,7.88860905221012E-30,
-1.));
#12563=DIRECTION('ref_axis',(1.,-2.12959150172473E-29,-7.09974814698911E-30));
#12564=DIRECTION('center_axis',(7.09974814698911E-30,-7.88860905221012E-30,
1.));
#12565=DIRECTION('ref_axis',(-1.,2.12959150172473E-29,7.09974814698911E-30));
#12566=DIRECTION('center_axis',(-7.09974814698911E-30,7.88860905221012E-30,
-1.));
#12567=DIRECTION('ref_axis',(-1.,2.1291967674334E-29,7.09974814698911E-30));
#12568=DIRECTION('center_axis',(-7.09974814698911E-30,7.88860905221012E-30,
-1.));
#12569=DIRECTION('ref_axis',(1.,-2.12941982799268E-29,-7.09974814698911E-30));
#12570=DIRECTION('center_axis',(-7.09974814698911E-30,7.88860905221012E-30,
-1.));
#12571=DIRECTION('ref_axis',(1.,-2.12941982799268E-29,-7.09974814698911E-30));
#12572=DIRECTION('center_axis',(-7.09974814698911E-30,7.88860905221012E-30,
-1.));
#12573=DIRECTION('ref_axis',(1.,-2.12941982799268E-29,-7.09974814698911E-30));
#12574=DIRECTION('center_axis',(-7.09974814698911E-30,7.88860905221012E-30,
-1.));
#12575=DIRECTION('ref_axis',(1.,-2.12941982799268E-29,-7.09974814698911E-30));
#12576=DIRECTION('center_axis',(-7.09974814698911E-30,7.88860905221012E-30,
-1.));
#12577=DIRECTION('ref_axis',(1.,-1.4210854715202E-14,-7.09974814698922E-30));
#12578=DIRECTION('center_axis',(-7.09974814698911E-30,7.88860905221012E-30,
-1.));
#12579=DIRECTION('ref_axis',(1.,1.4210854715202E-14,-7.09974814698899E-30));
#12580=DIRECTION('center_axis',(-7.09974814698911E-30,7.88860905221012E-30,
-1.));
#12581=DIRECTION('ref_axis',(1.,-2.12941982799268E-29,-7.09974814698911E-30));
#12582=DIRECTION('center_axis',(-7.09974814698911E-30,7.88860905221012E-30,
-1.));
#12583=DIRECTION('ref_axis',(1.,-1.24344978758018E-14,-7.0997481469892E-30));
#12584=DIRECTION('center_axis',(-7.09974814698911E-30,7.88860905221012E-30,
-1.));
#12585=DIRECTION('ref_axis',(1.,-2.12941982799268E-29,-7.09974814698911E-30));
#12586=DIRECTION('center_axis',(-7.09974814698911E-30,7.88860905221012E-30,
-1.));
#12587=DIRECTION('ref_axis',(1.,-2.12941982799268E-29,-7.09974814698911E-30));
#12588=DIRECTION('center_axis',(-7.09974814698911E-30,7.88860905221012E-30,
-1.));
#12589=DIRECTION('ref_axis',(1.,-2.12941982799268E-29,-7.09974814698911E-30));
#12590=DIRECTION('center_axis',(-7.09974814698911E-30,7.88860905221012E-30,
-1.));
#12591=DIRECTION('ref_axis',(1.,-2.12941982799268E-29,-7.09974814698911E-30));
#12592=DIRECTION('center_axis',(-7.09974814698911E-30,7.88860905221012E-30,
-1.));
#12593=DIRECTION('ref_axis',(1.,-2.12941982799268E-29,-7.09974814698911E-30));
#12594=DIRECTION('center_axis',(-7.09974814698911E-30,7.88860905221012E-30,
-1.));
#12595=DIRECTION('ref_axis',(1.,-2.12941982799268E-29,-7.09974814698911E-30));
#12596=DIRECTION('center_axis',(-7.09974814698911E-30,7.88860905221012E-30,
-1.));
#12597=DIRECTION('ref_axis',(1.,-2.12941982799268E-29,-7.09974814698911E-30));
#12598=DIRECTION('center_axis',(-7.09974814698911E-30,7.88860905221012E-30,
-1.));
#12599=DIRECTION('ref_axis',(1.,-2.6645352591004E-15,-7.09974814698913E-30));
#12600=DIRECTION('center_axis',(-7.09974814698911E-30,7.88860905221012E-30,
-1.));
#12601=DIRECTION('ref_axis',(1.,-2.12941982799268E-29,-7.09974814698911E-30));
#12602=DIRECTION('center_axis',(-7.09974814698911E-30,7.88860905221012E-30,
-1.));
#12603=DIRECTION('ref_axis',(1.,-2.12941982799268E-29,-7.09974814698911E-30));
#12604=DIRECTION('center_axis',(-7.09974814698911E-30,7.88860905221012E-30,
-1.));
#12605=DIRECTION('ref_axis',(1.,-8.88178419700147E-16,-7.09974814698911E-30));
#12606=DIRECTION('center_axis',(-7.09974814698911E-30,7.88860905221012E-30,
-1.));
#12607=DIRECTION('ref_axis',(1.,-2.12941982799268E-29,-7.09974814698911E-30));
#12608=DIRECTION('center_axis',(-7.09974814698911E-30,7.88860905221012E-30,
-1.));
#12609=DIRECTION('ref_axis',(1.,-2.12941982799268E-29,-7.09974814698911E-30));
#12610=DIRECTION('center_axis',(-7.09974814698911E-30,7.88860905221012E-30,
-1.));
#12611=DIRECTION('ref_axis',(1.,-2.12941982799268E-29,-7.09974814698911E-30));
#12612=DIRECTION('',(-0.707106781186543,8.65956056235582E-17,0.707106781186552));
#12613=DIRECTION('center_axis',(7.09974814698911E-30,-7.88860905221012E-30,
1.));
#12614=DIRECTION('ref_axis',(1.,-2.1291967674334E-29,-7.09974814698911E-30));
#12615=DIRECTION('center_axis',(-7.09974814698911E-30,7.88860905221012E-30,
-1.));
#12616=DIRECTION('ref_axis',(1.,-4.44089209850065E-15,-7.09974814698914E-30));
#12617=DIRECTION('center_axis',(-7.09974814698911E-30,7.88860905221012E-30,
-1.));
#12618=DIRECTION('ref_axis',(1.,1.59872115546022E-14,-7.09974814698898E-30));
#12619=DIRECTION('center_axis',(-7.09974814698911E-30,7.88860905221012E-30,
-1.));
#12620=DIRECTION('ref_axis',(1.,-5.15143483426073E-14,-7.09974814698951E-30));
#12621=DIRECTION('center_axis',(-7.09974814698911E-30,7.88860905221012E-30,
-1.));
#12622=DIRECTION('ref_axis',(1.,-8.88178419700147E-16,-7.09974814698911E-30));
#12623=DIRECTION('center_axis',(-7.09974814698911E-30,7.88860905221012E-30,
-1.));
#12624=DIRECTION('ref_axis',(1.,5.6843418860808E-14,-7.09974814698866E-30));
#12625=DIRECTION('center_axis',(-7.09974814698911E-30,7.88860905221012E-30,
-1.));
#12626=DIRECTION('ref_axis',(1.,3.19744231092045E-14,-7.09974814698885E-30));
#12627=DIRECTION('center_axis',(-7.09974814698911E-30,7.88860905221012E-30,
-1.));
#12628=DIRECTION('ref_axis',(1.,-2.12941982799268E-29,-7.09974814698911E-30));
#12629=DIRECTION('center_axis',(-7.09974814698911E-30,7.88860905221012E-30,
-1.));
#12630=DIRECTION('ref_axis',(1.,4.61852778244065E-14,-7.09974814698874E-30));
#12631=DIRECTION('center_axis',(-7.09974814698911E-30,7.88860905221012E-30,
-1.));
#12632=DIRECTION('ref_axis',(1.,4.44089209850063E-14,-7.09974814698876E-30));
#12633=DIRECTION('center_axis',(-7.09974814698911E-30,7.88860905221012E-30,
-1.));
#12634=DIRECTION('ref_axis',(1.,4.2632564145606E-14,-7.09974814698877E-30));
#12635=DIRECTION('center_axis',(-7.09974814698911E-30,7.88860905221012E-30,
-1.));
#12636=DIRECTION('ref_axis',(1.,2.75335310107039E-14,-7.09974814698889E-30));
#12637=DIRECTION('center_axis',(-7.09974814698911E-30,7.88860905221012E-30,
-1.));
#12638=DIRECTION('ref_axis',(1.,-5.50670620214078E-14,-7.09974814698954E-30));
#12639=DIRECTION('center_axis',(-7.09974814698911E-30,7.88860905221012E-30,
-1.));
#12640=DIRECTION('ref_axis',(1.,2.57571741713036E-14,-7.0997481469889E-30));
#12641=DIRECTION('center_axis',(-7.09974814698911E-30,7.88860905221012E-30,
-1.));
#12642=DIRECTION('ref_axis',(1.,1.24344978758017E-14,-7.09974814698901E-30));
#12643=DIRECTION('center_axis',(-7.09974814698911E-30,7.88860905221012E-30,
-1.));
#12644=DIRECTION('ref_axis',(1.,-2.48689957516035E-14,-7.0997481469893E-30));
#12645=DIRECTION('center_axis',(-7.09974814698911E-30,7.88860905221012E-30,
-1.));
#12646=DIRECTION('ref_axis',(1.,-2.48689957516035E-14,-7.0997481469893E-30));
#12647=DIRECTION('center_axis',(-7.09974814698911E-30,7.88860905221012E-30,
-1.));
#12648=DIRECTION('ref_axis',(1.,-2.12941982799268E-29,-7.09974814698911E-30));
#12649=DIRECTION('center_axis',(-7.09974814698911E-30,7.88860905221012E-30,
-1.));
#12650=DIRECTION('ref_axis',(1.,-2.12941982799268E-29,-7.09974814698911E-30));
#12651=DIRECTION('center_axis',(-7.09974814698911E-30,7.88860905221012E-30,
-1.));
#12652=DIRECTION('ref_axis',(1.,-2.12941982799268E-29,-7.09974814698911E-30));
#12653=DIRECTION('center_axis',(-7.09974814698911E-30,7.88860905221012E-30,
-1.));
#12654=DIRECTION('ref_axis',(1.,-2.12941982799268E-29,-7.09974814698911E-30));
#12655=DIRECTION('center_axis',(-7.09974814698911E-30,7.88860905221012E-30,
-1.));
#12656=DIRECTION('ref_axis',(1.,-2.12941982799268E-29,-7.09974814698911E-30));
#12657=DIRECTION('center_axis',(-7.09974814698911E-30,7.88860905221012E-30,
-1.));
#12658=DIRECTION('ref_axis',(1.,-2.12941982799268E-29,-7.09974814698911E-30));
#12659=DIRECTION('center_axis',(-7.09974814698911E-30,7.88860905221012E-30,
-1.));
#12660=DIRECTION('ref_axis',(1.83697019872082E-16,-1.,-7.88860905221012E-30));
#12661=DIRECTION('center_axis',(7.09974814698911E-30,-7.88860905221012E-30,
1.));
#12662=DIRECTION('ref_axis',(1.,-2.12879456519602E-29,-7.09974814698911E-30));
#12663=DIRECTION('',(-7.09974814698911E-30,7.88860905221012E-30,-1.));
#12664=DIRECTION('center_axis',(7.09974814698911E-30,-7.88860905221012E-30,
1.));
#12665=DIRECTION('ref_axis',(1.,-2.12879456519602E-29,-7.09974814698911E-30));
#12666=DIRECTION('',(-7.09974814698911E-30,7.88860905221012E-30,-1.));
#12667=DIRECTION('center_axis',(7.09974814698911E-30,-7.88860905221012E-30,
1.));
#12668=DIRECTION('ref_axis',(1.,-2.12959150172473E-29,-7.0997481469891E-30));
#12669=DIRECTION('center_axis',(7.09974814698911E-30,-7.88860905221012E-30,
1.));
#12670=DIRECTION('ref_axis',(1.,-2.12959150172473E-29,-7.0997481469891E-30));
#12671=DIRECTION('center_axis',(7.09974814698911E-30,-7.88860905221012E-30,
1.));
#12672=DIRECTION('ref_axis',(1.,-2.12959150172473E-29,-7.0997481469891E-30));
#12673=DIRECTION('center_axis',(7.09974814698911E-30,-7.88860905221012E-30,
1.));
#12674=DIRECTION('ref_axis',(1.,-2.12959150172473E-29,-7.0997481469891E-30));
#12675=DIRECTION('center_axis',(7.09974814698911E-30,-7.88860905221012E-30,
1.));
#12676=DIRECTION('ref_axis',(1.,-2.12959150172473E-29,-7.0997481469891E-30));
#12677=DIRECTION('center_axis',(7.09974814698911E-30,-7.88860905221012E-30,
1.));
#12678=DIRECTION('ref_axis',(1.,-2.12959150172473E-29,-7.0997481469891E-30));
#12679=DIRECTION('center_axis',(7.09974814698911E-30,-7.88860905221012E-30,
1.));
#12680=DIRECTION('ref_axis',(1.,-2.12959150172473E-29,-7.0997481469891E-30));
#12681=DIRECTION('center_axis',(7.09974814698911E-30,-7.88860905221012E-30,
1.));
#12682=DIRECTION('ref_axis',(1.,-2.12959150172473E-29,-7.0997481469891E-30));
#12683=DIRECTION('center_axis',(7.09974814698911E-30,-7.88860905221012E-30,
1.));
#12684=DIRECTION('ref_axis',(1.,-2.12959150172473E-29,-7.0997481469891E-30));
#12685=DIRECTION('center_axis',(7.09974814698911E-30,-7.88860905221012E-30,
1.));
#12686=DIRECTION('ref_axis',(1.,-2.12959150172473E-29,-7.0997481469891E-30));
#12687=DIRECTION('center_axis',(7.09974814698911E-30,-7.88860905221012E-30,
1.));
#12688=DIRECTION('ref_axis',(1.,-2.12959150172473E-29,-7.0997481469891E-30));
#12689=DIRECTION('center_axis',(7.09974814698911E-30,-7.88860905221012E-30,
1.));
#12690=DIRECTION('ref_axis',(1.,-2.12959150172473E-29,-7.0997481469891E-30));
#12691=DIRECTION('center_axis',(7.09974814698911E-30,-7.88860905221012E-30,
1.));
#12692=DIRECTION('ref_axis',(1.,-2.12959150172473E-29,-7.0997481469891E-30));
#12693=DIRECTION('center_axis',(7.09974814698911E-30,-7.88860905221012E-30,
1.));
#12694=DIRECTION('ref_axis',(1.,-2.12959150172473E-29,-7.0997481469891E-30));
#12695=DIRECTION('center_axis',(7.09974814698911E-30,-7.88860905221012E-30,
1.));
#12696=DIRECTION('ref_axis',(1.,-2.12959150172473E-29,-7.0997481469891E-30));
#12697=DIRECTION('center_axis',(7.09974814698911E-30,-7.88860905221012E-30,
1.));
#12698=DIRECTION('ref_axis',(1.,-2.12959150172473E-29,-7.0997481469891E-30));
#12699=DIRECTION('center_axis',(7.09974814698911E-30,-7.88860905221012E-30,
1.));
#12700=DIRECTION('ref_axis',(1.,-2.12959150172473E-29,-7.0997481469891E-30));
#12701=DIRECTION('center_axis',(7.09974814698911E-30,-7.88860905221012E-30,
1.));
#12702=DIRECTION('ref_axis',(1.,-2.12959150172473E-29,-7.0997481469891E-30));
#12703=DIRECTION('center_axis',(7.09974814698911E-30,-7.88860905221012E-30,
1.));
#12704=DIRECTION('ref_axis',(1.,-2.12959150172473E-29,-7.0997481469891E-30));
#12705=DIRECTION('center_axis',(7.09974814698911E-30,-7.88860905221012E-30,
1.));
#12706=DIRECTION('ref_axis',(1.,-2.12959150172473E-29,-7.0997481469891E-30));
#12707=DIRECTION('center_axis',(7.09974814698911E-30,-7.88860905221012E-30,
1.));
#12708=DIRECTION('ref_axis',(1.,-2.12959150172473E-29,-7.0997481469891E-30));
#12709=DIRECTION('center_axis',(7.09974814698911E-30,-7.88860905221012E-30,
1.));
#12710=DIRECTION('ref_axis',(1.,-2.12959150172473E-29,-7.0997481469891E-30));
#12711=DIRECTION('center_axis',(7.09974814698911E-30,-7.88860905221012E-30,
1.));
#12712=DIRECTION('ref_axis',(1.,-2.12959150172473E-29,-7.0997481469891E-30));
#12713=DIRECTION('',(0.707106781186549,8.659560562354E-17,-0.707106781186546));
#12714=DIRECTION('center_axis',(-7.09974814698911E-30,7.88860905221012E-30,
-1.));
#12715=DIRECTION('ref_axis',(1.,-2.12919676743341E-29,-7.09974814698911E-30));
#12716=DIRECTION('center_axis',(7.09974814698911E-30,-7.88860905221012E-30,
1.));
#12717=DIRECTION('ref_axis',(1.,-2.12959150172473E-29,-7.0997481469891E-30));
#12718=DIRECTION('center_axis',(7.09974814698911E-30,-7.88860905221012E-30,
1.));
#12719=DIRECTION('ref_axis',(1.,-2.12959150172473E-29,-7.0997481469891E-30));
#12720=DIRECTION('center_axis',(7.09974814698911E-30,-7.88860905221012E-30,
1.));
#12721=DIRECTION('ref_axis',(1.,-2.12959150172473E-29,-7.0997481469891E-30));
#12722=DIRECTION('center_axis',(7.09974814698911E-30,-7.88860905221012E-30,
1.));
#12723=DIRECTION('ref_axis',(1.,-2.12959150172473E-29,-7.0997481469891E-30));
#12724=DIRECTION('center_axis',(7.09974814698911E-30,-7.88860905221012E-30,
1.));
#12725=DIRECTION('ref_axis',(1.,-2.12959150172473E-29,-7.0997481469891E-30));
#12726=DIRECTION('center_axis',(7.09974814698911E-30,-7.88860905221012E-30,
1.));
#12727=DIRECTION('ref_axis',(1.,-2.12959150172473E-29,-7.0997481469891E-30));
#12728=DIRECTION('center_axis',(7.09974814698911E-30,-7.88860905221012E-30,
1.));
#12729=DIRECTION('ref_axis',(1.,-2.12959150172473E-29,-7.0997481469891E-30));
#12730=DIRECTION('center_axis',(7.09974814698911E-30,-7.88860905221012E-30,
1.));
#12731=DIRECTION('ref_axis',(1.,-2.12959150172473E-29,-7.0997481469891E-30));
#12732=DIRECTION('center_axis',(7.09974814698911E-30,-7.88860905221012E-30,
1.));
#12733=DIRECTION('ref_axis',(1.,-2.12959150172473E-29,-7.0997481469891E-30));
#12734=DIRECTION('center_axis',(7.09974814698911E-30,-7.88860905221012E-30,
1.));
#12735=DIRECTION('ref_axis',(1.,-2.12959150172473E-29,-7.0997481469891E-30));
#12736=DIRECTION('center_axis',(7.09974814698911E-30,-7.88860905221012E-30,
1.));
#12737=DIRECTION('ref_axis',(1.,-2.12959150172473E-29,-7.0997481469891E-30));
#12738=DIRECTION('center_axis',(7.09974814698911E-30,-7.88860905221012E-30,
1.));
#12739=DIRECTION('ref_axis',(1.,-2.12959150172473E-29,-7.0997481469891E-30));
#12740=DIRECTION('center_axis',(7.09974814698911E-30,-7.88860905221012E-30,
1.));
#12741=DIRECTION('ref_axis',(1.,-2.12959150172473E-29,-7.0997481469891E-30));
#12742=DIRECTION('center_axis',(7.09974814698911E-30,-7.88860905221012E-30,
1.));
#12743=DIRECTION('ref_axis',(1.,-2.12959150172473E-29,-7.0997481469891E-30));
#12744=DIRECTION('center_axis',(7.09974814698911E-30,-7.88860905221012E-30,
1.));
#12745=DIRECTION('ref_axis',(1.,-2.12959150172473E-29,-7.0997481469891E-30));
#12746=DIRECTION('center_axis',(7.09974814698911E-30,-7.88860905221012E-30,
1.));
#12747=DIRECTION('ref_axis',(1.,-2.12959150172473E-29,-7.0997481469891E-30));
#12748=DIRECTION('center_axis',(7.09974814698911E-30,-7.88860905221012E-30,
1.));
#12749=DIRECTION('ref_axis',(1.,-2.12959150172473E-29,-7.0997481469891E-30));
#12750=DIRECTION('center_axis',(7.09974814698911E-30,-7.88860905221012E-30,
1.));
#12751=DIRECTION('ref_axis',(1.,-2.12959150172473E-29,-7.0997481469891E-30));
#12752=DIRECTION('center_axis',(7.09974814698911E-30,-7.88860905221012E-30,
1.));
#12753=DIRECTION('ref_axis',(1.,-2.12959150172473E-29,-7.0997481469891E-30));
#12754=DIRECTION('center_axis',(7.09974814698911E-30,-7.88860905221012E-30,
1.));
#12755=DIRECTION('ref_axis',(1.,-2.12959150172473E-29,-7.0997481469891E-30));
#12756=DIRECTION('center_axis',(7.09974814698911E-30,-7.88860905221012E-30,
1.));
#12757=DIRECTION('ref_axis',(1.,-2.12959150172473E-29,-7.0997481469891E-30));
#12758=DIRECTION('center_axis',(7.09974814698911E-30,-7.88860905221012E-30,
1.));
#12759=DIRECTION('ref_axis',(1.,-2.12959150172473E-29,-7.0997481469891E-30));
#12760=DIRECTION('center_axis',(-7.09974814698911E-30,7.88860905221012E-30,
-1.));
#12761=DIRECTION('ref_axis',(-1.,2.12959150172473E-29,7.09974814698911E-30));
#12762=DIRECTION('center_axis',(-7.09974814698911E-30,7.88860905221012E-30,
-1.));
#12763=DIRECTION('ref_axis',(-1.,2.12959150172473E-29,7.09974814698911E-30));
#12764=DIRECTION('center_axis',(-7.09974814698911E-30,7.88860905221012E-30,
-1.));
#12765=DIRECTION('ref_axis',(-1.,2.12959150172473E-29,7.09974814698911E-30));
#12766=DIRECTION('center_axis',(-7.09974814698911E-30,7.88860905221012E-30,
-1.));
#12767=DIRECTION('ref_axis',(-1.,2.12959150172473E-29,7.09974814698911E-30));
#12768=DIRECTION('center_axis',(-7.09974814698911E-30,7.88860905221012E-30,
-1.));
#12769=DIRECTION('ref_axis',(-1.,2.12959150172473E-29,7.09974814698911E-30));
#12770=DIRECTION('center_axis',(-7.09974814698911E-30,7.88860905221012E-30,
-1.));
#12771=DIRECTION('ref_axis',(-1.,2.12959150172473E-29,7.09974814698911E-30));
#12772=DIRECTION('center_axis',(-7.09974814698911E-30,7.88860905221012E-30,
-1.));
#12773=DIRECTION('ref_axis',(-1.,2.12959150172473E-29,7.09974814698911E-30));
#12774=DIRECTION('center_axis',(-7.09974814698911E-30,7.88860905221012E-30,
-1.));
#12775=DIRECTION('ref_axis',(-1.,2.12959150172473E-29,7.09974814698911E-30));
#12776=DIRECTION('center_axis',(-7.09974814698911E-30,7.88860905221012E-30,
-1.));
#12777=DIRECTION('ref_axis',(-1.,2.12959150172473E-29,7.09974814698911E-30));
#12778=DIRECTION('center_axis',(-7.09974814698911E-30,7.88860905221012E-30,
-1.));
#12779=DIRECTION('ref_axis',(-1.,2.12959150172473E-29,7.09974814698911E-30));
#12780=DIRECTION('center_axis',(-7.09974814698911E-30,7.88860905221012E-30,
-1.));
#12781=DIRECTION('ref_axis',(-1.,2.12959150172473E-29,7.09974814698911E-30));
#12782=DIRECTION('center_axis',(-7.09974814698911E-30,7.88860905221012E-30,
-1.));
#12783=DIRECTION('ref_axis',(-1.,2.12959150172473E-29,7.09974814698911E-30));
#12784=DIRECTION('center_axis',(-7.09974814698911E-30,7.88860905221012E-30,
-1.));
#12785=DIRECTION('ref_axis',(-1.,2.12959150172473E-29,7.09974814698911E-30));
#12786=DIRECTION('center_axis',(-7.09974814698911E-30,7.88860905221012E-30,
-1.));
#12787=DIRECTION('ref_axis',(-1.,2.12959150172473E-29,7.09974814698911E-30));
#12788=DIRECTION('center_axis',(-7.09974814698911E-30,7.88860905221012E-30,
-1.));
#12789=DIRECTION('ref_axis',(-1.,2.12959150172473E-29,7.09974814698911E-30));
#12790=DIRECTION('center_axis',(-7.09974814698911E-30,7.88860905221012E-30,
-1.));
#12791=DIRECTION('ref_axis',(-1.,2.12959150172473E-29,7.09974814698911E-30));
#12792=DIRECTION('center_axis',(-7.09974814698911E-30,7.88860905221012E-30,
-1.));
#12793=DIRECTION('ref_axis',(-1.,2.12959150172473E-29,7.09974814698911E-30));
#12794=DIRECTION('center_axis',(-7.09974814698911E-30,7.88860905221012E-30,
-1.));
#12795=DIRECTION('ref_axis',(-1.,2.12959150172473E-29,7.09974814698911E-30));
#12796=DIRECTION('center_axis',(-7.09974814698911E-30,7.88860905221012E-30,
-1.));
#12797=DIRECTION('ref_axis',(-1.,2.12959150172473E-29,7.09974814698911E-30));
#12798=DIRECTION('center_axis',(-7.09974814698911E-30,7.88860905221012E-30,
-1.));
#12799=DIRECTION('ref_axis',(-1.,2.12959150172473E-29,7.09974814698911E-30));
#12800=DIRECTION('center_axis',(-7.09974814698911E-30,7.88860905221012E-30,
-1.));
#12801=DIRECTION('ref_axis',(-1.,2.12959150172473E-29,7.09974814698911E-30));
#12802=DIRECTION('center_axis',(-7.09974814698911E-30,7.88860905221012E-30,
-1.));
#12803=DIRECTION('ref_axis',(-1.,2.12959150172473E-29,7.09974814698911E-30));
#12804=DIRECTION('center_axis',(-7.09974814698911E-30,7.88860905221012E-30,
-1.));
#12805=DIRECTION('ref_axis',(-1.,2.12959150172473E-29,7.09974814698911E-30));
#12806=DIRECTION('center_axis',(-7.09974814698911E-30,7.88860905221012E-30,
-1.));
#12807=DIRECTION('ref_axis',(-1.,2.12959150172473E-29,7.09974814698911E-30));
#12808=DIRECTION('center_axis',(-7.09974814698911E-30,7.88860905221012E-30,
-1.));
#12809=DIRECTION('ref_axis',(-1.,2.12959150172473E-29,7.09974814698911E-30));
#12810=DIRECTION('center_axis',(-7.09974814698911E-30,7.88860905221012E-30,
-1.));
#12811=DIRECTION('ref_axis',(-1.,2.12959150172473E-29,7.09974814698911E-30));
#12812=DIRECTION('center_axis',(-7.09974814698911E-30,7.88860905221012E-30,
-1.));
#12813=DIRECTION('ref_axis',(-1.,2.12959150172473E-29,7.09974814698911E-30));
#12814=DIRECTION('center_axis',(-7.09974814698911E-30,7.88860905221012E-30,
-1.));
#12815=DIRECTION('ref_axis',(-1.,2.12959150172473E-29,7.09974814698911E-30));
#12816=DIRECTION('center_axis',(-7.09974814698911E-30,7.88860905221012E-30,
-1.));
#12817=DIRECTION('ref_axis',(-1.,2.12959150172473E-29,7.09974814698911E-30));
#12818=DIRECTION('center_axis',(-7.09974814698911E-30,7.88860905221012E-30,
-1.));
#12819=DIRECTION('ref_axis',(-1.,2.12959150172473E-29,7.09974814698911E-30));
#12820=DIRECTION('center_axis',(-7.09974814698911E-30,7.88860905221012E-30,
-1.));
#12821=DIRECTION('ref_axis',(-1.,2.12959150172473E-29,7.09974814698911E-30));
#12822=DIRECTION('center_axis',(-7.09974814698911E-30,7.88860905221012E-30,
-1.));
#12823=DIRECTION('ref_axis',(-1.,2.12959150172473E-29,7.09974814698911E-30));
#12824=DIRECTION('center_axis',(-7.09974814698911E-30,7.88860905221012E-30,
-1.));
#12825=DIRECTION('ref_axis',(-1.,2.12959150172473E-29,7.09974814698911E-30));
#12826=DIRECTION('center_axis',(-7.09974814698911E-30,7.88860905221012E-30,
-1.));
#12827=DIRECTION('ref_axis',(-1.,2.12959150172473E-29,7.09974814698911E-30));
#12828=DIRECTION('center_axis',(-7.09974814698911E-30,7.88860905221012E-30,
-1.));
#12829=DIRECTION('ref_axis',(-1.,2.12959150172473E-29,7.09974814698911E-30));
#12830=DIRECTION('center_axis',(-7.09974814698911E-30,7.88860905221012E-30,
-1.));
#12831=DIRECTION('ref_axis',(-1.,2.12959150172473E-29,7.09974814698911E-30));
#12832=DIRECTION('center_axis',(-7.09974814698911E-30,7.88860905221012E-30,
-1.));
#12833=DIRECTION('ref_axis',(-1.,2.12959150172473E-29,7.09974814698911E-30));
#12834=DIRECTION('center_axis',(-7.09974814698911E-30,7.88860905221012E-30,
-1.));
#12835=DIRECTION('ref_axis',(-1.,2.12959150172473E-29,7.09974814698911E-30));
#12836=DIRECTION('center_axis',(-7.09974814698911E-30,7.88860905221012E-30,
-1.));
#12837=DIRECTION('ref_axis',(-1.,2.12959150172473E-29,7.09974814698911E-30));
#12838=DIRECTION('center_axis',(-7.09974814698911E-30,7.88860905221012E-30,
-1.));
#12839=DIRECTION('ref_axis',(-1.,2.12959150172473E-29,7.09974814698911E-30));
#12840=DIRECTION('center_axis',(-7.09974814698911E-30,7.88860905221012E-30,
-1.));
#12841=DIRECTION('ref_axis',(-1.,2.12959150172473E-29,7.09974814698911E-30));
#12842=DIRECTION('center_axis',(-7.09974814698911E-30,7.88860905221012E-30,
-1.));
#12843=DIRECTION('ref_axis',(-1.,2.12959150172473E-29,7.09974814698911E-30));
#12844=DIRECTION('center_axis',(-7.09974814698911E-30,7.88860905221012E-30,
-1.));
#12845=DIRECTION('ref_axis',(-1.,2.12959150172473E-29,7.09974814698911E-30));
#12846=DIRECTION('center_axis',(-7.09974814698911E-30,7.88860905221012E-30,
-1.));
#12847=DIRECTION('ref_axis',(-1.,2.12959150172473E-29,7.09974814698911E-30));
#12848=DIRECTION('center_axis',(-7.09974814698911E-30,7.88860905221012E-30,
-1.));
#12849=DIRECTION('ref_axis',(-1.,2.12959150172473E-29,7.09974814698911E-30));
#12850=DIRECTION('center_axis',(-7.09974814698911E-30,7.88860905221012E-30,
-1.));
#12851=DIRECTION('ref_axis',(-1.,2.12959150172473E-29,7.09974814698911E-30));
#12852=DIRECTION('center_axis',(-7.09974814698911E-30,7.88860905221012E-30,
-1.));
#12853=DIRECTION('ref_axis',(-1.,2.12959150172473E-29,7.09974814698911E-30));
#12854=DIRECTION('center_axis',(-7.09974814698911E-30,7.88860905221012E-30,
-1.));
#12855=DIRECTION('ref_axis',(-1.,2.12959150172473E-29,7.09974814698911E-30));
#12856=DIRECTION('center_axis',(-7.09974814698911E-30,7.88860905221012E-30,
-1.));
#12857=DIRECTION('ref_axis',(-1.,2.12959150172473E-29,7.09974814698911E-30));
#12858=DIRECTION('center_axis',(-7.09974814698911E-30,7.88860905221012E-30,
-1.));
#12859=DIRECTION('ref_axis',(-1.,2.12959150172473E-29,7.09974814698911E-30));
#12860=DIRECTION('center_axis',(-7.09974814698911E-30,7.88860905221012E-30,
-1.));
#12861=DIRECTION('ref_axis',(-1.,2.12959150172473E-29,7.09974814698911E-30));
#12862=DIRECTION('center_axis',(-7.09974814698911E-30,7.88860905221012E-30,
-1.));
#12863=DIRECTION('ref_axis',(-1.,2.12959150172473E-29,7.09974814698911E-30));
#12864=DIRECTION('center_axis',(-7.09974814698911E-30,7.88860905221012E-30,
-1.));
#12865=DIRECTION('ref_axis',(-1.,2.12959150172473E-29,7.09974814698911E-30));
#12866=DIRECTION('center_axis',(-7.09974814698911E-30,7.88860905221012E-30,
-1.));
#12867=DIRECTION('ref_axis',(-1.,2.12959150172473E-29,7.09974814698911E-30));
#12868=DIRECTION('center_axis',(-7.09974814698911E-30,7.88860905221012E-30,
-1.));
#12869=DIRECTION('ref_axis',(-1.,2.12959150172473E-29,7.09974814698911E-30));
#12870=DIRECTION('center_axis',(-7.09974814698911E-30,7.88860905221012E-30,
-1.));
#12871=DIRECTION('ref_axis',(-1.,2.12959150172473E-29,7.09974814698911E-30));
#12872=DIRECTION('center_axis',(-7.09974814698911E-30,7.88860905221012E-30,
-1.));
#12873=DIRECTION('ref_axis',(-1.,2.12959150172473E-29,7.09974814698911E-30));
#12874=DIRECTION('center_axis',(-7.09974814698911E-30,7.88860905221012E-30,
-1.));
#12875=DIRECTION('ref_axis',(-1.,2.12959150172473E-29,7.09974814698911E-30));
#12876=DIRECTION('center_axis',(-7.09974814698911E-30,7.88860905221012E-30,
-1.));
#12877=DIRECTION('ref_axis',(-1.,2.12959150172473E-29,7.09974814698911E-30));
#12878=DIRECTION('center_axis',(-7.09974814698911E-30,7.88860905221012E-30,
-1.));
#12879=DIRECTION('ref_axis',(-1.,2.12959150172473E-29,7.09974814698911E-30));
#12880=DIRECTION('center_axis',(-7.09974814698911E-30,7.88860905221012E-30,
-1.));
#12881=DIRECTION('ref_axis',(-1.,2.12959150172473E-29,7.09974814698911E-30));
#12882=DIRECTION('center_axis',(-7.09974814698911E-30,7.88860905221012E-30,
-1.));
#12883=DIRECTION('ref_axis',(-1.,2.12959150172473E-29,7.09974814698911E-30));
#12884=DIRECTION('center_axis',(-7.09974814698911E-30,7.88860905221012E-30,
-1.));
#12885=DIRECTION('ref_axis',(-1.,2.12959150172473E-29,7.09974814698911E-30));
#12886=DIRECTION('center_axis',(-7.09974814698911E-30,7.88860905221012E-30,
-1.));
#12887=DIRECTION('ref_axis',(-1.,2.12959150172473E-29,7.09974814698911E-30));
#12888=DIRECTION('center_axis',(-7.09974814698911E-30,7.88860905221012E-30,
-1.));
#12889=DIRECTION('ref_axis',(-1.,2.12959150172473E-29,7.09974814698911E-30));
#12890=DIRECTION('center_axis',(-7.09974814698911E-30,7.88860905221012E-30,
-1.));
#12891=DIRECTION('ref_axis',(-1.,2.12959150172473E-29,7.09974814698911E-30));
#12892=DIRECTION('center_axis',(-7.09974814698911E-30,7.88860905221012E-30,
-1.));
#12893=DIRECTION('ref_axis',(-1.,2.12959150172473E-29,7.09974814698911E-30));
#12894=DIRECTION('center_axis',(-7.09974814698911E-30,7.88860905221012E-30,
-1.));
#12895=DIRECTION('ref_axis',(-1.,2.12959150172473E-29,7.09974814698911E-30));
#12896=DIRECTION('center_axis',(-7.09974814698911E-30,7.88860905221012E-30,
-1.));
#12897=DIRECTION('ref_axis',(-1.,2.12959150172473E-29,7.09974814698911E-30));
#12898=DIRECTION('center_axis',(-7.09974814698911E-30,7.88860905221012E-30,
-1.));
#12899=DIRECTION('ref_axis',(-1.,2.12959150172473E-29,7.09974814698911E-30));
#12900=DIRECTION('center_axis',(-7.09974814698911E-30,7.88860905221012E-30,
-1.));
#12901=DIRECTION('ref_axis',(-1.,2.12959150172473E-29,7.09974814698911E-30));
#12902=DIRECTION('center_axis',(-7.09974814698911E-30,7.88860905221012E-30,
-1.));
#12903=DIRECTION('ref_axis',(-1.,2.12959150172473E-29,7.09974814698911E-30));
#12904=DIRECTION('center_axis',(-7.09974814698911E-30,7.88860905221012E-30,
-1.));
#12905=DIRECTION('ref_axis',(-1.,2.12959150172473E-29,7.09974814698911E-30));
#12906=DIRECTION('center_axis',(-7.09974814698911E-30,7.88860905221012E-30,
-1.));
#12907=DIRECTION('ref_axis',(-1.,2.12959150172473E-29,7.09974814698911E-30));
#12908=DIRECTION('center_axis',(-7.09974814698911E-30,7.88860905221012E-30,
-1.));
#12909=DIRECTION('ref_axis',(-1.,2.12959150172473E-29,7.09974814698911E-30));
#12910=DIRECTION('center_axis',(-7.09974814698911E-30,7.88860905221012E-30,
-1.));
#12911=DIRECTION('ref_axis',(-1.,2.12959150172473E-29,7.09974814698911E-30));
#12912=DIRECTION('center_axis',(-7.09974814698911E-30,7.88860905221012E-30,
-1.));
#12913=DIRECTION('ref_axis',(-1.,2.12959150172473E-29,7.09974814698911E-30));
#12914=DIRECTION('center_axis',(-7.09974814698911E-30,7.88860905221012E-30,
-1.));
#12915=DIRECTION('ref_axis',(-1.,2.12959150172473E-29,7.09974814698911E-30));
#12916=DIRECTION('center_axis',(-7.09974814698911E-30,7.88860905221012E-30,
-1.));
#12917=DIRECTION('ref_axis',(-1.,2.12959150172473E-29,7.09974814698911E-30));
#12918=DIRECTION('center_axis',(-7.09974814698911E-30,7.88860905221012E-30,
-1.));
#12919=DIRECTION('ref_axis',(-1.,2.12959150172473E-29,7.09974814698911E-30));
#12920=DIRECTION('center_axis',(-7.09974814698911E-30,7.88860905221012E-30,
-1.));
#12921=DIRECTION('ref_axis',(-1.,2.12959150172473E-29,7.09974814698911E-30));
#12922=DIRECTION('center_axis',(-7.09974814698911E-30,7.88860905221012E-30,
-1.));
#12923=DIRECTION('ref_axis',(-1.,2.12959150172473E-29,7.09974814698911E-30));
#12924=DIRECTION('center_axis',(-7.09974814698911E-30,7.88860905221012E-30,
-1.));
#12925=DIRECTION('ref_axis',(-1.,2.12959150172473E-29,7.09974814698911E-30));
#12926=DIRECTION('center_axis',(-7.09974814698911E-30,7.88860905221012E-30,
-1.));
#12927=DIRECTION('ref_axis',(-1.,2.12959150172473E-29,7.09974814698911E-30));
#12928=DIRECTION('center_axis',(-7.09974814698911E-30,7.88860905221012E-30,
-1.));
#12929=DIRECTION('ref_axis',(-1.,2.12959150172473E-29,7.09974814698911E-30));
#12930=DIRECTION('center_axis',(-7.09974814698911E-30,7.88860905221012E-30,
-1.));
#12931=DIRECTION('ref_axis',(-1.,2.12959150172473E-29,7.09974814698911E-30));
#12932=DIRECTION('center_axis',(-7.09974814698911E-30,7.88860905221012E-30,
-1.));
#12933=DIRECTION('ref_axis',(-1.,2.12959150172473E-29,7.09974814698911E-30));
#12934=DIRECTION('center_axis',(-7.09974814698911E-30,7.88860905221012E-30,
-1.));
#12935=DIRECTION('ref_axis',(-1.,2.12959150172473E-29,7.09974814698911E-30));
#12936=DIRECTION('center_axis',(-6.70531769437859E-30,-7.88860905221012E-30,
1.));
#12937=DIRECTION('ref_axis',(1.,-2.12941982799268E-29,6.70531769437859E-30));
#12938=DIRECTION('',(2.12941982799268E-29,-1.,6.31088724176809E-30));
#12939=DIRECTION('',(1.,-2.12941982799268E-29,6.70531769437859E-30));
#12940=DIRECTION('',(2.12941982799268E-29,-1.,6.31088724176809E-30));
#12941=DIRECTION('center_axis',(-6.70531769437859E-30,-7.88860905221012E-30,
1.));
#12942=DIRECTION('ref_axis',(1.,-2.12941982799268E-29,6.70531769437859E-30));
#12943=DIRECTION('',(2.12941982799268E-29,-1.,6.31088724176809E-30));
#12944=DIRECTION('',(2.12941982799268E-29,-1.,6.31088724176809E-30));
#12945=DIRECTION('',(1.,-2.12941982799268E-29,6.70531769437859E-30));
#12946=DIRECTION('center_axis',(1.,-2.12941982799268E-29,-7.09974814698911E-30));
#12947=DIRECTION('ref_axis',(-7.09974814698911E-30,7.88860905221012E-30,
-1.));
#12948=DIRECTION('',(-7.09974814698911E-30,7.88860905221012E-30,-1.));
#12949=DIRECTION('center_axis',(1.,-2.12941982799268E-29,-7.09974814698911E-30));
#12950=DIRECTION('ref_axis',(-7.09974814698911E-30,7.88860905221012E-30,
-1.));
#12951=DIRECTION('',(-7.09974814698911E-30,7.88860905221012E-30,-1.));
#12952=DIRECTION('center_axis',(-2.12941982799268E-29,1.,7.88860905221012E-30));
#12953=DIRECTION('ref_axis',(7.09974814698911E-30,-7.88860905221012E-30,
1.));
#12954=DIRECTION('center_axis',(7.09974814698911E-30,-7.88860905221012E-30,
1.));
#12955=DIRECTION('ref_axis',(-1.,-1.10026367343295E-58,7.0997481469891E-30));
#12956=DIRECTION('center_axis',(7.09974814698911E-30,-7.88860905221012E-30,
1.));
#12957=DIRECTION('ref_axis',(-1.,-1.10026367343295E-58,7.0997481469891E-30));
#12958=DIRECTION('center_axis',(-7.09974814698911E-30,7.88860905221012E-30,
-1.));
#12959=DIRECTION('ref_axis',(1.,1.0890276736257E-58,-7.09974814698911E-30));
#12960=DIRECTION('center_axis',(-7.09974814698911E-30,7.88860905221012E-30,
-1.));
#12961=DIRECTION('ref_axis',(-1.,-1.0890276736257E-58,7.09974814698911E-30));
#12962=DIRECTION('center_axis',(-7.09974814698911E-30,7.88860905221012E-30,
-1.));
#12963=DIRECTION('ref_axis',(-0.989821441880933,0.142314838273285,8.1501490693107E-30));
#12964=DIRECTION('center_axis',(-7.09974814698911E-30,7.88860905221012E-30,
-1.));
#12965=DIRECTION('ref_axis',(0.989821441880933,-0.142314838273285,-8.1501490693107E-30));
#12966=DIRECTION('center_axis',(7.09974814698911E-30,-7.88860905221012E-30,
1.));
#12967=DIRECTION('ref_axis',(-0.989821441880933,0.142314838273285,8.15014906931069E-30));
#12968=DIRECTION('center_axis',(7.09974814698911E-30,-7.88860905221012E-30,
1.));
#12969=DIRECTION('ref_axis',(-0.989821441880933,0.142314838273285,8.15014906931069E-30));
#12970=DIRECTION('center_axis',(-7.09974814698911E-30,7.88860905221012E-30,
-1.));
#12971=DIRECTION('ref_axis',(-0.959492973614497,0.28173255684143,9.0346364596702E-30));
#12972=DIRECTION('center_axis',(-7.09974814698911E-30,7.88860905221012E-30,
-1.));
#12973=DIRECTION('ref_axis',(0.959492973614497,-0.281732556841431,-9.03463645967021E-30));
#12974=DIRECTION('center_axis',(7.09974814698911E-30,-7.88860905221012E-30,
1.));
#12975=DIRECTION('ref_axis',(-0.959492973614497,0.28173255684143,9.0346364596702E-30));
#12976=DIRECTION('center_axis',(7.09974814698911E-30,-7.88860905221012E-30,
1.));
#12977=DIRECTION('ref_axis',(-0.959492973614497,0.28173255684143,9.0346364596702E-30));
#12978=DIRECTION('center_axis',(-7.09974814698911E-30,7.88860905221012E-30,
-1.));
#12979=DIRECTION('ref_axis',(-0.909631995354518,0.415415013001887,9.73520470545092E-30));
#12980=DIRECTION('center_axis',(-7.09974814698911E-30,7.88860905221012E-30,
-1.));
#12981=DIRECTION('ref_axis',(0.909631995354518,-0.415415013001887,-9.73520470545091E-30));
#12982=DIRECTION('center_axis',(7.09974814698911E-30,-7.88860905221012E-30,
1.));
#12983=DIRECTION('ref_axis',(-0.909631995354518,0.415415013001887,9.73520470545091E-30));
#12984=DIRECTION('center_axis',(7.09974814698911E-30,-7.88860905221012E-30,
1.));
#12985=DIRECTION('ref_axis',(-0.909631995354518,0.415415013001887,9.73520470545091E-30));
#12986=DIRECTION('center_axis',(-7.09974814698911E-30,7.88860905221012E-30,
-1.));
#12987=DIRECTION('ref_axis',(-0.841253532831181,0.540640817455599,1.02375922574407E-29));
#12988=DIRECTION('center_axis',(-7.09974814698911E-30,7.88860905221012E-30,
-1.));
#12989=DIRECTION('ref_axis',(0.84125353283118,-0.540640817455599,-1.02375922574407E-29));
#12990=DIRECTION('center_axis',(7.09974814698911E-30,-7.88860905221012E-30,
1.));
#12991=DIRECTION('ref_axis',(-0.84125353283118,0.5406408174556,1.02375922574407E-29));
#12992=DIRECTION('center_axis',(7.09974814698911E-30,-7.88860905221012E-30,
1.));
#12993=DIRECTION('ref_axis',(-0.84125353283118,0.5406408174556,1.02375922574407E-29));
#12994=DIRECTION('center_axis',(-7.09974814698911E-30,7.88860905221012E-30,
-1.));
#12995=DIRECTION('ref_axis',(-0.755749574354257,0.654860733945286,1.05315719538472E-29));
#12996=DIRECTION('center_axis',(-7.09974814698911E-30,7.88860905221012E-30,
-1.));
#12997=DIRECTION('ref_axis',(0.755749574354257,-0.654860733945286,-1.05315719538472E-29));
#12998=DIRECTION('center_axis',(7.09974814698911E-30,-7.88860905221012E-30,
1.));
#12999=DIRECTION('ref_axis',(-0.755749574354257,0.654860733945286,1.05315719538472E-29));
#13000=DIRECTION('center_axis',(7.09974814698911E-30,-7.88860905221012E-30,
1.));
#13001=DIRECTION('ref_axis',(-0.755749574354257,0.654860733945286,1.05315719538472E-29));
#13002=DIRECTION('center_axis',(-7.09974814698911E-30,7.88860905221012E-30,
-1.));
#13003=DIRECTION('ref_axis',(-0.654860733945284,0.755749574354259,1.06111592158189E-29));
#13004=DIRECTION('center_axis',(-7.09974814698911E-30,7.88860905221012E-30,
-1.));
#13005=DIRECTION('ref_axis',(0.654860733945284,-0.75574957435426,-1.06111592158189E-29));
#13006=DIRECTION('center_axis',(7.09974814698911E-30,-7.88860905221012E-30,
1.));
#13007=DIRECTION('ref_axis',(-0.654860733945284,0.755749574354259,1.06111592158189E-29));
#13008=DIRECTION('center_axis',(7.09974814698911E-30,-7.88860905221012E-30,
1.));
#13009=DIRECTION('ref_axis',(-0.654860733945284,0.755749574354259,1.06111592158189E-29));
#13010=DIRECTION('center_axis',(-7.09974814698911E-30,7.88860905221012E-30,
-1.));
#13011=DIRECTION('ref_axis',(-0.540640817455596,0.841253532831182,1.04747338762128E-29));
#13012=DIRECTION('center_axis',(-7.09974814698911E-30,7.88860905221012E-30,
-1.));
#13013=DIRECTION('ref_axis',(0.540640817455596,-0.841253532831182,-1.04747338762128E-29));
#13014=DIRECTION('center_axis',(7.09974814698911E-30,-7.88860905221012E-30,
1.));
#13015=DIRECTION('ref_axis',(-0.540640817455596,0.841253532831182,1.04747338762128E-29));
#13016=DIRECTION('center_axis',(7.09974814698911E-30,-7.88860905221012E-30,
1.));
#13017=DIRECTION('ref_axis',(-0.540640817455596,0.841253532831182,1.04747338762128E-29));
#13018=DIRECTION('center_axis',(-7.09974814698911E-30,7.88860905221012E-30,
-1.));
#13019=DIRECTION('ref_axis',(-0.415415013001884,0.909631995354519,1.01250731615252E-29));
#13020=DIRECTION('center_axis',(-7.09974814698911E-30,7.88860905221012E-30,
-1.));
#13021=DIRECTION('ref_axis',(0.415415013001884,-0.909631995354519,-1.01250731615252E-29));
#13022=DIRECTION('center_axis',(7.09974814698911E-30,-7.88860905221012E-30,
1.));
#13023=DIRECTION('ref_axis',(-0.415415013001883,0.90963199535452,1.01250731615252E-29));
#13024=DIRECTION('center_axis',(7.09974814698911E-30,-7.88860905221012E-30,
1.));
#13025=DIRECTION('ref_axis',(-0.415415013001883,0.90963199535452,1.01250731615252E-29));
#13026=DIRECTION('center_axis',(-7.09974814698911E-30,7.88860905221012E-30,
-1.));
#13027=DIRECTION('ref_axis',(-0.281732556841427,0.959492973614498,9.56929515556876E-30));
#13028=DIRECTION('center_axis',(-7.09974814698911E-30,7.88860905221012E-30,
-1.));
#13029=DIRECTION('ref_axis',(0.281732556841427,-0.959492973614498,-9.56929515556876E-30));
#13030=DIRECTION('center_axis',(7.09974814698911E-30,-7.88860905221012E-30,
1.));
#13031=DIRECTION('ref_axis',(-0.281732556841426,0.959492973614498,9.56929515556875E-30));
#13032=DIRECTION('center_axis',(7.09974814698911E-30,-7.88860905221012E-30,
1.));
#13033=DIRECTION('ref_axis',(-0.281732556841426,0.959492973614498,9.56929515556875E-30));
#13034=DIRECTION('center_axis',(-7.09974814698911E-30,7.88860905221012E-30,
-1.));
#13035=DIRECTION('ref_axis',(-0.142314838273282,0.989821441880933,8.81871389581339E-30));
#13036=DIRECTION('center_axis',(-7.09974814698911E-30,7.88860905221012E-30,
-1.));
#13037=DIRECTION('ref_axis',(0.142314838273282,-0.989821441880933,-8.81871389581339E-30));
#13038=DIRECTION('center_axis',(7.09974814698911E-30,-7.88860905221012E-30,
1.));
#13039=DIRECTION('ref_axis',(-0.142314838273281,0.989821441880933,8.81871389581338E-30));
#13040=DIRECTION('center_axis',(7.09974814698911E-30,-7.88860905221012E-30,
1.));
#13041=DIRECTION('ref_axis',(-0.142314838273281,0.989821441880933,8.81871389581338E-30));
#13042=DIRECTION('center_axis',(-7.09974814698911E-30,7.88860905221012E-30,
-1.));
#13043=DIRECTION('ref_axis',(3.85494105772623E-15,1.,7.88860905221009E-30));
#13044=DIRECTION('center_axis',(-7.09974814698911E-30,7.88860905221012E-30,
-1.));
#13045=DIRECTION('ref_axis',(-3.85494105772623E-15,-1.,-7.88860905221009E-30));
#13046=DIRECTION('center_axis',(7.09974814698911E-30,-7.88860905221012E-30,
1.));
#13047=DIRECTION('ref_axis',(3.85494105772623E-15,1.,7.88860905221009E-30));
#13048=DIRECTION('center_axis',(7.09974814698911E-30,-7.88860905221012E-30,
1.));
#13049=DIRECTION('ref_axis',(3.85494105772623E-15,1.,7.88860905221009E-30));
#13050=DIRECTION('center_axis',(-7.09974814698911E-30,7.88860905221012E-30,
-1.));
#13051=DIRECTION('ref_axis',(0.142314838273289,0.989821441880932,6.79791487717376E-30));
#13052=DIRECTION('center_axis',(-7.09974814698911E-30,7.88860905221012E-30,
-1.));
#13053=DIRECTION('ref_axis',(-0.142314838273289,-0.989821441880932,-6.79791487717376E-30));
#13054=DIRECTION('center_axis',(7.09974814698911E-30,-7.88860905221012E-30,
1.));
#13055=DIRECTION('ref_axis',(0.142314838273288,0.989821441880932,6.79791487717376E-30));
#13056=DIRECTION('center_axis',(7.09974814698911E-30,-7.88860905221012E-30,
1.));
#13057=DIRECTION('ref_axis',(0.142314838273288,0.989821441880932,6.79791487717376E-30));
#13058=DIRECTION('center_axis',(-7.09974814698911E-30,7.88860905221012E-30,
-1.));
#13059=DIRECTION('ref_axis',(0.281732556841434,0.959492973614496,5.56883475880585E-30));
#13060=DIRECTION('center_axis',(-7.09974814698911E-30,7.88860905221012E-30,
-1.));
#13061=DIRECTION('ref_axis',(-0.281732556841434,-0.959492973614496,-5.56883475880585E-30));
#13062=DIRECTION('center_axis',(7.09974814698911E-30,-7.88860905221012E-30,
1.));
#13063=DIRECTION('ref_axis',(0.281732556841434,0.959492973614496,5.56883475880585E-30));
#13064=DIRECTION('center_axis',(7.09974814698911E-30,-7.88860905221012E-30,
1.));
#13065=DIRECTION('ref_axis',(0.281732556841434,0.959492973614496,5.56883475880585E-30));
#13066=DIRECTION('center_axis',(-7.09974814698911E-30,7.88860905221012E-30,
-1.));
#13067=DIRECTION('ref_axis',(0.415415013001891,0.909631995354516,4.22638922394196E-30));
#13068=DIRECTION('center_axis',(-7.09974814698911E-30,7.88860905221012E-30,
-1.));
#13069=DIRECTION('ref_axis',(-0.415415013001891,-0.909631995354516,-4.22638922394196E-30));
#13070=DIRECTION('center_axis',(7.09974814698911E-30,-7.88860905221012E-30,
1.));
#13071=DIRECTION('ref_axis',(0.415415013001891,0.909631995354516,4.22638922394196E-30));
#13072=DIRECTION('center_axis',(7.09974814698911E-30,-7.88860905221012E-30,
1.));
#13073=DIRECTION('ref_axis',(0.415415013001891,0.909631995354516,4.22638922394196E-30));
#13074=DIRECTION('center_axis',(-7.09974814698911E-30,7.88860905221012E-30,
-1.));
#13075=DIRECTION('ref_axis',(0.0473042560766741,0.998880527068694,7.54392966348545E-30));
#13076=DIRECTION('center_axis',(-7.09974814698911E-30,7.88860905221012E-30,
-1.));
#13077=DIRECTION('ref_axis',(-0.646029139287098,-0.76331274795589,-1.43483166863767E-30));
#13078=DIRECTION('center_axis',(7.09974814698911E-30,-7.88860905221012E-30,
1.));
#13079=DIRECTION('ref_axis',(0.27333986172383,-0.961917522448155,-9.52883545183607E-30));
#13080=DIRECTION('center_axis',(7.09974814698911E-30,-7.88860905221012E-30,
1.));
#13081=DIRECTION('ref_axis',(0.27333986172383,-0.961917522448155,-9.52883545183607E-30));
#13082=DIRECTION('center_axis',(-7.09974814698911E-30,7.88860905221012E-30,
-1.));
#13083=DIRECTION('ref_axis',(0.654860733945289,0.755749574354255,1.31246665109093E-30));
#13084=DIRECTION('center_axis',(-7.09974814698911E-30,7.88860905221012E-30,
-1.));
#13085=DIRECTION('ref_axis',(-0.654860733945289,-0.755749574354255,-1.31246665109092E-30));
#13086=DIRECTION('center_axis',(7.09974814698911E-30,-7.88860905221012E-30,
1.));
#13087=DIRECTION('ref_axis',(0.654860733945288,0.755749574354255,1.31246665109094E-30));
#13088=DIRECTION('center_axis',(7.09974814698911E-30,-7.88860905221012E-30,
1.));
#13089=DIRECTION('ref_axis',(0.654860733945288,0.755749574354255,1.31246665109094E-30));
#13090=DIRECTION('center_axis',(-7.09974814698911E-30,7.88860905221012E-30,
-1.));
#13091=DIRECTION('ref_axis',(0.755749574354262,0.654860733945281,-1.99691326371774E-31));
#13092=DIRECTION('center_axis',(-7.09974814698911E-30,7.88860905221012E-30,
-1.));
#13093=DIRECTION('ref_axis',(-0.755749574354262,-0.654860733945281,1.99691326371774E-31));
#13094=DIRECTION('center_axis',(7.09974814698911E-30,-7.88860905221012E-30,
1.));
#13095=DIRECTION('ref_axis',(0.755749574354263,0.65486073394528,-1.99691326371783E-31));
#13096=DIRECTION('center_axis',(7.09974814698911E-30,-7.88860905221012E-30,
1.));
#13097=DIRECTION('ref_axis',(0.755749574354263,0.65486073394528,-1.99691326371783E-31));
#13098=DIRECTION('center_axis',(-7.09974814698911E-30,7.88860905221012E-30,
-1.));
#13099=DIRECTION('ref_axis',(0.841253532831184,0.540640817455593,-1.70778416429177E-30));
#13100=DIRECTION('center_axis',(-7.09974814698911E-30,7.88860905221012E-30,
-1.));
#13101=DIRECTION('ref_axis',(-0.841253532831185,-0.540640817455593,1.70778416429178E-30));
#13102=DIRECTION('center_axis',(7.09974814698911E-30,-7.88860905221012E-30,
1.));
#13103=DIRECTION('ref_axis',(0.841253532831184,0.540640817455592,-1.70778416429178E-30));
#13104=DIRECTION('center_axis',(7.09974814698911E-30,-7.88860905221012E-30,
1.));
#13105=DIRECTION('ref_axis',(0.841253532831184,0.540640817455592,-1.70778416429178E-30));
#13106=DIRECTION('center_axis',(-7.09974814698911E-30,7.88860905221012E-30,
-1.));
#13107=DIRECTION('ref_axis',(0.909631995354521,0.415415013001881,-3.18111144146964E-30));
#13108=DIRECTION('center_axis',(-7.09974814698911E-30,7.88860905221012E-30,
-1.));
#13109=DIRECTION('ref_axis',(-0.909631995354521,-0.415415013001881,3.18111144146964E-30));
#13110=DIRECTION('center_axis',(7.09974814698911E-30,-7.88860905221012E-30,
1.));
#13111=DIRECTION('ref_axis',(0.909631995354522,0.415415013001879,-3.18111144146966E-30));
#13112=DIRECTION('center_axis',(7.09974814698911E-30,-7.88860905221012E-30,
1.));
#13113=DIRECTION('ref_axis',(0.909631995354522,0.415415013001879,-3.18111144146966E-30));
#13114=DIRECTION('center_axis',(-7.09974814698911E-30,7.88860905221012E-30,
-1.));
#13115=DIRECTION('ref_axis',(0.959492973614499,0.281732556841423,-4.58968046326706E-30));
#13116=DIRECTION('center_axis',(-7.09974814698911E-30,7.88860905221012E-30,
-1.));
#13117=DIRECTION('ref_axis',(-0.959492973614499,-0.281732556841423,4.58968046326706E-30));
#13118=DIRECTION('center_axis',(7.09974814698911E-30,-7.88860905221012E-30,
1.));
#13119=DIRECTION('ref_axis',(0.9594929736145,0.281732556841422,-4.58968046326707E-30));
#13120=DIRECTION('center_axis',(7.09974814698911E-30,-7.88860905221012E-30,
1.));
#13121=DIRECTION('ref_axis',(0.9594929736145,0.281732556841422,-4.58968046326707E-30));
#13122=DIRECTION('center_axis',(-7.09974814698911E-30,7.88860905221012E-30,
-1.));
#13123=DIRECTION('ref_axis',(0.989821441880934,0.142314838273278,-5.90481682637785E-30));
#13124=DIRECTION('center_axis',(-7.09974814698911E-30,7.88860905221012E-30,
-1.));
#13125=DIRECTION('ref_axis',(-0.989821441880934,-0.142314838273278,5.90481682637784E-30));
#13126=DIRECTION('center_axis',(7.09974814698911E-30,-7.88860905221012E-30,
1.));
#13127=DIRECTION('ref_axis',(0.989821441880934,0.142314838273277,-5.90481682637786E-30));
#13128=DIRECTION('center_axis',(7.09974814698911E-30,-7.88860905221012E-30,
1.));
#13129=DIRECTION('ref_axis',(0.989821441880934,0.142314838273277,-5.90481682637786E-30));
#13130=DIRECTION('center_axis',(-7.09974814698911E-30,7.88860905221012E-30,
-1.));
#13131=DIRECTION('ref_axis',(1.,1.0890276736257E-58,-7.09974814698911E-30));
#13132=DIRECTION('center_axis',(-7.09974814698911E-30,7.88860905221012E-30,
-1.));
#13133=DIRECTION('ref_axis',(-1.,-1.0890276736257E-58,7.09974814698911E-30));
#13134=DIRECTION('center_axis',(7.09974814698911E-30,-7.88860905221012E-30,
1.));
#13135=DIRECTION('ref_axis',(1.,1.0890276736257E-58,-7.0997481469891E-30));
#13136=DIRECTION('center_axis',(7.09974814698911E-30,-7.88860905221012E-30,
1.));
#13137=DIRECTION('ref_axis',(1.,1.0890276736257E-58,-7.0997481469891E-30));
#13138=DIRECTION('center_axis',(-7.09974814698911E-30,7.88860905221012E-30,
-1.));
#13139=DIRECTION('ref_axis',(0.989821441880932,-0.142314838273293,-8.15014906931075E-30));
#13140=DIRECTION('center_axis',(-7.09974814698911E-30,7.88860905221012E-30,
-1.));
#13141=DIRECTION('ref_axis',(-0.989821441880932,0.142314838273293,8.15014906931075E-30));
#13142=DIRECTION('center_axis',(7.09974814698911E-30,-7.88860905221012E-30,
1.));
#13143=DIRECTION('ref_axis',(0.989821441880932,-0.142314838273292,-8.15014906931074E-30));
#13144=DIRECTION('center_axis',(7.09974814698911E-30,-7.88860905221012E-30,
1.));
#13145=DIRECTION('ref_axis',(0.989821441880932,-0.142314838273292,-8.15014906931074E-30));
#13146=DIRECTION('center_axis',(-7.09974814698911E-30,7.88860905221012E-30,
-1.));
#13147=DIRECTION('ref_axis',(0.959492973614495,-0.281732556841437,-9.03463645967024E-30));
#13148=DIRECTION('center_axis',(-7.09974814698911E-30,7.88860905221012E-30,
-1.));
#13149=DIRECTION('ref_axis',(-0.959492973614495,0.281732556841437,9.03463645967024E-30));
#13150=DIRECTION('center_axis',(7.09974814698911E-30,-7.88860905221012E-30,
1.));
#13151=DIRECTION('ref_axis',(0.959492973614495,-0.281732556841437,-9.03463645967025E-30));
#13152=DIRECTION('center_axis',(7.09974814698911E-30,-7.88860905221012E-30,
1.));
#13153=DIRECTION('ref_axis',(0.959492973614495,-0.281732556841437,-9.03463645967025E-30));
#13154=DIRECTION('center_axis',(-7.09974814698911E-30,7.88860905221012E-30,
-1.));
#13155=DIRECTION('ref_axis',(0.909631995354515,-0.415415013001894,-9.73520470545095E-30));
#13156=DIRECTION('center_axis',(-7.09974814698911E-30,7.88860905221012E-30,
-1.));
#13157=DIRECTION('ref_axis',(-0.909631995354515,0.415415013001894,9.73520470545095E-30));
#13158=DIRECTION('center_axis',(7.09974814698911E-30,-7.88860905221012E-30,
1.));
#13159=DIRECTION('ref_axis',(0.909631995354515,-0.415415013001894,-9.73520470545095E-30));
#13160=DIRECTION('center_axis',(7.09974814698911E-30,-7.88860905221012E-30,
1.));
#13161=DIRECTION('ref_axis',(0.909631995354515,-0.415415013001894,-9.73520470545095E-30));
#13162=DIRECTION('center_axis',(-7.09974814698911E-30,7.88860905221012E-30,
-1.));
#13163=DIRECTION('ref_axis',(0.841253532831177,-0.540640817455604,-1.02375922574407E-29));
#13164=DIRECTION('center_axis',(-7.09974814698911E-30,7.88860905221012E-30,
-1.));
#13165=DIRECTION('ref_axis',(-0.841253532831177,0.540640817455605,1.02375922574407E-29));
#13166=DIRECTION('center_axis',(7.09974814698911E-30,-7.88860905221012E-30,
1.));
#13167=DIRECTION('ref_axis',(0.841253532831177,-0.540640817455604,-1.02375922574407E-29));
#13168=DIRECTION('center_axis',(7.09974814698911E-30,-7.88860905221012E-30,
1.));
#13169=DIRECTION('ref_axis',(0.841253532831177,-0.540640817455604,-1.02375922574407E-29));
#13170=DIRECTION('center_axis',(-7.09974814698911E-30,7.88860905221012E-30,
-1.));
#13171=DIRECTION('ref_axis',(0.755749574354253,-0.654860733945292,-1.05315719538472E-29));
#13172=DIRECTION('center_axis',(-7.09974814698911E-30,7.88860905221012E-30,
-1.));
#13173=DIRECTION('ref_axis',(-0.755749574354252,0.654860733945292,1.05315719538472E-29));
#13174=DIRECTION('center_axis',(7.09974814698911E-30,-7.88860905221012E-30,
1.));
#13175=DIRECTION('ref_axis',(0.755749574354253,-0.654860733945291,-1.05315719538472E-29));
#13176=DIRECTION('center_axis',(7.09974814698911E-30,-7.88860905221012E-30,
1.));
#13177=DIRECTION('ref_axis',(0.755749574354253,-0.654860733945291,-1.05315719538472E-29));
#13178=DIRECTION('center_axis',(-7.09974814698911E-30,7.88860905221012E-30,
-1.));
#13179=DIRECTION('ref_axis',(0.654860733945278,-0.755749574354264,-1.06111592158189E-29));
#13180=DIRECTION('center_axis',(-7.09974814698911E-30,7.88860905221012E-30,
-1.));
#13181=DIRECTION('ref_axis',(-0.654860733945278,0.755749574354264,1.06111592158189E-29));
#13182=DIRECTION('center_axis',(7.09974814698911E-30,-7.88860905221012E-30,
1.));
#13183=DIRECTION('ref_axis',(0.654860733945278,-0.755749574354264,-1.06111592158189E-29));
#13184=DIRECTION('center_axis',(7.09974814698911E-30,-7.88860905221012E-30,
1.));
#13185=DIRECTION('ref_axis',(0.654860733945278,-0.755749574354264,-1.06111592158189E-29));
#13186=DIRECTION('center_axis',(-7.09974814698911E-30,7.88860905221012E-30,
-1.));
#13187=DIRECTION('ref_axis',(0.540640817455589,-0.841253532831186,-1.04747338762128E-29));
#13188=DIRECTION('center_axis',(-7.09974814698911E-30,7.88860905221012E-30,
-1.));
#13189=DIRECTION('ref_axis',(-0.540640817455589,0.841253532831186,1.04747338762128E-29));
#13190=DIRECTION('center_axis',(7.09974814698911E-30,-7.88860905221012E-30,
1.));
#13191=DIRECTION('ref_axis',(0.540640817455589,-0.841253532831187,-1.04747338762128E-29));
#13192=DIRECTION('center_axis',(7.09974814698911E-30,-7.88860905221012E-30,
1.));
#13193=DIRECTION('ref_axis',(0.540640817455589,-0.841253532831187,-1.04747338762128E-29));
#13194=DIRECTION('center_axis',(-7.09974814698911E-30,7.88860905221012E-30,
-1.));
#13195=DIRECTION('ref_axis',(0.415415013001877,-0.909631995354522,-1.01250731615252E-29));
#13196=DIRECTION('center_axis',(-7.09974814698911E-30,7.88860905221012E-30,
-1.));
#13197=DIRECTION('ref_axis',(-0.415415013001877,0.909631995354522,1.01250731615252E-29));
#13198=DIRECTION('center_axis',(7.09974814698911E-30,-7.88860905221012E-30,
1.));
#13199=DIRECTION('ref_axis',(0.415415013001879,-0.909631995354522,-1.01250731615252E-29));
#13200=DIRECTION('center_axis',(7.09974814698911E-30,-7.88860905221012E-30,
1.));
#13201=DIRECTION('ref_axis',(0.415415013001879,-0.909631995354522,-1.01250731615252E-29));
#13202=DIRECTION('center_axis',(-7.09974814698911E-30,7.88860905221012E-30,
-1.));
#13203=DIRECTION('ref_axis',(0.281732556841419,-0.9594929736145,-9.56929515556872E-30));
#13204=DIRECTION('center_axis',(-7.09974814698911E-30,7.88860905221012E-30,
-1.));
#13205=DIRECTION('ref_axis',(-0.28173255684142,0.9594929736145,9.56929515556872E-30));
#13206=DIRECTION('center_axis',(7.09974814698911E-30,-7.88860905221012E-30,
1.));
#13207=DIRECTION('ref_axis',(0.281732556841418,-0.959492973614501,-9.56929515556872E-30));
#13208=DIRECTION('center_axis',(7.09974814698911E-30,-7.88860905221012E-30,
1.));
#13209=DIRECTION('ref_axis',(0.281732556841418,-0.959492973614501,-9.56929515556872E-30));
#13210=DIRECTION('center_axis',(-7.09974814698911E-30,7.88860905221012E-30,
-1.));
#13211=DIRECTION('ref_axis',(0.142314838273275,-0.989821441880934,-8.81871389581334E-30));
#13212=DIRECTION('center_axis',(-7.09974814698911E-30,7.88860905221012E-30,
-1.));
#13213=DIRECTION('ref_axis',(-0.142314838273275,0.989821441880934,8.81871389581335E-30));
#13214=DIRECTION('center_axis',(7.09974814698911E-30,-7.88860905221012E-30,
1.));
#13215=DIRECTION('ref_axis',(0.142314838273273,-0.989821441880935,-8.81871389581334E-30));
#13216=DIRECTION('center_axis',(7.09974814698911E-30,-7.88860905221012E-30,
1.));
#13217=DIRECTION('ref_axis',(0.142314838273273,-0.989821441880935,-8.81871389581334E-30));
#13218=DIRECTION('center_axis',(-7.09974814698911E-30,7.88860905221012E-30,
-1.));
#13219=DIRECTION('ref_axis',(-1.04083408558608E-14,-1.,-7.88860905221005E-30));
#13220=DIRECTION('center_axis',(-7.09974814698911E-30,7.88860905221012E-30,
-1.));
#13221=DIRECTION('ref_axis',(1.04083408558608E-14,1.,7.88860905221005E-30));
#13222=DIRECTION('center_axis',(7.09974814698911E-30,-7.88860905221012E-30,
1.));
#13223=DIRECTION('ref_axis',(-1.15648231731787E-14,-1.,-7.88860905221003E-30));
#13224=DIRECTION('center_axis',(7.09974814698911E-30,-7.88860905221012E-30,
1.));
#13225=DIRECTION('ref_axis',(-1.15648231731787E-14,-1.,-7.88860905221003E-30));
#13226=DIRECTION('center_axis',(-7.09974814698911E-30,7.88860905221012E-30,
-1.));
#13227=DIRECTION('ref_axis',(-0.142314838273296,-0.989821441880931,-6.7979148771737E-30));
#13228=DIRECTION('center_axis',(-7.09974814698911E-30,7.88860905221012E-30,
-1.));
#13229=DIRECTION('ref_axis',(0.142314838273296,0.989821441880931,6.7979148771737E-30));
#13230=DIRECTION('center_axis',(7.09974814698911E-30,-7.88860905221012E-30,
1.));
#13231=DIRECTION('ref_axis',(-0.142314838273296,-0.989821441880931,-6.7979148771737E-30));
#13232=DIRECTION('center_axis',(7.09974814698911E-30,-7.88860905221012E-30,
1.));
#13233=DIRECTION('ref_axis',(-0.142314838273296,-0.989821441880931,-6.7979148771737E-30));
#13234=DIRECTION('center_axis',(-7.09974814698911E-30,7.88860905221012E-30,
-1.));
#13235=DIRECTION('ref_axis',(-0.281732556841441,-0.959492973614494,-5.56883475880578E-30));
#13236=DIRECTION('center_axis',(-7.09974814698911E-30,7.88860905221012E-30,
-1.));
#13237=DIRECTION('ref_axis',(0.281732556841441,0.959492973614494,5.56883475880578E-30));
#13238=DIRECTION('center_axis',(7.09974814698911E-30,-7.88860905221012E-30,
1.));
#13239=DIRECTION('ref_axis',(-0.281732556841441,-0.959492973614494,-5.56883475880578E-30));
#13240=DIRECTION('center_axis',(7.09974814698911E-30,-7.88860905221012E-30,
1.));
#13241=DIRECTION('ref_axis',(-0.281732556841441,-0.959492973614494,-5.56883475880578E-30));
#13242=DIRECTION('center_axis',(-7.09974814698911E-30,7.88860905221012E-30,
-1.));
#13243=DIRECTION('ref_axis',(-0.415415013001897,-0.909631995354514,-4.22638922394189E-30));
#13244=DIRECTION('center_axis',(-7.09974814698911E-30,7.88860905221012E-30,
-1.));
#13245=DIRECTION('ref_axis',(0.415415013001897,0.909631995354513,4.22638922394189E-30));
#13246=DIRECTION('center_axis',(7.09974814698911E-30,-7.88860905221012E-30,
1.));
#13247=DIRECTION('ref_axis',(-0.415415013001898,-0.909631995354513,-4.22638922394188E-30));
#13248=DIRECTION('center_axis',(7.09974814698911E-30,-7.88860905221012E-30,
1.));
#13249=DIRECTION('ref_axis',(-0.415415013001898,-0.909631995354513,-4.22638922394188E-30));
#13250=DIRECTION('center_axis',(-7.09974814698911E-30,7.88860905221012E-30,
-1.));
#13251=DIRECTION('ref_axis',(-0.0473042560766785,-0.998880527068694,-7.54392966348542E-30));
#13252=DIRECTION('center_axis',(-7.09974814698911E-30,7.88860905221012E-30,
-1.));
#13253=DIRECTION('ref_axis',(0.646029139287104,0.763312747955885,1.43483166863759E-30));
#13254=DIRECTION('center_axis',(7.49417859959961E-30,-7.88860905221012E-30,
1.));
#13255=DIRECTION('ref_axis',(-0.273339861723828,0.961917522448156,9.63664901721228E-30));
#13256=DIRECTION('center_axis',(7.49417859959961E-30,-7.88860905221012E-30,
1.));
#13257=DIRECTION('ref_axis',(-0.273339861723828,0.961917522448156,9.63664901721228E-30));
#13258=DIRECTION('center_axis',(-7.09974814698911E-30,7.88860905221012E-30,
-1.));
#13259=DIRECTION('ref_axis',(-0.654860733945295,-0.75574957435425,-1.31246665109085E-30));
#13260=DIRECTION('center_axis',(-7.09974814698911E-30,7.88860905221012E-30,
-1.));
#13261=DIRECTION('ref_axis',(0.654860733945295,0.75574957435425,1.31246665109085E-30));
#13262=DIRECTION('center_axis',(7.09974814698911E-30,-7.88860905221012E-30,
1.));
#13263=DIRECTION('ref_axis',(-0.654860733945294,-0.75574957435425,-1.31246665109085E-30));
#13264=DIRECTION('center_axis',(7.09974814698911E-30,-7.88860905221012E-30,
1.));
#13265=DIRECTION('ref_axis',(-0.654860733945294,-0.75574957435425,-1.31246665109085E-30));
#13266=DIRECTION('center_axis',(-7.09974814698911E-30,7.88860905221012E-30,
-1.));
#13267=DIRECTION('ref_axis',(-0.755749574354266,-0.654860733945276,1.99691326371847E-31));
#13268=DIRECTION('center_axis',(-7.09974814698911E-30,7.88860905221012E-30,
-1.));
#13269=DIRECTION('ref_axis',(0.755749574354267,0.654860733945276,-1.99691326371846E-31));
#13270=DIRECTION('center_axis',(7.09974814698911E-30,-7.88860905221012E-30,
1.));
#13271=DIRECTION('ref_axis',(-0.755749574354267,-0.654860733945275,1.99691326371857E-31));
#13272=DIRECTION('center_axis',(7.09974814698911E-30,-7.88860905221012E-30,
1.));
#13273=DIRECTION('ref_axis',(-0.755749574354267,-0.654860733945275,1.99691326371857E-31));
#13274=DIRECTION('center_axis',(-7.09974814698911E-30,7.88860905221012E-30,
-1.));
#13275=DIRECTION('ref_axis',(-0.841253532831189,-0.540640817455586,1.70778416429186E-30));
#13276=DIRECTION('center_axis',(-7.09974814698911E-30,7.88860905221012E-30,
-1.));
#13277=DIRECTION('ref_axis',(0.841253532831188,0.540640817455586,-1.70778416429185E-30));
#13278=DIRECTION('center_axis',(7.09974814698911E-30,-7.88860905221012E-30,
1.));
#13279=DIRECTION('ref_axis',(-0.841253532831189,-0.540640817455585,1.70778416429187E-30));
#13280=DIRECTION('center_axis',(7.09974814698911E-30,-7.88860905221012E-30,
1.));
#13281=DIRECTION('ref_axis',(-0.841253532831189,-0.540640817455585,1.70778416429187E-30));
#13282=DIRECTION('center_axis',(-7.09974814698911E-30,7.88860905221012E-30,
-1.));
#13283=DIRECTION('ref_axis',(-0.909631995354524,-0.415415013001874,3.18111144146971E-30));
#13284=DIRECTION('center_axis',(-7.09974814698911E-30,7.88860905221012E-30,
-1.));
#13285=DIRECTION('ref_axis',(0.909631995354524,0.415415013001874,-3.18111144146971E-30));
#13286=DIRECTION('center_axis',(7.09974814698911E-30,-7.88860905221012E-30,
1.));
#13287=DIRECTION('ref_axis',(-0.909631995354523,-0.415415013001875,3.1811114414697E-30));
#13288=DIRECTION('center_axis',(7.09974814698911E-30,-7.88860905221012E-30,
1.));
#13289=DIRECTION('ref_axis',(-0.909631995354523,-0.415415013001875,3.1811114414697E-30));
#13290=DIRECTION('center_axis',(-7.09974814698911E-30,7.88860905221012E-30,
-1.));
#13291=DIRECTION('ref_axis',(-0.959492973614501,-0.281732556841416,4.58968046326713E-30));
#13292=DIRECTION('center_axis',(-7.09974814698911E-30,7.88860905221012E-30,
-1.));
#13293=DIRECTION('ref_axis',(0.959492973614501,0.281732556841416,-4.58968046326713E-30));
#13294=DIRECTION('center_axis',(7.09974814698911E-30,-7.88860905221012E-30,
1.));
#13295=DIRECTION('ref_axis',(-0.959492973614502,-0.281732556841414,4.58968046326714E-30));
#13296=DIRECTION('center_axis',(7.09974814698911E-30,-7.88860905221012E-30,
1.));
#13297=DIRECTION('ref_axis',(-0.959492973614502,-0.281732556841414,4.58968046326714E-30));
#13298=DIRECTION('center_axis',(-7.09974814698911E-30,7.88860905221012E-30,
-1.));
#13299=DIRECTION('ref_axis',(-0.989821441880935,-0.142314838273271,5.90481682637791E-30));
#13300=DIRECTION('center_axis',(-7.09974814698911E-30,7.88860905221012E-30,
-1.));
#13301=DIRECTION('ref_axis',(0.989821441880935,0.142314838273271,-5.90481682637791E-30));
#13302=DIRECTION('center_axis',(7.09974814698911E-30,-7.88860905221012E-30,
1.));
#13303=DIRECTION('ref_axis',(-0.989821441880934,-0.142314838273273,5.90481682637789E-30));
#13304=DIRECTION('center_axis',(7.09974814698911E-30,-7.88860905221012E-30,
1.));
#13305=DIRECTION('ref_axis',(-0.989821441880934,-0.142314838273273,5.90481682637789E-30));
#13306=DIRECTION('axis',(0.,0.,1.));
#13307=DIRECTION('refdir',(1.,0.,0.));
#13308=DIRECTION('center_axis',(0.,1.,0.));
#13309=DIRECTION('ref_axis',(0.,0.,1.));
#13310=DIRECTION('center_axis',(0.,1.,0.));
#13311=DIRECTION('ref_axis',(0.,0.,-1.));
#13312=DIRECTION('',(0.,1.,0.));
#13313=DIRECTION('center_axis',(0.,1.,0.));
#13314=DIRECTION('ref_axis',(0.,0.,1.));
#13315=DIRECTION('center_axis',(0.,0.,-1.));
#13316=DIRECTION('ref_axis',(-1.,0.,0.));
#13317=DIRECTION('center_axis',(0.,0.,-1.));
#13318=DIRECTION('ref_axis',(-1.,0.,0.));
#13319=DIRECTION('',(0.,0.,-1.));
#13320=DIRECTION('center_axis',(0.,0.,-1.));
#13321=DIRECTION('ref_axis',(-1.,0.,0.));
#13322=DIRECTION('center_axis',(1.,0.,0.));
#13323=DIRECTION('ref_axis',(0.,0.,1.));
#13324=DIRECTION('center_axis',(1.,0.,0.));
#13325=DIRECTION('ref_axis',(0.,0.,-1.));
#13326=DIRECTION('',(1.,0.,0.));
#13327=DIRECTION('center_axis',(-1.,0.,0.));
#13328=DIRECTION('ref_axis',(0.,0.,1.));
#13329=DIRECTION('center_axis',(1.,0.,0.));
#13330=DIRECTION('ref_axis',(0.,0.,1.));
#13331=DIRECTION('center_axis',(1.,0.,0.));
#13332=DIRECTION('ref_axis',(0.,0.,-1.));
#13333=DIRECTION('',(1.,0.,0.));
#13334=DIRECTION('center_axis',(-1.,0.,0.));
#13335=DIRECTION('ref_axis',(0.,0.,1.));
#13336=DIRECTION('center_axis',(1.,0.,0.));
#13337=DIRECTION('ref_axis',(0.,0.,1.));
#13338=DIRECTION('center_axis',(-1.,0.,0.));
#13339=DIRECTION('ref_axis',(0.,0.,1.));
#13340=DIRECTION('',(1.,0.,0.));
#13341=DIRECTION('center_axis',(-1.,0.,0.));
#13342=DIRECTION('ref_axis',(0.,0.,1.));
#13343=DIRECTION('center_axis',(1.,0.,0.));
#13344=DIRECTION('ref_axis',(0.,0.,1.));
#13345=DIRECTION('center_axis',(-1.,0.,0.));
#13346=DIRECTION('ref_axis',(0.,0.,1.));
#13347=DIRECTION('',(1.,0.,0.));
#13348=DIRECTION('center_axis',(-1.,0.,0.));
#13349=DIRECTION('ref_axis',(0.,0.,1.));
#13350=DIRECTION('center_axis',(0.,0.,-1.));
#13351=DIRECTION('ref_axis',(1.,0.,0.));
#13352=DIRECTION('center_axis',(0.,0.,1.));
#13353=DIRECTION('ref_axis',(1.,0.,0.));
#13354=DIRECTION('',(0.,0.,-1.));
#13355=DIRECTION('center_axis',(0.,0.,1.));
#13356=DIRECTION('ref_axis',(1.,0.,0.));
#13357=DIRECTION('center_axis',(0.,0.,-1.));
#13358=DIRECTION('ref_axis',(1.,0.,0.));
#13359=DIRECTION('center_axis',(0.,0.,1.));
#13360=DIRECTION('ref_axis',(1.,0.,0.));
#13361=DIRECTION('',(0.,0.,-1.));
#13362=DIRECTION('center_axis',(0.,0.,1.));
#13363=DIRECTION('ref_axis',(1.,0.,0.));
#13364=DIRECTION('center_axis',(0.,0.,-1.));
#13365=DIRECTION('ref_axis',(1.,0.,0.));
#13366=DIRECTION('center_axis',(0.,0.,1.));
#13367=DIRECTION('ref_axis',(1.,0.,0.));
#13368=DIRECTION('',(0.,0.,-1.));
#13369=DIRECTION('center_axis',(0.,0.,1.));
#13370=DIRECTION('ref_axis',(1.,0.,0.));
#13371=DIRECTION('center_axis',(0.,0.,-1.));
#13372=DIRECTION('ref_axis',(1.,0.,0.));
#13373=DIRECTION('center_axis',(0.,0.,1.));
#13374=DIRECTION('ref_axis',(1.,0.,0.));
#13375=DIRECTION('',(0.,0.,-1.));
#13376=DIRECTION('center_axis',(0.,0.,1.));
#13377=DIRECTION('ref_axis',(1.,0.,0.));
#13378=DIRECTION('center_axis',(0.,0.,-1.));
#13379=DIRECTION('ref_axis',(1.,0.,0.));
#13380=DIRECTION('center_axis',(0.,0.,1.));
#13381=DIRECTION('ref_axis',(1.,0.,0.));
#13382=DIRECTION('',(0.,0.,-1.));
#13383=DIRECTION('center_axis',(0.,0.,1.));
#13384=DIRECTION('ref_axis',(1.,0.,0.));
#13385=DIRECTION('center_axis',(0.,0.,-1.));
#13386=DIRECTION('ref_axis',(1.,0.,0.));
#13387=DIRECTION('center_axis',(0.,0.,1.));
#13388=DIRECTION('ref_axis',(1.,0.,0.));
#13389=DIRECTION('',(0.,0.,-1.));
#13390=DIRECTION('center_axis',(0.,0.,1.));
#13391=DIRECTION('ref_axis',(1.,0.,0.));
#13392=DIRECTION('center_axis',(0.,0.,-1.));
#13393=DIRECTION('ref_axis',(1.,0.,0.));
#13394=DIRECTION('center_axis',(0.,0.,1.));
#13395=DIRECTION('ref_axis',(1.,0.,0.));
#13396=DIRECTION('',(0.,0.,-1.));
#13397=DIRECTION('center_axis',(0.,0.,1.));
#13398=DIRECTION('ref_axis',(1.,0.,0.));
#13399=DIRECTION('center_axis',(0.,0.,1.));
#13400=DIRECTION('ref_axis',(-1.,0.,0.));
#13401=DIRECTION('',(1.,0.,0.));
#13402=DIRECTION('',(0.,-1.,0.));
#13403=DIRECTION('',(-1.,0.,0.));
#13404=DIRECTION('',(0.,1.,0.));
#13405=DIRECTION('',(1.,0.,0.));
#13406=DIRECTION('',(0.,1.,0.));
#13407=DIRECTION('',(-1.,0.,0.));
#13408=DIRECTION('',(0.,-1.,0.));
#13409=DIRECTION('center_axis',(0.,0.,1.));
#13410=DIRECTION('ref_axis',(-1.,0.,0.));
#13411=DIRECTION('',(-1.,0.,0.));
#13412=DIRECTION('',(0.,1.,0.));
#13413=DIRECTION('',(1.,0.,0.));
#13414=DIRECTION('',(0.,1.,0.));
#13415=DIRECTION('center_axis',(0.,0.,1.));
#13416=DIRECTION('ref_axis',(-1.,0.,0.));
#13417=DIRECTION('',(1.,0.,0.));
#13418=DIRECTION('',(0.,1.,0.));
#13419=DIRECTION('',(-1.,0.,0.));
#13420=DIRECTION('',(0.,1.,0.));
#13421=DIRECTION('center_axis',(0.,0.,1.));
#13422=DIRECTION('ref_axis',(-1.,0.,0.));
#13423=DIRECTION('',(1.,0.,0.));
#13424=DIRECTION('',(0.,-1.,0.));
#13425=DIRECTION('',(-1.,0.,0.));
#13426=DIRECTION('',(0.,-1.,0.));
#13427=DIRECTION('center_axis',(0.,0.,1.));
#13428=DIRECTION('ref_axis',(-1.,0.,0.));
#13429=DIRECTION('',(-1.,0.,0.));
#13430=DIRECTION('',(0.,-1.,0.));
#13431=DIRECTION('',(1.,0.,0.));
#13432=DIRECTION('',(0.,-1.,0.));
#13433=DIRECTION('center_axis',(-1.,0.,0.));
#13434=DIRECTION('ref_axis',(0.,0.,-1.));
#13435=DIRECTION('',(0.,0.,1.));
#13436=DIRECTION('center_axis',(-1.,0.,0.));
#13437=DIRECTION('ref_axis',(0.,0.,1.));
#13438=DIRECTION('center_axis',(-1.,0.,0.));
#13439=DIRECTION('ref_axis',(0.,0.,1.));
#13440=DIRECTION('center_axis',(-1.,0.,0.));
#13441=DIRECTION('ref_axis',(0.,0.,1.));
#13442=DIRECTION('',(0.,1.,0.));
#13443=DIRECTION('',(0.,0.,1.));
#13444=DIRECTION('',(0.,-1.,0.));
#13445=DIRECTION('center_axis',(0.,0.,1.));
#13446=DIRECTION('ref_axis',(-1.,0.,0.));
#13447=DIRECTION('',(-1.,0.,0.));
#13448=DIRECTION('',(0.,1.,0.));
#13449=DIRECTION('',(1.,-1.33440267382831E-16,0.));
#13450=DIRECTION('',(0.,-1.,0.));
#13451=DIRECTION('',(-1.,0.,0.));
#13452=DIRECTION('',(0.,-1.,0.));
#13453=DIRECTION('',(1.,0.,0.));
#13454=DIRECTION('center_axis',(1.,0.,0.));
#13455=DIRECTION('ref_axis',(0.,0.,1.));
#13456=DIRECTION('',(0.,0.,1.));
#13457=DIRECTION('center_axis',(-1.,0.,0.));
#13458=DIRECTION('ref_axis',(0.,0.,1.));
#13459=DIRECTION('center_axis',(-1.,0.,0.));
#13460=DIRECTION('ref_axis',(0.,0.,1.));
#13461=DIRECTION('center_axis',(-1.,0.,0.));
#13462=DIRECTION('ref_axis',(0.,0.,1.));
#13463=DIRECTION('',(0.,0.,1.));
#13464=DIRECTION('',(0.,1.,0.));
#13465=DIRECTION('center_axis',(0.,1.,0.));
#13466=DIRECTION('ref_axis',(0.,0.,-1.));
#13467=DIRECTION('',(-1.,0.,0.));
#13468=DIRECTION('center_axis',(0.,-1.,0.));
#13469=DIRECTION('ref_axis',(0.,0.,1.));
#13470=DIRECTION('',(1.,0.,0.));
#13471=DIRECTION('center_axis',(-1.,0.,0.));
#13472=DIRECTION('ref_axis',(0.,0.,-1.));
#13473=DIRECTION('center_axis',(1.,0.,0.));
#13474=DIRECTION('ref_axis',(0.,0.,-1.));
#13475=DIRECTION('',(0.,0.,1.));
#13476=DIRECTION('',(0.,1.,0.));
#13477=DIRECTION('',(0.,0.,1.));
#13478=DIRECTION('center_axis',(1.,0.,0.));
#13479=DIRECTION('ref_axis',(0.,0.,-1.));
#13480=DIRECTION('center_axis',(1.,0.,0.));
#13481=DIRECTION('ref_axis',(0.,0.,-1.));
#13482=DIRECTION('center_axis',(0.,-1.,0.));
#13483=DIRECTION('ref_axis',(0.,0.,1.));
#13484=DIRECTION('',(0.,0.,1.));
#13485=DIRECTION('',(-1.,0.,0.));
#13486=DIRECTION('center_axis',(1.,0.,0.));
#13487=DIRECTION('ref_axis',(0.,0.,1.));
#13488=DIRECTION('center_axis',(-1.,0.,0.));
#13489=DIRECTION('ref_axis',(0.,0.,1.));
#13490=DIRECTION('center_axis',(-1.,0.,0.));
#13491=DIRECTION('ref_axis',(0.,0.,1.));
#13492=DIRECTION('center_axis',(-1.,0.,0.));
#13493=DIRECTION('ref_axis',(0.,0.,1.));
#13494=DIRECTION('',(0.,0.,1.));
#13495=DIRECTION('',(0.,-1.,0.));
#13496=DIRECTION('center_axis',(1.33440267382831E-16,1.,0.));
#13497=DIRECTION('ref_axis',(-1.,1.33440267382831E-16,0.));
#13498=DIRECTION('',(1.,-1.33440267382831E-16,0.));
#13499=DIRECTION('center_axis',(0.,0.,-1.));
#13500=DIRECTION('ref_axis',(1.,0.,0.));
#13501=DIRECTION('center_axis',(0.,0.,-1.));
#13502=DIRECTION('ref_axis',(1.,0.,0.));
#13503=DIRECTION('',(-1.,0.,0.));
#13504=DIRECTION('',(0.,1.,0.));
#13505=DIRECTION('',(1.,0.,0.));
#13506=DIRECTION('',(0.,-1.,0.));
#13507=DIRECTION('center_axis',(1.,0.,0.));
#13508=DIRECTION('ref_axis',(0.,1.22464679914735E-16,-1.));
#13509=DIRECTION('center_axis',(1.,0.,0.));
#13510=DIRECTION('ref_axis',(0.,1.22464679914735E-16,-1.));
#13511=DIRECTION('center_axis',(1.,0.,0.));
#13512=DIRECTION('ref_axis',(0.,1.22464679914735E-16,-1.));
#13513=DIRECTION('center_axis',(1.,0.,0.));
#13514=DIRECTION('ref_axis',(0.,1.22464679914735E-16,-1.));
#13515=DIRECTION('center_axis',(1.,0.,0.));
#13516=DIRECTION('ref_axis',(0.,1.22464679914735E-16,-1.));
#13517=DIRECTION('center_axis',(1.,0.,0.));
#13518=DIRECTION('ref_axis',(0.,1.22464679914735E-16,-1.));
#13519=DIRECTION('center_axis',(0.,-1.,0.));
#13520=DIRECTION('ref_axis',(0.,0.,1.));
#13521=DIRECTION('center_axis',(0.707106781186549,0.707106781186546,-1.57296168257423E-15));
#13522=DIRECTION('ref_axis',(0.707106781186546,-0.707106781186549,9.32138197837028E-14));
#13523=DIRECTION('center_axis',(0.707106781186548,-0.707106781186548,0.));
#13524=DIRECTION('ref_axis',(0.707106781186548,0.707106781186548,4.73150009852597E-13));
#13525=DIRECTION('center_axis',(1.,0.,0.));
#13526=DIRECTION('ref_axis',(0.,0.,1.));
#13527=DIRECTION('center_axis',(0.707106781186548,0.707106781186548,0.));
#13528=DIRECTION('ref_axis',(0.707106781186548,-0.707106781186548,-1.54176894316072E-13));
#13529=DIRECTION('center_axis',(-1.,0.,0.));
#13530=DIRECTION('ref_axis',(0.,0.,-1.));
#13531=DIRECTION('center_axis',(0.707106781186552,-0.707106781186543,6.49701564541535E-15));
#13532=DIRECTION('ref_axis',(0.707106781186543,0.707106781186552,-3.8859613000266E-13));
#13533=DIRECTION('center_axis',(0.,1.,0.));
#13534=DIRECTION('ref_axis',(0.,0.,-1.));
#13535=DIRECTION('axis',(0.,0.,1.));
#13536=DIRECTION('refdir',(1.,0.,0.));
#13537=DIRECTION('center_axis',(-1.,0.,0.));
#13538=DIRECTION('ref_axis',(0.,0.,1.));
#13539=DIRECTION('',(0.,1.,0.));
#13540=DIRECTION('',(0.,0.,1.));
#13541=DIRECTION('',(0.,-1.,0.));
#13542=DIRECTION('',(0.,0.,-1.));
#13543=DIRECTION('center_axis',(0.,-1.,0.));
#13544=DIRECTION('ref_axis',(0.,0.,-1.));
#13545=DIRECTION('',(1.,0.,0.));
#13546=DIRECTION('',(0.,0.,-1.));
#13547=DIRECTION('',(-1.,0.,0.));
#13548=DIRECTION('',(0.,0.,1.));
#13549=DIRECTION('center_axis',(1.,0.,0.));
#13550=DIRECTION('ref_axis',(0.,0.,-1.));
#13551=DIRECTION('',(0.,1.,0.));
#13552=DIRECTION('',(0.,0.,-1.));
#13553=DIRECTION('',(0.,-1.,0.));
#13554=DIRECTION('',(0.,0.,1.));
#13555=DIRECTION('center_axis',(-4.42531498973675E-17,1.,0.));
#13556=DIRECTION('ref_axis',(-1.,-4.42531498973675E-17,0.));
#13557=DIRECTION('',(-1.,-4.42531498973675E-17,0.));
#13558=DIRECTION('',(0.,0.,-1.));
#13559=DIRECTION('',(1.,4.42531498973675E-17,0.));
#13560=DIRECTION('',(0.,0.,1.));
#13561=DIRECTION('center_axis',(0.,0.,-1.));
#13562=DIRECTION('ref_axis',(-1.,0.,0.));
#13563=DIRECTION('',(0.,1.,0.));
#13564=DIRECTION('',(-1.,0.,0.));
#13565=DIRECTION('',(0.,-1.,0.));
#13566=DIRECTION('',(1.,4.42531498973675E-17,0.));
#13567=DIRECTION('center_axis',(0.,0.,-1.));
#13568=DIRECTION('ref_axis',(-1.,0.,0.));
#13569=DIRECTION('',(0.,1.,0.));
#13570=DIRECTION('',(1.,0.,0.));
#13571=DIRECTION('',(0.,-1.,0.));
#13572=DIRECTION('',(-1.,-4.42531498973675E-17,0.));
#13573=DIRECTION('center_axis',(0.,-1.,0.));
#13574=DIRECTION('ref_axis',(0.,0.,-1.));
#13575=DIRECTION('center_axis',(0.,1.,0.));
#13576=DIRECTION('ref_axis',(0.,0.,1.));
#13577=DIRECTION('center_axis',(0.,-1.,0.));
#13578=DIRECTION('ref_axis',(0.,0.,-1.));
#13579=DIRECTION('center_axis',(0.,1.,0.));
#13580=DIRECTION('ref_axis',(-1.,0.,0.));
#13581=DIRECTION('center_axis',(0.,0.,1.));
#13582=DIRECTION('ref_axis',(-1.,0.,0.));
#13583=DIRECTION('center_axis',(-1.,1.73472347597681E-15,0.));
#13584=DIRECTION('ref_axis',(1.73472347597681E-15,1.,0.));
#13585=DIRECTION('center_axis',(0.,1.,-1.11022302462516E-16));
#13586=DIRECTION('ref_axis',(1.77635683940025E-15,0.,-1.));
#13587=DIRECTION('center_axis',(-1.,0.,0.));
#13588=DIRECTION('ref_axis',(0.,0.,-1.));
#13589=DIRECTION('center_axis',(0.,0.,1.));
#13590=DIRECTION('ref_axis',(-1.,0.,0.));
#13591=DIRECTION('center_axis',(1.,0.,0.));
#13592=DIRECTION('ref_axis',(0.,0.,-1.));
#13593=DIRECTION('center_axis',(-1.,0.,0.));
#13594=DIRECTION('ref_axis',(0.,0.,1.));
#13595=DIRECTION('center_axis',(0.,0.,-1.));
#13596=DIRECTION('ref_axis',(-1.,0.,0.));
#13597=DIRECTION('center_axis',(0.,0.,1.));
#13598=DIRECTION('ref_axis',(1.,0.,0.));
#13599=DIRECTION('center_axis',(0.,1.,0.));
#13600=DIRECTION('ref_axis',(0.,0.,1.));
#13601=DIRECTION('center_axis',(0.,-1.,0.));
#13602=DIRECTION('ref_axis',(0.,0.,-1.));
#13603=DIRECTION('center_axis',(0.,1.,0.));
#13604=DIRECTION('ref_axis',(0.,0.,1.));
#13605=DIRECTION('center_axis',(0.,0.,-1.));
#13606=DIRECTION('ref_axis',(-1.,0.,0.));
#13607=DIRECTION('center_axis',(0.,0.,1.));
#13608=DIRECTION('ref_axis',(1.,0.,0.));
#13609=DIRECTION('center_axis',(-1.,-4.42531498973675E-17,0.));
#13610=DIRECTION('ref_axis',(4.42531498973675E-17,-1.,0.));
#13611=DIRECTION('center_axis',(-1.,0.,0.));
#13612=DIRECTION('ref_axis',(0.,0.,1.));
#13613=DIRECTION('center_axis',(0.,1.,0.));
#13614=DIRECTION('ref_axis',(0.,0.,1.));
#13615=DIRECTION('center_axis',(-8.67361737988404E-16,1.,0.));
#13616=DIRECTION('ref_axis',(-1.,-8.67361737988404E-16,0.));
#13617=DIRECTION('center_axis',(0.,-1.,0.));
#13618=DIRECTION('ref_axis',(0.,0.,-1.));
#13619=DIRECTION('center_axis',(0.,1.,0.));
#13620=DIRECTION('ref_axis',(-1.,0.,0.));
#13621=DIRECTION('center_axis',(0.,0.,1.));
#13622=DIRECTION('ref_axis',(-1.,0.,0.));
#13623=DIRECTION('center_axis',(0.,1.,0.));
#13624=DIRECTION('ref_axis',(0.,0.,-1.));
#13625=DIRECTION('center_axis',(-1.,0.,-1.73472347597681E-15));
#13626=DIRECTION('ref_axis',(1.73472347597681E-15,0.,-1.));
#13627=DIRECTION('center_axis',(0.,1.,0.));
#13628=DIRECTION('ref_axis',(0.,0.,-1.));
#13629=DIRECTION('center_axis',(-1.,0.,0.));
#13630=DIRECTION('ref_axis',(0.,0.,-1.));
#13631=DIRECTION('center_axis',(0.,1.,0.));
#13632=DIRECTION('ref_axis',(-1.,0.,0.));
#13633=DIRECTION('center_axis',(0.,0.,1.));
#13634=DIRECTION('ref_axis',(-1.,0.,0.));
#13635=DIRECTION('center_axis',(0.,0.,-1.));
#13636=DIRECTION('ref_axis',(-1.,0.,0.));
#13637=DIRECTION('center_axis',(0.,0.,1.));
#13638=DIRECTION('ref_axis',(1.,0.,0.));
#13639=DIRECTION('center_axis',(-1.,0.,0.));
#13640=DIRECTION('ref_axis',(0.,0.,1.));
#13641=DIRECTION('center_axis',(-1.,0.,0.));
#13642=DIRECTION('ref_axis',(0.,0.,1.));
#13643=DIRECTION('center_axis',(1.,4.42531498973675E-17,0.));
#13644=DIRECTION('ref_axis',(-4.42531498973675E-17,1.,0.));
#13645=DIRECTION('center_axis',(-1.,0.,0.));
#13646=DIRECTION('ref_axis',(0.,0.,1.));
#13647=DIRECTION('center_axis',(0.,0.,-1.));
#13648=DIRECTION('ref_axis',(-1.,0.,0.));
#13649=DIRECTION('center_axis',(0.,0.,1.));
#13650=DIRECTION('ref_axis',(1.,0.,0.));
#13651=DIRECTION('center_axis',(1.,0.,0.));
#13652=DIRECTION('ref_axis',(0.,0.,1.));
#13653=DIRECTION('center_axis',(0.,-1.,8.67361737988403E-16));
#13654=DIRECTION('ref_axis',(0.,8.67361737988403E-16,1.));
#13655=DIRECTION('center_axis',(1.,0.,0.));
#13656=DIRECTION('ref_axis',(0.,0.,-1.));
#13657=DIRECTION('center_axis',(0.,1.,0.));
#13658=DIRECTION('ref_axis',(0.,0.,-1.));
#13659=DIRECTION('center_axis',(0.,-1.,0.));
#13660=DIRECTION('ref_axis',(0.,0.,-1.));
#13661=DIRECTION('axis',(0.,0.,1.));
#13662=DIRECTION('refdir',(1.,0.,0.));
#13663=DIRECTION('center_axis',(0.,0.,-1.));
#13664=DIRECTION('ref_axis',(-1.,0.,0.));
#13665=DIRECTION('center_axis',(0.,0.,1.));
#13666=DIRECTION('ref_axis',(1.,0.,0.));
#13667=DIRECTION('',(0.,0.,-1.));
#13668=DIRECTION('center_axis',(0.,0.,1.));
#13669=DIRECTION('ref_axis',(1.,0.,0.));
#13670=DIRECTION('center_axis',(0.,0.,-1.));
#13671=DIRECTION('ref_axis',(-1.,0.,0.));
#13672=DIRECTION('center_axis',(0.,0.,1.));
#13673=DIRECTION('ref_axis',(1.,0.,0.));
#13674=DIRECTION('',(0.,0.,-1.));
#13675=DIRECTION('center_axis',(0.,0.,1.));
#13676=DIRECTION('ref_axis',(1.,0.,0.));
#13677=DIRECTION('center_axis',(0.,0.,-1.));
#13678=DIRECTION('ref_axis',(-1.,0.,0.));
#13679=DIRECTION('center_axis',(0.,0.,1.));
#13680=DIRECTION('ref_axis',(1.,0.,0.));
#13681=DIRECTION('',(0.,0.,-1.));
#13682=DIRECTION('center_axis',(0.,0.,1.));
#13683=DIRECTION('ref_axis',(1.,0.,0.));
#13684=DIRECTION('center_axis',(0.,0.,-1.));
#13685=DIRECTION('ref_axis',(-1.,0.,0.));
#13686=DIRECTION('center_axis',(0.,0.,1.));
#13687=DIRECTION('ref_axis',(1.,0.,0.));
#13688=DIRECTION('',(0.,0.,-1.));
#13689=DIRECTION('center_axis',(0.,0.,1.));
#13690=DIRECTION('ref_axis',(1.,0.,0.));
#13691=DIRECTION('center_axis',(0.,0.,-1.));
#13692=DIRECTION('ref_axis',(-1.,0.,0.));
#13693=DIRECTION('center_axis',(0.,0.,1.));
#13694=DIRECTION('ref_axis',(1.,0.,0.));
#13695=DIRECTION('',(0.,0.,-1.));
#13696=DIRECTION('center_axis',(0.,0.,1.));
#13697=DIRECTION('ref_axis',(1.,0.,0.));
#13698=DIRECTION('center_axis',(0.,0.,-1.));
#13699=DIRECTION('ref_axis',(-1.,0.,0.));
#13700=DIRECTION('center_axis',(0.,0.,1.));
#13701=DIRECTION('ref_axis',(1.,0.,0.));
#13702=DIRECTION('',(0.,0.,-1.));
#13703=DIRECTION('center_axis',(0.,0.,1.));
#13704=DIRECTION('ref_axis',(1.,0.,0.));
#13705=DIRECTION('center_axis',(0.,0.,-1.));
#13706=DIRECTION('ref_axis',(-1.,0.,0.));
#13707=DIRECTION('center_axis',(0.,0.,1.));
#13708=DIRECTION('ref_axis',(1.,0.,0.));
#13709=DIRECTION('',(0.,0.,-1.));
#13710=DIRECTION('center_axis',(0.,0.,1.));
#13711=DIRECTION('ref_axis',(1.,0.,0.));
#13712=DIRECTION('center_axis',(0.,0.,-1.));
#13713=DIRECTION('ref_axis',(-1.,0.,0.));
#13714=DIRECTION('center_axis',(0.,0.,1.));
#13715=DIRECTION('ref_axis',(1.,0.,0.));
#13716=DIRECTION('',(0.,0.,1.));
#13717=DIRECTION('center_axis',(0.,0.,1.));
#13718=DIRECTION('ref_axis',(1.,0.,0.));
#13719=DIRECTION('center_axis',(0.,0.,1.));
#13720=DIRECTION('ref_axis',(1.,0.,0.));
#13721=DIRECTION('center_axis',(0.,0.,1.));
#13722=DIRECTION('ref_axis',(1.,0.,0.));
#13723=DIRECTION('axis',(0.,0.,1.));
#13724=DIRECTION('refdir',(1.,0.,0.));
#13725=DIRECTION('center_axis',(-2.36658271566304E-30,1.04667633103075E-31,
-1.));
#13726=DIRECTION('ref_axis',(-1.,-2.47704611391098E-61,2.36658271566304E-30));
#13727=DIRECTION('center_axis',(2.36658271566304E-30,-1.04667633103075E-31,
1.));
#13728=DIRECTION('ref_axis',(1.,2.47704611391098E-61,-2.36658271566304E-30));
#13729=DIRECTION('',(-2.36658271566304E-30,1.04667633103075E-31,-1.));
#13730=DIRECTION('center_axis',(2.36658271566304E-30,-1.04667633103075E-31,
1.));
#13731=DIRECTION('ref_axis',(1.,2.47704611391098E-61,-2.36658271566304E-30));
#13732=DIRECTION('center_axis',(-2.36658271566304E-30,1.04667633103075E-31,
-1.));
#13733=DIRECTION('ref_axis',(-1.,-2.47704611391098E-61,2.36658271566304E-30));
#13734=DIRECTION('center_axis',(2.36658271566304E-30,-1.04667633103075E-31,
1.));
#13735=DIRECTION('ref_axis',(1.,2.47704611391098E-61,-2.36658271566304E-30));
#13736=DIRECTION('',(-2.36658271566304E-30,1.04667633103075E-31,-1.));
#13737=DIRECTION('center_axis',(2.36658271566304E-30,-1.04667633103075E-31,
1.));
#13738=DIRECTION('ref_axis',(1.,2.47704611391098E-61,-2.36658271566304E-30));
#13739=DIRECTION('center_axis',(-2.36658271566304E-30,1.04667633103075E-31,
-1.));
#13740=DIRECTION('ref_axis',(-1.,-2.47704611391098E-61,2.36658271566304E-30));
#13741=DIRECTION('center_axis',(2.36658271566304E-30,-1.04667633103075E-31,
1.));
#13742=DIRECTION('ref_axis',(1.,2.47704611391098E-61,-2.36658271566304E-30));
#13743=DIRECTION('',(-2.36658271566304E-30,1.04667633103075E-31,-1.));
#13744=DIRECTION('center_axis',(2.36658271566304E-30,-1.04667633103075E-31,
1.));
#13745=DIRECTION('ref_axis',(1.,2.47704611391098E-61,-2.36658271566304E-30));
#13746=DIRECTION('center_axis',(-2.36658271566304E-30,1.04667633103075E-31,
-1.));
#13747=DIRECTION('ref_axis',(-1.,-2.47704611391098E-61,2.36658271566304E-30));
#13748=DIRECTION('center_axis',(2.36658271566304E-30,-1.04667633103075E-31,
1.));
#13749=DIRECTION('ref_axis',(1.,2.47704611391098E-61,-2.36658271566304E-30));
#13750=DIRECTION('',(-2.36658271566304E-30,1.04667633103075E-31,-1.));
#13751=DIRECTION('center_axis',(2.36658271566304E-30,-1.04667633103075E-31,
1.));
#13752=DIRECTION('ref_axis',(1.,2.47704611391098E-61,-2.36658271566304E-30));
#13753=DIRECTION('center_axis',(-2.36658271566304E-30,1.04667633103075E-31,
-1.));
#13754=DIRECTION('ref_axis',(-1.,-2.47704611391098E-61,2.36658271566304E-30));
#13755=DIRECTION('center_axis',(2.36658271566304E-30,-1.04667633103075E-31,
1.));
#13756=DIRECTION('ref_axis',(1.,2.47704611391098E-61,-2.36658271566304E-30));
#13757=DIRECTION('',(-2.36658271566304E-30,1.04667633103075E-31,-1.));
#13758=DIRECTION('center_axis',(2.36658271566304E-30,-1.04667633103075E-31,
1.));
#13759=DIRECTION('ref_axis',(1.,2.47704611391098E-61,-2.36658271566304E-30));
#13760=DIRECTION('center_axis',(-2.36658271566304E-30,1.04667633103075E-31,
-1.));
#13761=DIRECTION('ref_axis',(-1.,-2.47704611391098E-61,2.36658271566304E-30));
#13762=DIRECTION('center_axis',(2.36658271566304E-30,-1.04667633103075E-31,
1.));
#13763=DIRECTION('ref_axis',(1.,2.47704611391098E-61,-2.36658271566304E-30));
#13764=DIRECTION('',(-2.36658271566304E-30,1.04667633103075E-31,-1.));
#13765=DIRECTION('center_axis',(2.36658271566304E-30,-1.04667633103075E-31,
1.));
#13766=DIRECTION('ref_axis',(1.,2.47704611391098E-61,-2.36658271566304E-30));
#13767=DIRECTION('center_axis',(-2.36658271566304E-30,1.04667633103075E-31,
-1.));
#13768=DIRECTION('ref_axis',(-1.,-2.47704611391098E-61,2.36658271566304E-30));
#13769=DIRECTION('center_axis',(2.36658271566304E-30,-1.04667633103075E-31,
1.));
#13770=DIRECTION('ref_axis',(1.,2.47704611391098E-61,-2.36658271566304E-30));
#13771=DIRECTION('',(-2.36658271566304E-30,1.04667633103075E-31,-1.));
#13772=DIRECTION('center_axis',(2.36658271566304E-30,-1.04667633103075E-31,
1.));
#13773=DIRECTION('ref_axis',(1.,2.47704611391098E-61,-2.36658271566304E-30));
#13774=DIRECTION('center_axis',(-2.36658271566304E-30,1.04667633103075E-31,
-1.));
#13775=DIRECTION('ref_axis',(-1.,-2.47704611391098E-61,2.36658271566304E-30));
#13776=DIRECTION('center_axis',(2.36658271566304E-30,-1.04667633103075E-31,
1.));
#13777=DIRECTION('ref_axis',(1.,2.47704611391098E-61,-2.36658271566304E-30));
#13778=DIRECTION('',(2.36658271566304E-30,-1.04667633103075E-31,1.));
#13779=DIRECTION('center_axis',(2.36658271566304E-30,-1.04667633103075E-31,
1.));
#13780=DIRECTION('ref_axis',(1.,2.47704611391098E-61,-2.36658271566304E-30));
#13781=DIRECTION('center_axis',(-2.36658271566304E-30,-1.04667633103075E-31,
1.));
#13782=DIRECTION('ref_axis',(1.,0.,2.36658271566304E-30));
#13783=DIRECTION('center_axis',(-2.36658271566304E-30,-1.04667633103075E-31,
1.));
#13784=DIRECTION('ref_axis',(1.,0.,2.36658271566304E-30));
#13785=DIRECTION('axis',(0.,0.,1.));
#13786=DIRECTION('refdir',(1.,0.,0.));
#13787=DIRECTION('center_axis',(4.71519812073164E-16,9.75250265821225E-17,
-1.));
#13788=DIRECTION('ref_axis',(-1.,-1.38777878078144E-16,-4.71519812073164E-16));
#13789=DIRECTION('center_axis',(4.71519812073164E-16,9.75250265821225E-17,
-1.));
#13790=DIRECTION('ref_axis',(1.,-5.19029264012261E-15,4.71519812073163E-16));
#13791=DIRECTION('',(-0.707106781186547,-8.04957806758036E-17,0.707106781186548));
#13792=DIRECTION('center_axis',(-4.71519812073164E-16,-9.75250265821225E-17,
1.));
#13793=DIRECTION('ref_axis',(1.,1.38777878078144E-16,4.71519812073164E-16));
#13794=DIRECTION('center_axis',(4.71519812073164E-16,9.75250265821225E-17,
-1.));
#13795=DIRECTION('ref_axis',(-1.,-1.38777878078145E-16,-4.44089209850063E-16));
#13796=DIRECTION('center_axis',(4.71519812073164E-16,9.75250265821225E-17,
-1.));
#13797=DIRECTION('ref_axis',(-1.,-1.38777878078143E-16,-4.71519812073164E-16));
#13798=DIRECTION('center_axis',(1.63131981634091E-17,-1.,-9.75250265821225E-17));
#13799=DIRECTION('ref_axis',(1.,1.6313198163409E-17,4.44089209850063E-16));
#13800=DIRECTION('center_axis',(-4.71519812073164E-16,-9.75250265821225E-17,
1.));
#13801=DIRECTION('ref_axis',(-1.,6.07847105982273E-15,-4.71519812073163E-16));
#13802=DIRECTION('center_axis',(-4.71519812073164E-16,-9.75250265821225E-17,
1.));
#13803=DIRECTION('ref_axis',(-1.,6.07847105982273E-15,-4.71519812073163E-16));
#13804=DIRECTION('center_axis',(-4.71519812073164E-16,-9.75250265821225E-17,
1.));
#13805=DIRECTION('ref_axis',(1.,1.38777878078144E-16,4.71519812073164E-16));
#13806=DIRECTION('center_axis',(4.71519812073164E-16,9.75250265821225E-17,
-1.));
#13807=DIRECTION('ref_axis',(-1.,-1.38777878078144E-16,-4.71519812073164E-16));
#13808=DIRECTION('',(4.71519812073164E-16,9.75250265821225E-17,-1.));
#13809=DIRECTION('center_axis',(4.71519812073164E-16,9.75250265821225E-17,
-1.));
#13810=DIRECTION('ref_axis',(-1.,-1.38777878078144E-16,-4.71519812073164E-16));
#13811=DIRECTION('center_axis',(-4.71519812073164E-16,-9.75250265821225E-17,
1.));
#13812=DIRECTION('ref_axis',(1.,1.38777878078144E-16,4.71519812073164E-16));
#13813=DIRECTION('',(-4.71519812073164E-16,-9.75250265821225E-17,1.));
#13814=DIRECTION('center_axis',(4.71519812073163E-16,-9.75250265821224E-17,
1.));
#13815=DIRECTION('ref_axis',(1.,1.38777878078144E-16,-4.71519812073163E-16));
#13816=DIRECTION('center_axis',(-4.71519812073163E-16,9.75250265821224E-17,
-1.));
#13817=DIRECTION('ref_axis',(-1.,-1.38777878078144E-16,4.71519812073163E-16));
#13818=DIRECTION('center_axis',(-4.71519812073163E-16,9.75250265821224E-17,
-1.));
#13819=DIRECTION('ref_axis',(-1.,-1.38777878078144E-16,4.71519812073163E-16));
#13820=DIRECTION('axis',(0.,0.,1.));
#13821=DIRECTION('refdir',(1.,0.,0.));
#13822=DIRECTION('center_axis',(0.,0.,1.));
#13823=DIRECTION('ref_axis',(1.,0.,0.));
#13824=DIRECTION('center_axis',(0.,0.,-1.));
#13825=DIRECTION('ref_axis',(-1.,0.,0.));
#13826=DIRECTION('',(0.,0.,-1.));
#13827=DIRECTION('center_axis',(0.,0.,-1.));
#13828=DIRECTION('ref_axis',(-1.,0.,0.));
#13829=DIRECTION('center_axis',(1.,-1.87789324842145E-16,0.));
#13830=DIRECTION('ref_axis',(1.87789324842145E-16,1.,0.));
#13831=DIRECTION('',(1.87789324842145E-16,1.,0.));
#13832=DIRECTION('',(0.,0.,1.));
#13833=DIRECTION('',(1.87789324842145E-16,1.,0.));
#13834=DIRECTION('',(0.,0.,1.));
#13835=DIRECTION('center_axis',(0.5,-0.866025403784439,0.));
#13836=DIRECTION('ref_axis',(0.866025403784439,0.5,0.));
#13837=DIRECTION('',(0.866025403784439,0.5,0.));
#13838=DIRECTION('',(0.,0.,1.));
#13839=DIRECTION('',(0.866025403784439,0.5,0.));
#13840=DIRECTION('center_axis',(-0.5,-0.866025403784439,0.));
#13841=DIRECTION('ref_axis',(0.866025403784439,-0.5,0.));
#13842=DIRECTION('',(0.866025403784438,-0.5,0.));
#13843=DIRECTION('',(0.,0.,1.));
#13844=DIRECTION('',(0.866025403784438,-0.5,0.));
#13845=DIRECTION('center_axis',(-1.,0.,0.));
#13846=DIRECTION('ref_axis',(0.,0.,1.));
#13847=DIRECTION('',(0.,-1.,0.));
#13848=DIRECTION('',(0.,0.,1.));
#13849=DIRECTION('',(0.,-1.,0.));
#13850=DIRECTION('center_axis',(-0.5,0.866025403784439,0.));
#13851=DIRECTION('ref_axis',(-0.866025403784439,-0.5,0.));
#13852=DIRECTION('',(-0.866025403784439,-0.5,0.));
#13853=DIRECTION('',(0.,0.,1.));
#13854=DIRECTION('',(-0.866025403784439,-0.5,0.));
#13855=DIRECTION('center_axis',(0.5,0.866025403784439,0.));
#13856=DIRECTION('ref_axis',(-0.866025403784439,0.5,0.));
#13857=DIRECTION('',(-0.866025403784439,0.5,0.));
#13858=DIRECTION('',(-0.866025403784439,0.5,0.));
#13859=DIRECTION('center_axis',(0.,0.,1.));
#13860=DIRECTION('ref_axis',(1.,0.,0.));
#13861=DIRECTION('center_axis',(0.,0.,1.));
#13862=DIRECTION('ref_axis',(1.,0.,0.));
#13863=DIRECTION('center_axis',(0.,0.,-1.));
#13864=DIRECTION('ref_axis',(-1.,0.,0.));
#13865=DIRECTION('axis',(0.,0.,1.));
#13866=DIRECTION('refdir',(1.,0.,0.));
#13867=DIRECTION('center_axis',(0.,-1.,0.));
#13868=DIRECTION('ref_axis',(0.,0.,-1.));
#13869=DIRECTION('',(1.,0.,0.));
#13870=DIRECTION('',(0.,0.,1.));
#13871=DIRECTION('',(1.,0.,0.));
#13872=DIRECTION('',(0.,0.,-1.));
#13873=DIRECTION('center_axis',(-1.,0.,0.));
#13874=DIRECTION('ref_axis',(0.,0.,1.));
#13875=DIRECTION('',(0.,-1.,0.));
#13876=DIRECTION('',(0.,0.,-1.));
#13877=DIRECTION('',(0.,-1.,0.));
#13878=DIRECTION('',(0.,0.,1.));
#13879=DIRECTION('center_axis',(0.,1.,0.));
#13880=DIRECTION('ref_axis',(0.,0.,1.));
#13881=DIRECTION('',(-1.,0.,0.));
#13882=DIRECTION('',(0.,0.,-1.));
#13883=DIRECTION('',(-1.,0.,0.));
#13884=DIRECTION('',(0.,0.,1.));
#13885=DIRECTION('center_axis',(1.,7.70988211545248E-17,0.));
#13886=DIRECTION('ref_axis',(-7.70988211545248E-17,1.,0.));
#13887=DIRECTION('',(-7.70988211545248E-17,1.,0.));
#13888=DIRECTION('',(0.,0.,1.));
#13889=DIRECTION('',(-7.70988211545248E-17,1.,0.));
#13890=DIRECTION('',(0.,0.,1.));
#13891=DIRECTION('center_axis',(4.33680868994202E-16,-1.,0.));
#13892=DIRECTION('ref_axis',(1.,4.33680868994202E-16,0.));
#13893=DIRECTION('',(1.,4.33680868994202E-16,0.));
#13894=DIRECTION('',(0.,0.,1.));
#13895=DIRECTION('',(1.,4.33680868994202E-16,0.));
#13896=DIRECTION('center_axis',(-1.,0.,0.));
#13897=DIRECTION('ref_axis',(0.,0.,1.));
#13898=DIRECTION('',(0.,-1.,0.));
#13899=DIRECTION('',(0.,0.,-1.));
#13900=DIRECTION('',(0.,-1.,0.));
#13901=DIRECTION('center_axis',(1.73472347597681E-16,-1.,0.));
#13902=DIRECTION('ref_axis',(1.,1.73472347597681E-16,0.));
#13903=DIRECTION('',(1.,1.73472347597681E-16,0.));
#13904=DIRECTION('',(0.,0.,1.));
#13905=DIRECTION('',(1.,1.73472347597681E-16,0.));
#13906=DIRECTION('',(0.,0.,-1.));
#13907=DIRECTION('center_axis',(1.,1.44560289664734E-16,0.));
#13908=DIRECTION('ref_axis',(-1.44560289664734E-16,1.,0.));
#13909=DIRECTION('',(-1.44560289664734E-16,1.,0.));
#13910=DIRECTION('',(0.,0.,1.));
#13911=DIRECTION('',(-1.44560289664734E-16,1.,0.));
#13912=DIRECTION('',(0.,0.,-1.));
#13913=DIRECTION('center_axis',(0.,0.,-1.));
#13914=DIRECTION('ref_axis',(-1.,0.,0.));
#13915=DIRECTION('',(0.707106781186549,-0.707106781186546,0.));
#13916=DIRECTION('',(-0.707106781186551,0.707106781186544,0.));
#13917=DIRECTION('',(-0.707106781186545,-0.70710678118655,0.));
#13918=DIRECTION('',(-0.707106781186545,-0.70710678118655,0.));
#13919=DIRECTION('',(-0.70710678118655,0.707106781186545,0.));
#13920=DIRECTION('',(0.707106781186545,0.70710678118655,0.));
#13921=DIRECTION('center_axis',(0.,0.,-1.));
#13922=DIRECTION('ref_axis',(-1.,0.,0.));
#13923=DIRECTION('',(-0.707106781186549,0.707106781186546,0.));
#13924=DIRECTION('',(-0.707106781186545,-0.70710678118655,0.));
#13925=DIRECTION('',(0.70710678118655,-0.707106781186545,0.));
#13926=DIRECTION('',(0.707106781186545,0.70710678118655,0.));
#13927=DIRECTION('',(0.707106781186545,0.70710678118655,0.));
#13928=DIRECTION('',(0.707106781186551,-0.707106781186544,0.));
#13929=DIRECTION('center_axis',(-0.707106781186546,-0.707106781186549,0.));
#13930=DIRECTION('ref_axis',(0.,0.,1.));
#13931=DIRECTION('center_axis',(0.70710678118655,-0.707106781186545,0.));
#13932=DIRECTION('ref_axis',(0.,0.,1.));
#13933=DIRECTION('center_axis',(-0.707106781186544,-0.707106781186551,0.));
#13934=DIRECTION('ref_axis',(0.,0.,-1.));
#13935=DIRECTION('center_axis',(0.70710678118655,-0.707106781186545,0.));
#13936=DIRECTION('ref_axis',(0.,0.,-1.));
#13937=DIRECTION('center_axis',(-0.70710678118655,0.707106781186545,0.));
#13938=DIRECTION('ref_axis',(0.,0.,1.));
#13939=DIRECTION('center_axis',(0.707106781186545,0.70710678118655,0.));
#13940=DIRECTION('ref_axis',(0.,0.,1.));
#13941=DIRECTION('axis',(0.,0.,1.));
#13942=DIRECTION('refdir',(1.,0.,0.));
#13943=DIRECTION('center_axis',(1.49883571991992E-29,3.54987407349455E-30,
1.));
#13944=DIRECTION('ref_axis',(1.,-1.26016059376688E-58,-1.49883571991992E-29));
#13945=DIRECTION('center_axis',(1.49883571991992E-29,3.54987407349455E-30,
1.));
#13946=DIRECTION('ref_axis',(1.,-5.32067806257128E-59,-1.49883571991992E-29));
#13947=DIRECTION('',(1.49883571991992E-29,3.54987407349455E-30,1.));
#13948=DIRECTION('center_axis',(1.49883571991992E-29,3.54987407349455E-30,
1.));
#13949=DIRECTION('ref_axis',(1.,-1.26016059376688E-58,-1.49883571991992E-29));
#13950=DIRECTION('center_axis',(1.49883571991992E-29,3.54987407349455E-30,
1.));
#13951=DIRECTION('ref_axis',(1.,-1.26016059376688E-58,-1.49883571991992E-29));
#13952=DIRECTION('center_axis',(1.49883571991992E-29,3.54987407349455E-30,
1.));
#13953=DIRECTION('ref_axis',(1.,-1.26016059376688E-58,-1.49883571991992E-29));
#13954=DIRECTION('',(-1.49883571991992E-29,-3.54987407349455E-30,-1.));
#13955=DIRECTION('center_axis',(1.49883571991992E-29,3.54987407349455E-30,
1.));
#13956=DIRECTION('ref_axis',(1.,-5.32067806257128E-59,-1.49883571991992E-29));
#13957=DIRECTION('center_axis',(2.05103835357463E-29,-3.54987407349455E-30,
-1.));
#13958=DIRECTION('ref_axis',(-1.,0.,-2.05103835357463E-29));
#13959=DIRECTION('center_axis',(-2.05103835357463E-29,3.54987407349455E-30,
1.));
#13960=DIRECTION('ref_axis',(1.,0.,2.05103835357463E-29));
#13961=DIRECTION('',(-6.98296267768627E-15,0.,-1.));
#13962=DIRECTION('',(-1.,0.,6.98296267768627E-15));
#13963=DIRECTION('',(-3.60027924974532E-15,-0.830365262741516,-0.557219463436278));
#13964=DIRECTION('',(1.,-8.01582463471311E-16,-5.26663767047608E-15));
#13965=DIRECTION('',(-0.820639210278119,0.571446661162794,6.84963850913457E-15));
#13966=DIRECTION('',(7.39419330527966E-15,-1.36788541708432E-15,1.));
#13967=DIRECTION('',(7.458509453054E-15,1.65223496030256E-17,1.));
#13968=DIRECTION('',(0.820639210278118,-0.571446661162795,-6.11130366589091E-15));
#13969=DIRECTION('',(1.,-2.7791136476792E-18,-6.98309053539866E-15));
#13970=DIRECTION('',(-6.98309053539866E-15,-7.21644966006352E-16,-1.));
#13971=DIRECTION('',(-6.98296267768627E-15,0.,-1.));
#13972=DIRECTION('',(-1.,0.,6.98296267768627E-15));
#13973=DIRECTION('',(-6.99440505513849E-15,1.30104260698254E-18,-1.));
#13974=DIRECTION('',(-0.945873500394443,-0.32453554697685,6.61540015810633E-15));
#13975=DIRECTION('',(7.39419330527954E-15,-1.36788541708467E-15,1.));
#13976=DIRECTION('',(0.820639210278119,-0.571446661162794,-6.84963850913467E-15));
#13977=DIRECTION('',(-1.,2.77911365296838E-18,6.98309053539402E-15));
#13978=DIRECTION('',(6.98309053539402E-15,-3.69245429642865E-41,1.));
#13979=DIRECTION('',(0.,0.,1.));
#13980=DIRECTION('',(1.,0.,0.));
#13981=DIRECTION('',(0.,0.,1.));
#13982=DIRECTION('',(1.,0.,0.));
#13983=DIRECTION('',(1.,1.48150879974396E-17,-6.89267343525292E-15));
#13984=DIRECTION('',(-6.81548361256536E-15,-0.147128308448788,-0.98911741509944));
#13985=DIRECTION('',(1.,-2.77911364767131E-18,-6.98309053539862E-15));
#13986=DIRECTION('',(-6.98309053539862E-15,1.16989751219876E-14,-1.));
#13987=DIRECTION('',(-2.16840434497101E-19,-1.,2.87539977523829E-36));
#13988=DIRECTION('',(0.982190357743813,-2.12978583932031E-19,0.187888533857391));
#13989=DIRECTION('',(-1.,2.77911364633405E-18,6.98309053539173E-15));
#13990=DIRECTION('',(3.49395205071358E-15,0.86602540378444,0.499999999999998));
#13991=DIRECTION('',(-1.,2.77911364103947E-18,6.98309053539633E-15));
#13992=DIRECTION('',(-3.48913848468505E-15,0.866025403784436,-0.500000000000004));
#13993=DIRECTION('',(-1.,2.77911364237445E-18,6.98309053540322E-15));
#13994=DIRECTION('',(-6.98309053540322E-15,-6.98296267768627E-15,-1.));
#13995=DIRECTION('',(-1.,2.77911364900858E-18,6.98309053540551E-15));
#13996=DIRECTION('',(-3.49395205072274E-15,-0.866025403784443,-0.499999999999992));
#13997=DIRECTION('',(-1.,2.779113654306E-18,6.98309053540091E-15));
#13998=DIRECTION('',(3.48913848467589E-15,-0.866025403784433,0.50000000000001));
#13999=DIRECTION('',(1.,-1.39865826688389E-16,-7.04349926140452E-15));
#14000=DIRECTION('',(-6.0507154842071E-15,-0.529127184365614,-0.848542528554295));
#14001=DIRECTION('',(1.,1.14449903309839E-15,-5.42627044917174E-15));
#14002=DIRECTION('',(-5.32698476299264E-15,0.470295793736697,-0.882508847770701));
#14003=DIRECTION('',(1.,3.86120227866043E-16,-3.50536344675197E-15));
#14004=DIRECTION('',(-5.04961721841306E-16,0.999422978102309,-0.0339663192164017));
#14005=DIRECTION('',(1.,-1.65662343715307E-15,-3.20168525656498E-15));
#14006=DIRECTION('',(3.59333059809555E-15,0.529127184365608,0.848542528554299));
#14007=DIRECTION('',(1.,-2.94098829693983E-15,-4.81891406879777E-15));
#14008=DIRECTION('',(2.86959987688105E-15,-0.470295793736703,0.882508847770697));
#14009=DIRECTION('',(1.,-2.18260949170748E-15,-6.73982107121754E-15));
#14010=DIRECTION('',(-1.9524231642703E-15,-0.99942297810231,0.0339663192163947));
#14011=DIRECTION('',(7.04991620636975E-15,-6.93889390390727E-18,1.));
#14012=DIRECTION('',(0.895258480570842,-0.445547138882057,-6.31458887539222E-15));
#14013=DIRECTION('',(8.40066901809105E-15,-3.89259441896923E-16,1.));
#14014=DIRECTION('',(0.0617740994300837,-0.998090156568835,-9.07459780511577E-16));
#14015=DIRECTION('',(8.74494611700096E-15,-1.75020596507734E-15,1.));
#14016=DIRECTION('',(-0.833484381140759,-0.552543017686774,6.3217119169206E-15));
#14017=DIRECTION('',(7.73847040418957E-15,-2.72883194026474E-15,1.));
#14018=DIRECTION('',(-0.895258480570839,0.445547138882063,8.1437545194721E-15));
#14019=DIRECTION('',(6.38771759246826E-15,-2.34651139227172E-15,1.));
#14020=DIRECTION('',(-0.0617740994300767,0.998090156568836,2.73662542459142E-15));
#14021=DIRECTION('',(6.04344049355836E-15,-9.85564869091294E-16,1.));
#14022=DIRECTION('',(0.833484381140762,0.552543017686768,-4.49254627284075E-15));
#14023=DIRECTION('',(-6.93497193459788E-15,2.60658890535654E-17,-1.));
#14024=DIRECTION('',(-0.961574815122742,-0.27454302927167,6.66133814775094E-15));
#14025=DIRECTION('',(-3.44491224520631E-15,6.01889481442067E-15,-1.));
#14026=DIRECTION('',(-0.71854864534257,0.695476702899786,6.66133814775094E-15));
#14027=DIRECTION('',(3.49005968939158E-15,5.99282892536708E-15,-1.));
#14028=DIRECTION('',(0.243026169780174,0.970019732171453,6.66133814775094E-15));
#14029=DIRECTION('',(6.93497193459788E-15,-2.60658890536135E-17,-1.));
#14030=DIRECTION('',(0.961574815122743,0.274543029271663,6.66133814775094E-15));
#14031=DIRECTION('',(3.44491224520627E-15,-6.0188948144207E-15,-1.));
#14032=DIRECTION('',(0.718548645342565,-0.695476702899791,6.66133814775094E-15));
#14033=DIRECTION('',(-3.49005968939163E-15,-5.99282892536706E-15,-1.));
#14034=DIRECTION('',(-0.243026169780181,-0.970019732171452,6.66133814775094E-15));
#14035=DIRECTION('',(0.,0.,-1.));
#14036=DIRECTION('',(-1.,0.,0.));
#14037=DIRECTION('',(-6.86049799777153E-15,-7.40649559432389E-32,-1.));
#14038=DIRECTION('',(-0.98911741509944,-0.147128308448788,6.78583804585066E-15));
#14039=DIRECTION('',(-1.,1.00006808390063E-15,5.14865927669917E-15));
#14040=DIRECTION('',(5.22373843518038E-15,0.101842492372826,0.994800536161542));
#14041=DIRECTION('',(7.02216063075412E-15,-5.55111512312579E-17,1.));
#14042=DIRECTION('',(0.953807088678663,0.300419768967244,-6.68110994022551E-15));
#14043=CARTESIAN_POINT('',(0.,0.,0.));
#14044=CARTESIAN_POINT('',(0.,0.,0.));
#14045=CARTESIAN_POINT('Origin',(-62.,46.68,3.68653347947321));
#14046=CARTESIAN_POINT('',(52.,46.68,6.18653347947322));
#14047=CARTESIAN_POINT('Origin',(52.,46.68,3.68653347947321));
#14048=CARTESIAN_POINT('',(62.,46.68,6.18653347947322));
#14049=CARTESIAN_POINT('',(-62.,46.68,6.18653347947322));
#14050=CARTESIAN_POINT('Origin',(62.,46.68,3.68653347947321));
#14051=CARTESIAN_POINT('Origin',(-62.,25.68,3.68653347947321));
#14052=CARTESIAN_POINT('',(52.,25.68,6.18653347947322));
#14053=CARTESIAN_POINT('Origin',(52.,25.68,3.68653347947321));
#14054=CARTESIAN_POINT('',(62.,25.68,6.18653347947322));
#14055=CARTESIAN_POINT('',(-62.,25.68,6.18653347947322));
#14056=CARTESIAN_POINT('Origin',(62.,25.68,3.68653347947321));
#14057=CARTESIAN_POINT('Origin',(-62.,46.68,3.68653347947321));
#14058=CARTESIAN_POINT('',(-62.,46.68,6.18653347947322));
#14059=CARTESIAN_POINT('Origin',(-62.,46.68,3.68653347947321));
#14060=CARTESIAN_POINT('',(-52.,46.68,6.18653347947322));
#14061=CARTESIAN_POINT('',(-62.,46.68,6.18653347947322));
#14062=CARTESIAN_POINT('Origin',(-52.,46.68,3.68653347947321));
#14063=CARTESIAN_POINT('Origin',(-62.,25.68,3.68653347947321));
#14064=CARTESIAN_POINT('',(-62.,25.68,6.18653347947322));
#14065=CARTESIAN_POINT('Origin',(-62.,25.68,3.68653347947321));
#14066=CARTESIAN_POINT('',(-52.,25.68,6.18653347947322));
#14067=CARTESIAN_POINT('',(-62.,25.68,6.18653347947322));
#14068=CARTESIAN_POINT('Origin',(-52.,25.68,3.68653347947321));
#14069=CARTESIAN_POINT('Origin',(-26.310635094611,-8.00000000000001,14.5));
#14070=CARTESIAN_POINT('',(-29.310635094611,-8.00000000000001,14.5));
#14071=CARTESIAN_POINT('Origin',(-26.310635094611,-8.00000000000001,14.5));
#14072=CARTESIAN_POINT('',(-29.310635094611,-8.00000000000001,24.5));
#14073=CARTESIAN_POINT('',(-29.310635094611,-8.00000000000001,14.5));
#14074=CARTESIAN_POINT('Origin',(-26.310635094611,-8.00000000000001,24.5));
#14075=CARTESIAN_POINT('Origin',(-26.310635094611,-33.,14.5));
#14076=CARTESIAN_POINT('',(-29.310635094611,-33.,14.5));
#14077=CARTESIAN_POINT('Origin',(-26.310635094611,-33.,14.5));
#14078=CARTESIAN_POINT('',(-29.310635094611,-33.,24.5));
#14079=CARTESIAN_POINT('',(-29.310635094611,-33.,14.5));
#14080=CARTESIAN_POINT('Origin',(-26.310635094611,-33.,24.5));
#14081=CARTESIAN_POINT('Origin',(-4.66,-45.5,14.5));
#14082=CARTESIAN_POINT('',(-7.66000000000001,-45.5,14.5));
#14083=CARTESIAN_POINT('Origin',(-4.66,-45.5,14.5));
#14084=CARTESIAN_POINT('',(-7.66000000000001,-45.5,24.5));
#14085=CARTESIAN_POINT('',(-7.66000000000001,-45.5,14.5));
#14086=CARTESIAN_POINT('Origin',(-4.66,-45.5,24.5));
#14087=CARTESIAN_POINT('Origin',(16.990635094611,-33.,14.5));
#14088=CARTESIAN_POINT('',(13.990635094611,-33.,14.5));
#14089=CARTESIAN_POINT('Origin',(16.990635094611,-33.,14.5));
#14090=CARTESIAN_POINT('',(13.990635094611,-33.,24.5));
#14091=CARTESIAN_POINT('',(13.990635094611,-33.,14.5));
#14092=CARTESIAN_POINT('Origin',(16.990635094611,-33.,24.5));
#14093=CARTESIAN_POINT('Origin',(16.990635094611,-8.00000000000001,14.5));
#14094=CARTESIAN_POINT('',(13.990635094611,-8.00000000000001,14.5));
#14095=CARTESIAN_POINT('Origin',(16.990635094611,-8.00000000000001,14.5));
#14096=CARTESIAN_POINT('',(13.990635094611,-8.00000000000001,24.5));
#14097=CARTESIAN_POINT('',(13.990635094611,-8.00000000000001,14.5));
#14098=CARTESIAN_POINT('Origin',(16.990635094611,-8.00000000000001,24.5));
#14099=CARTESIAN_POINT('Origin',(-4.66,4.49999999999999,14.5));
#14100=CARTESIAN_POINT('',(-7.66,4.49999999999999,14.5));
#14101=CARTESIAN_POINT('Origin',(-4.66,4.49999999999999,14.5));
#14102=CARTESIAN_POINT('',(-7.66,4.49999999999999,24.5));
#14103=CARTESIAN_POINT('',(-7.66,4.49999999999999,14.5));
#14104=CARTESIAN_POINT('Origin',(-4.66,4.49999999999999,24.5));
#14105=CARTESIAN_POINT('Origin',(-4.66,-20.5,14.5));
#14106=CARTESIAN_POINT('',(-22.16,-20.5,14.5));
#14107=CARTESIAN_POINT('Origin',(-4.66,-20.5,14.5));
#14108=CARTESIAN_POINT('',(-22.16,-20.5,24.5));
#14109=CARTESIAN_POINT('',(-22.16,-20.5,14.5));
#14110=CARTESIAN_POINT('Origin',(-4.66,-20.5,24.5));
#14111=CARTESIAN_POINT('Origin',(0.,0.,-14.5));
#14112=CARTESIAN_POINT('',(-62.,59.68,-14.5));
#14113=CARTESIAN_POINT('',(-52.,59.68,-14.5));
#14114=CARTESIAN_POINT('',(-62.,59.68,-14.5));
#14115=CARTESIAN_POINT('',(-62.,76.5,-14.5));
#14116=CARTESIAN_POINT('',(-62.,-76.5,-14.5));
#14117=CARTESIAN_POINT('',(62.,76.5,-14.5));
#14118=CARTESIAN_POINT('',(-62.,76.5,-14.5));
#14119=CARTESIAN_POINT('',(62.,59.68,-14.5));
#14120=CARTESIAN_POINT('',(62.,-76.5,-14.5));
#14121=CARTESIAN_POINT('',(52.,59.68,-14.5));
#14122=CARTESIAN_POINT('',(-62.,59.68,-14.5));
#14123=CARTESIAN_POINT('',(52.,66.5,-14.5));
#14124=CARTESIAN_POINT('',(52.,-66.5,-14.5));
#14125=CARTESIAN_POINT('',(-52.,66.5,-14.5));
#14126=CARTESIAN_POINT('',(-52.,66.5,-14.5));
#14127=CARTESIAN_POINT('',(-52.,-66.5,-14.5));
#14128=CARTESIAN_POINT('Origin',(0.,0.,-14.5));
#14129=CARTESIAN_POINT('',(62.,54.68,-14.5));
#14130=CARTESIAN_POINT('',(52.,54.68,-14.5));
#14131=CARTESIAN_POINT('',(-62.,54.68,-14.5));
#14132=CARTESIAN_POINT('',(62.,53.68,-14.5));
#14133=CARTESIAN_POINT('',(62.,-76.5,-14.5));
#14134=CARTESIAN_POINT('',(52.,53.68,-14.5));
#14135=CARTESIAN_POINT('',(-62.,53.68,-14.5));
#14136=CARTESIAN_POINT('',(52.,-66.5,-14.5));
#14137=CARTESIAN_POINT('Origin',(0.,0.,-14.5));
#14138=CARTESIAN_POINT('',(52.,17.68,-14.5));
#14139=CARTESIAN_POINT('',(62.,17.68,-14.5));
#14140=CARTESIAN_POINT('',(-62.,17.68,-14.5));
#14141=CARTESIAN_POINT('',(52.,18.68,-14.5));
#14142=CARTESIAN_POINT('',(52.,-66.5,-14.5));
#14143=CARTESIAN_POINT('',(62.,18.68,-14.5));
#14144=CARTESIAN_POINT('',(-62.,18.68,-14.5));
#14145=CARTESIAN_POINT('',(62.,-76.5,-14.5));
#14146=CARTESIAN_POINT('Origin',(0.,0.,-14.5));
#14147=CARTESIAN_POINT('',(-62.,17.68,-14.5));
#14148=CARTESIAN_POINT('',(-52.,17.68,-14.5));
#14149=CARTESIAN_POINT('',(-62.,17.68,-14.5));
#14150=CARTESIAN_POINT('',(-62.,18.68,-14.5));
#14151=CARTESIAN_POINT('',(-62.,-76.5,-14.5));
#14152=CARTESIAN_POINT('',(-52.,18.68,-14.5));
#14153=CARTESIAN_POINT('',(-62.,18.68,-14.5));
#14154=CARTESIAN_POINT('',(-52.,-66.5,-14.5));
#14155=CARTESIAN_POINT('Origin',(0.,0.,-14.5));
#14156=CARTESIAN_POINT('',(-52.,54.68,-14.5));
#14157=CARTESIAN_POINT('',(-62.,54.68,-14.5));
#14158=CARTESIAN_POINT('',(-62.,54.68,-14.5));
#14159=CARTESIAN_POINT('',(-52.,53.68,-14.5));
#14160=CARTESIAN_POINT('',(-52.,-66.5,-14.5));
#14161=CARTESIAN_POINT('',(-62.,53.68,-14.5));
#14162=CARTESIAN_POINT('',(-62.,53.68,-14.5));
#14163=CARTESIAN_POINT('',(-62.,-76.5,-14.5));
#14164=CARTESIAN_POINT('Origin',(62.,-76.5,14.5));
#14165=CARTESIAN_POINT('',(62.,76.5,21.5));
#14166=CARTESIAN_POINT('',(62.,76.5,14.5));
#14167=CARTESIAN_POINT('',(62.,-76.5,21.5));
#14168=CARTESIAN_POINT('',(62.,-76.5,21.5));
#14169=CARTESIAN_POINT('',(62.,-76.5,-14.5));
#14170=CARTESIAN_POINT('',(62.,-76.5,14.5));
#14171=CARTESIAN_POINT('',(62.,12.68,-14.5));
#14172=CARTESIAN_POINT('',(62.,-76.5,-14.5));
#14173=CARTESIAN_POINT('Origin',(62.,15.18,-14.5));
#14174=CARTESIAN_POINT('Origin',(62.,36.18,-14.5));
#14175=CARTESIAN_POINT('Origin',(62.,57.18,-14.5));
#14176=CARTESIAN_POINT('Origin',(0.,0.,-14.5));
#14177=CARTESIAN_POINT('',(52.,12.68,-14.5));
#14178=CARTESIAN_POINT('',(-62.,12.68,-14.5));
#14179=CARTESIAN_POINT('',(-62.,-76.5,-14.5));
#14180=CARTESIAN_POINT('',(-62.,-76.5,-14.5));
#14181=CARTESIAN_POINT('',(-62.,12.68,-14.5));
#14182=CARTESIAN_POINT('',(-62.,-76.5,-14.5));
#14183=CARTESIAN_POINT('',(-52.,12.68,-14.5));
#14184=CARTESIAN_POINT('',(-62.,12.68,-14.5));
#14185=CARTESIAN_POINT('',(-52.,-66.5,-14.5));
#14186=CARTESIAN_POINT('',(-52.,-66.5,-14.5));
#14187=CARTESIAN_POINT('',(52.,-66.5,-14.5));
#14188=CARTESIAN_POINT('',(-52.,-66.5,-14.5));
#14189=CARTESIAN_POINT('',(52.,-66.5,-14.5));
#14190=CARTESIAN_POINT('Origin',(-62.,-76.5,14.5));
#14191=CARTESIAN_POINT('',(-62.,-76.5,21.5));
#14192=CARTESIAN_POINT('',(-62.,-76.5,14.5));
#14193=CARTESIAN_POINT('',(-62.,76.5,21.5));
#14194=CARTESIAN_POINT('',(-62.,76.5,21.5));
#14195=CARTESIAN_POINT('',(-62.,76.5,14.5));
#14196=CARTESIAN_POINT('Origin',(-62.,57.18,-14.5));
#14197=CARTESIAN_POINT('Origin',(-62.,36.18,-14.5));
#14198=CARTESIAN_POINT('Origin',(-62.,15.18,-14.5));
#14199=CARTESIAN_POINT('Origin',(-62.,-76.5,14.5));
#14200=CARTESIAN_POINT('',(-62.,-76.5,21.5));
#14201=CARTESIAN_POINT('Origin',(-62.,76.5,14.5));
#14202=CARTESIAN_POINT('',(62.,76.5,21.5));
#14203=CARTESIAN_POINT('Origin',(52.,-66.5,14.5));
#14204=CARTESIAN_POINT('Origin',(52.,57.18,-14.5));
#14205=CARTESIAN_POINT('Origin',(52.,36.18,-14.5));
#14206=CARTESIAN_POINT('Origin',(52.,15.18,-14.5));
#14207=CARTESIAN_POINT('',(52.,-66.5,14.5));
#14208=CARTESIAN_POINT('',(52.,-66.5,14.5));
#14209=CARTESIAN_POINT('',(52.,66.5,14.5));
#14210=CARTESIAN_POINT('',(52.,-66.5,14.5));
#14211=CARTESIAN_POINT('',(52.,66.5,14.5));
#14212=CARTESIAN_POINT('Origin',(-52.,66.5,14.5));
#14213=CARTESIAN_POINT('',(-52.,66.5,14.5));
#14214=CARTESIAN_POINT('',(-52.,66.5,14.5));
#14215=CARTESIAN_POINT('',(-52.,66.5,14.5));
#14216=CARTESIAN_POINT('Origin',(-52.,-66.5,14.5));
#14217=CARTESIAN_POINT('Origin',(-52.,57.18,-14.5));
#14218=CARTESIAN_POINT('',(-52.,-66.5,14.5));
#14219=CARTESIAN_POINT('',(-52.,-66.5,14.5));
#14220=CARTESIAN_POINT('',(-52.,-66.5,14.5));
#14221=CARTESIAN_POINT('Origin',(-52.,15.18,-14.5));
#14222=CARTESIAN_POINT('Origin',(-52.,36.18,-14.5));
#14223=CARTESIAN_POINT('Origin',(-52.,-66.5,14.5));
#14224=CARTESIAN_POINT('',(-52.,-66.5,14.5));
#14225=CARTESIAN_POINT('Origin',(0.,0.,14.5));
#14226=CARTESIAN_POINT('Origin',(0.,0.,24.5));
#14227=CARTESIAN_POINT('',(59.,73.5,24.5));
#14228=CARTESIAN_POINT('',(-59.,73.5,24.5));
#14229=CARTESIAN_POINT('',(-62.,73.5,24.5));
#14230=CARTESIAN_POINT('',(-59.,-73.5,24.5));
#14231=CARTESIAN_POINT('',(-59.,-76.5,24.5));
#14232=CARTESIAN_POINT('',(59.,-73.5,24.5));
#14233=CARTESIAN_POINT('',(62.,-73.5,24.5));
#14234=CARTESIAN_POINT('',(59.,76.5,24.5));
#14235=CARTESIAN_POINT('Origin',(-62.,36.18,-14.5));
#14236=CARTESIAN_POINT('Origin',(-62.,15.18,-14.5));
#14237=CARTESIAN_POINT('Origin',(-62.,57.18,-14.5));
#14238=CARTESIAN_POINT('Origin',(-62.,36.18,-14.5));
#14239=CARTESIAN_POINT('Origin',(-62.,15.18,-14.5));
#14240=CARTESIAN_POINT('Origin',(-62.,57.18,-14.5));
#14241=CARTESIAN_POINT('Origin',(59.,0.,21.5));
#14242=CARTESIAN_POINT('Origin',(59.0000000000002,-73.5000000000002,21.5000000000003));
#14243=CARTESIAN_POINT('Origin',(59.0000000000008,73.5000000000007,21.5000000000007));
#14244=CARTESIAN_POINT('Origin',(0.,73.5,21.5));
#14245=CARTESIAN_POINT('Origin',(-59.0000000000003,73.5000000000003,21.5000000000004));
#14246=CARTESIAN_POINT('Origin',(0.,-73.5,21.5));
#14247=CARTESIAN_POINT('Origin',(-59.0000000000006,-73.5000000000006,21.5000000000007));
#14248=CARTESIAN_POINT('Origin',(-59.,0.,21.5));
#14249=CARTESIAN_POINT('',(0.,0.,0.));
#14250=CARTESIAN_POINT('Origin',(78.0000000000001,-11.7,-3.46944695195361E-15));
#14251=CARTESIAN_POINT('',(-16.9,-21.2,-5.09198826713469E-15));
#14252=CARTESIAN_POINT('',(-19.1,-21.2,2.01131938556989E-13));
#14253=CARTESIAN_POINT('',(78.0000000000001,-21.2,-4.6328614111436E-15));
#14254=CARTESIAN_POINT('',(-22.1,-2.20000000000001,-2.08166817117217E-14));
#14255=CARTESIAN_POINT('Ctrl Pts',(-19.1,-21.2,4.05231403988182E-13));
#14256=CARTESIAN_POINT('Ctrl Pts',(-19.2141053600769,-21.2,-1.15460863648497));
#14257=CARTESIAN_POINT('Ctrl Pts',(-19.332091158415,-20.9895203441917,-2.30044202055597));
#14258=CARTESIAN_POINT('Ctrl Pts',(-19.5730265024687,-20.1352887413494,
-4.54344435292798));
#14259=CARTESIAN_POINT('Ctrl Pts',(-19.6962929725925,-19.4685757291998,
-5.60768898329886));
#14260=CARTESIAN_POINT('Ctrl Pts',(-19.947172704971,-17.7660153225662,-7.4155252102245));
#14261=CARTESIAN_POINT('Ctrl Pts',(-20.0685650512849,-16.7477137680798,
-8.14290619632582));
#14262=CARTESIAN_POINT('Ctrl Pts',(-20.319586856915,-14.4912108845094,-9.16464314019048));
#14263=CARTESIAN_POINT('Ctrl Pts',(-20.4403562347154,-13.274900868981,-9.44993444082396));
#14264=CARTESIAN_POINT('Ctrl Pts',(-20.6911293307758,-10.8010005184202,
-9.53803958026904));
#14265=CARTESIAN_POINT('Ctrl Pts',(-20.8125911601839,-9.5670200122243,-9.33986229220506));
#14266=CARTESIAN_POINT('Ctrl Pts',(-21.0627326460083,-7.24203907542784,
-8.48033707933769));
#14267=CARTESIAN_POINT('Ctrl Pts',(-21.1861739757011,-6.17366151377902,
-7.82617419694351));
#14268=CARTESIAN_POINT('Ctrl Pts',(-21.4353260823092,-4.34505010391497,
-6.14065935137859));
#14269=CARTESIAN_POINT('Ctrl Pts',(-21.5619357157688,-3.60400801504437,
-5.12410600030777));
#14270=CARTESIAN_POINT('Ctrl Pts',(-21.7536591008347,-2.79107732111429,
-3.36964268186332));
#14271=CARTESIAN_POINT('Ctrl Pts',(-21.8232454680744,-2.57052382279367,
-2.71585246112488));
#14272=CARTESIAN_POINT('Ctrl Pts',(-21.9626425064765,-2.27462673223657,
-1.37285912097139));
#14273=CARTESIAN_POINT('Ctrl Pts',(-22.032058430158,-2.20000000000001,-0.687486751394685));
#14274=CARTESIAN_POINT('Ctrl Pts',(-22.1,-2.20000000000001,-2.52575738102223E-14));
#14275=CARTESIAN_POINT('',(-25.9,-2.20000000000001,-2.08166817117217E-14));
#14276=CARTESIAN_POINT('',(78.0000000000001,-2.19999999999999,-1.38777878078145E-14));
#14277=CARTESIAN_POINT('',(-22.9,-21.2,1.91278709213441E-13));
#14278=CARTESIAN_POINT('Ctrl Pts',(-25.9,-2.20000000000001,-1.346145417358E-14));
#14279=CARTESIAN_POINT('Ctrl Pts',(-25.8320584301579,-2.20000000000001,
-0.687486751394945));
#14280=CARTESIAN_POINT('Ctrl Pts',(-25.7626425064764,-2.27462673223674,
-1.3728591209719));
#14281=CARTESIAN_POINT('Ctrl Pts',(-25.6232454680743,-2.57052382279374,
-2.71585246112496));
#14282=CARTESIAN_POINT('Ctrl Pts',(-25.5536591008347,-2.79107732111439,
-3.36964268186342));
#14283=CARTESIAN_POINT('Ctrl Pts',(-25.3619357157688,-3.60400801504449,
-5.12410600030786));
#14284=CARTESIAN_POINT('Ctrl Pts',(-25.2353260823091,-4.34505010391509,
-6.14065935137866));
#14285=CARTESIAN_POINT('Ctrl Pts',(-24.986173975701,-6.1736615137792,-7.82617419694359));
#14286=CARTESIAN_POINT('Ctrl Pts',(-24.8627326460082,-7.24203907542804,
-8.48033707933774));
#14287=CARTESIAN_POINT('Ctrl Pts',(-24.6125911601838,-9.5670200122245,-9.33986229220506));
#14288=CARTESIAN_POINT('Ctrl Pts',(-24.4911293307757,-10.8010005184203,
-9.53803958026902));
#14289=CARTESIAN_POINT('Ctrl Pts',(-24.2403562347153,-13.2749008689812,
-9.44993444082388));
#14290=CARTESIAN_POINT('Ctrl Pts',(-24.1195868569149,-14.4912108845096,
-9.16464314019041));
#14291=CARTESIAN_POINT('Ctrl Pts',(-23.8685650512848,-16.7477137680801,
-8.14290619632563));
#14292=CARTESIAN_POINT('Ctrl Pts',(-23.747172704971,-17.7660153225664,-7.41552521022427));
#14293=CARTESIAN_POINT('Ctrl Pts',(-23.4962929725924,-19.4685757292,-5.60768898329859));
#14294=CARTESIAN_POINT('Ctrl Pts',(-23.3730265024686,-20.1352887413495,
-4.54344435292771));
#14295=CARTESIAN_POINT('Ctrl Pts',(-23.132091158415,-20.9895203441917,-2.3004420205559));
#14296=CARTESIAN_POINT('Ctrl Pts',(-23.0141053600769,-21.2,-1.15460863648495));
#14297=CARTESIAN_POINT('Ctrl Pts',(-22.9,-21.2,3.88855614374961E-13));
#14298=CARTESIAN_POINT('',(-28.,-21.2,-4.6328614111436E-15));
#14299=CARTESIAN_POINT('',(78.0000000000001,-21.2,-4.6328614111436E-15));
#14300=CARTESIAN_POINT('Origin',(-28.,-11.7,-1.38777878078145E-14));
#14301=CARTESIAN_POINT('Ctrl Pts',(-22.9,-21.2,3.87190279838026E-13));
#14302=CARTESIAN_POINT('Ctrl Pts',(-22.8907374657687,-21.2,0.0937256760946458));
#14303=CARTESIAN_POINT('Ctrl Pts',(-22.8814385325659,-21.1986129794597,
0.187503087496975));
#14304=CARTESIAN_POINT('Ctrl Pts',(-22.7476627637501,-21.158782162885,1.53206141455917));
#14305=CARTESIAN_POINT('Ctrl Pts',(-22.6195857027287,-20.8749735642952,
2.76326935456493));
#14306=CARTESIAN_POINT('Ctrl Pts',(-22.3715836109607,-19.8492914847688,
5.03864619904501));
#14307=CARTESIAN_POINT('Ctrl Pts',(-22.2456483173604,-19.1196837186759,
6.06203761529605));
#14308=CARTESIAN_POINT('Ctrl Pts',(-21.9962859433281,-17.3106672228239,
7.76583202293418));
#14309=CARTESIAN_POINT('Ctrl Pts',(-21.8733077828502,-16.2500729662692,
8.43116573925417));
#14310=CARTESIAN_POINT('Ctrl Pts',(-21.6230205555366,-13.9355883064945,
9.3158003799263));
#14311=CARTESIAN_POINT('Ctrl Pts',(-21.5017872572193,-12.7041409356645,
9.52751127093411));
#14312=CARTESIAN_POINT('Ctrl Pts',(-21.2509382405826,-10.2294916214254,
9.46676421981238));
#14313=CARTESIAN_POINT('Ctrl Pts',(-21.1301518730001,-9.00991703997751,
9.19486269390215));
#14314=CARTESIAN_POINT('Ctrl Pts',(-20.8791269559889,-6.7415612104141,8.19766790339056));
#14315=CARTESIAN_POINT('Ctrl Pts',(-20.7574769583156,-5.7148544442386,7.48105206827987));
#14316=CARTESIAN_POINT('Ctrl Pts',(-20.5066661962114,-3.99170948168168,
5.69050173900247));
#14317=CARTESIAN_POINT('Ctrl Pts',(-20.3829213282128,-3.31314727879795,
4.63251285108534));
#14318=CARTESIAN_POINT('Ctrl Pts',(-20.1327007105934,-2.40024227986376,
2.30894656775527));
#14319=CARTESIAN_POINT('Ctrl Pts',(-20.005768200205,-2.17734057865521,1.0650747678804));
#14320=CARTESIAN_POINT('Ctrl Pts',(-19.7575217818351,-2.22627476101522,
-1.43571070081335));
#14321=CARTESIAN_POINT('Ctrl Pts',(-19.6295778173592,-2.49719213060869,
-2.66851420318476));
#14322=CARTESIAN_POINT('Ctrl Pts',(-19.3812911783324,-3.49816598006772,
-4.95240981504498));
#14323=CARTESIAN_POINT('Ctrl Pts',(-19.2559908218536,-4.21629480933593,
-5.98259204016963));
#14324=CARTESIAN_POINT('Ctrl Pts',(-19.0064304834418,-6.00563654506256,
-7.70457444607862));
#14325=CARTESIAN_POINT('Ctrl Pts',(-18.8838716533655,-7.05840175783298,
-8.38103212678982));
#14326=CARTESIAN_POINT('Ctrl Pts',(-18.6334518017468,-9.36229409907318,
-9.29067738573382));
#14327=CARTESIAN_POINT('Ctrl Pts',(-18.512401104484,-10.5911524555273,-9.5158718365491));
#14328=CARTESIAN_POINT('Ctrl Pts',(-18.2614900330185,-13.0664139465303,
-9.4823822891556));
#14329=CARTESIAN_POINT('Ctrl Pts',(-18.1406407820112,-14.2891812567478,
-9.22382157527658));
#14330=CARTESIAN_POINT('Ctrl Pts',(-17.889626499178,-16.5692015069562,-8.25108999017966));
#14331=CARTESIAN_POINT('Ctrl Pts',(-17.7676770718268,-17.6042062462676,
-7.54520943878782));
#14332=CARTESIAN_POINT('Ctrl Pts',(-17.5169480501853,-19.3476995003355,
-5.77191772591639));
#14333=CARTESIAN_POINT('Ctrl Pts',(-17.392688674322,-20.0379796864886,-4.72019166334915));
#14334=CARTESIAN_POINT('Ctrl Pts',(-17.1456751427851,-20.9644157250574,
-2.43216559502745));
#14335=CARTESIAN_POINT('Ctrl Pts',(-17.0207145116956,-21.2,-1.22148528043644));
#14336=CARTESIAN_POINT('Ctrl Pts',(-16.9,-21.2,-5.55111512312578E-15));
#14337=CARTESIAN_POINT('Origin',(78.0000000000001,-11.7,-3.46944695195361E-15));
#14338=CARTESIAN_POINT('',(-10.9,-21.2,-1.23573508489533E-14));
#14339=CARTESIAN_POINT('',(-13.1,-21.2,7.39802075989836E-15));
#14340=CARTESIAN_POINT('',(78.0000000000001,-21.2,-4.6328614111436E-15));
#14341=CARTESIAN_POINT('Ctrl Pts',(-13.1,-21.2,2.02615701994091E-14));
#14342=CARTESIAN_POINT('Ctrl Pts',(-13.2207145116956,-21.2,-1.22148528043635));
#14343=CARTESIAN_POINT('Ctrl Pts',(-13.3456751427851,-20.9644157250575,
-2.43216559502735));
#14344=CARTESIAN_POINT('Ctrl Pts',(-13.592688674322,-20.0379796864885,-4.72019166334929));
#14345=CARTESIAN_POINT('Ctrl Pts',(-13.7169480501853,-19.3476995003353,
-5.77191772591653));
#14346=CARTESIAN_POINT('Ctrl Pts',(-13.9676770718269,-17.6042062462674,
-7.5452094387879));
#14347=CARTESIAN_POINT('Ctrl Pts',(-14.089626499178,-16.569201506956,-8.25108999017973));
#14348=CARTESIAN_POINT('Ctrl Pts',(-14.3406407820113,-14.2891812567476,
-9.22382157527662));
#14349=CARTESIAN_POINT('Ctrl Pts',(-14.4614900330186,-13.0664139465301,
-9.4823822891556));
#14350=CARTESIAN_POINT('Ctrl Pts',(-14.7124011044841,-10.591152455527,-9.51587183654904));
#14351=CARTESIAN_POINT('Ctrl Pts',(-14.8334518017469,-9.36229409907295,
-9.29067738573371));
#14352=CARTESIAN_POINT('Ctrl Pts',(-15.0838716533656,-7.05840175783286,
-8.38103212678968));
#14353=CARTESIAN_POINT('Ctrl Pts',(-15.2064304834419,-6.0056365450624,-7.70457444607847));
#14354=CARTESIAN_POINT('Ctrl Pts',(-15.4559908218536,-4.21629480933576,
-5.98259204016936));
#14355=CARTESIAN_POINT('Ctrl Pts',(-15.5812911783325,-3.49816598006762,
-4.95240981504472));
#14356=CARTESIAN_POINT('Ctrl Pts',(-15.8295778173592,-2.49719213060864,
-2.66851420318443));
#14357=CARTESIAN_POINT('Ctrl Pts',(-15.9575217818352,-2.22627476101525,
-1.43571070081306));
#14358=CARTESIAN_POINT('Ctrl Pts',(-16.2057682002051,-2.1773405786553,1.0650747678805));
#14359=CARTESIAN_POINT('Ctrl Pts',(-16.3327007105934,-2.40024227986371,
2.30894656775527));
#14360=CARTESIAN_POINT('Ctrl Pts',(-16.5829213282129,-3.31314727879807,
4.63251285108554));
#14361=CARTESIAN_POINT('Ctrl Pts',(-16.7066661962114,-3.99170948168173,
5.69050173900263));
#14362=CARTESIAN_POINT('Ctrl Pts',(-16.9574769583157,-5.71485444423879,
7.48105206828005));
#14363=CARTESIAN_POINT('Ctrl Pts',(-17.079126955989,-6.74156121041422,8.19766790339073));
#14364=CARTESIAN_POINT('Ctrl Pts',(-17.3301518730003,-9.00991703997782,
9.19486269390231));
#14365=CARTESIAN_POINT('Ctrl Pts',(-17.4509382405827,-10.2294916214257,
9.46676421981248));
#14366=CARTESIAN_POINT('Ctrl Pts',(-17.7017872572195,-12.7041409356649,
9.52751127093413));
#14367=CARTESIAN_POINT('Ctrl Pts',(-17.8230205555367,-13.9355883064948,
9.31580037992625));
#14368=CARTESIAN_POINT('Ctrl Pts',(-18.0733077828503,-16.2500729662695,
8.43116573925405));
#14369=CARTESIAN_POINT('Ctrl Pts',(-18.1962859433283,-17.3106672228242,
7.76583202293403));
#14370=CARTESIAN_POINT('Ctrl Pts',(-18.4456483173605,-19.1196837186761,
6.06203761529587));
#14371=CARTESIAN_POINT('Ctrl Pts',(-18.5715836109608,-19.849291484769,5.0386461990448));
#14372=CARTESIAN_POINT('Ctrl Pts',(-18.8195857027288,-20.8749735642953,
2.76326935456469));
#14373=CARTESIAN_POINT('Ctrl Pts',(-18.9476627637502,-21.1587821628851,
1.53206141455895));
#14374=CARTESIAN_POINT('Ctrl Pts',(-19.081438532566,-21.1986129794598,0.187503087496803));
#14375=CARTESIAN_POINT('Ctrl Pts',(-19.0907374657687,-21.2,0.0937256760945715));
#14376=CARTESIAN_POINT('Ctrl Pts',(-19.1,-21.2,4.06896738525122E-13));
#14377=CARTESIAN_POINT('Ctrl Pts',(-16.9,-21.2,-6.93889390390721E-15));
#14378=CARTESIAN_POINT('Ctrl Pts',(-16.8969830453883,-21.2,0.0305279423179293));
#14379=CARTESIAN_POINT('Ctrl Pts',(-16.8939621685952,-21.1998528492313,
0.061061986178125));
#14380=CARTESIAN_POINT('Ctrl Pts',(-16.767248128974,-21.1875162370896,1.34043950276099));
#14381=CARTESIAN_POINT('Ctrl Pts',(-16.6394486076613,-20.929329190971,2.57468702777397));
#14382=CARTESIAN_POINT('Ctrl Pts',(-16.390901029389,-19.9527852055101,4.8667989871523));
#14383=CARTESIAN_POINT('Ctrl Pts',(-16.2661865852166,-19.2459958496645,
5.90361775701928));
#14384=CARTESIAN_POINT('Ctrl Pts',(-16.0164434579476,-17.4760938667978,
7.6434092654843));
#14385=CARTESIAN_POINT('Ctrl Pts',(-15.8942543732133,-16.4310772867914,
8.33076824399953));
#14386=CARTESIAN_POINT('Ctrl Pts',(-15.6437167913769,-14.1377024264444,
9.26493007649789));
#14387=CARTESIAN_POINT('Ctrl Pts',(-15.5228012264078,-12.9114457325454,
9.50334490259744));
#14388=CARTESIAN_POINT('Ctrl Pts',(-15.2718422511462,-10.4357116660551,
9.49658163777807));
#14389=CARTESIAN_POINT('Ctrl Pts',(-15.1508875962576,-9.20987735813003,
9.25110322734293));
#14390=CARTESIAN_POINT('Ctrl Pts',(-14.8998967426513,-6.91855760852222,
8.30236799838261));
#14391=CARTESIAN_POINT('Ctrl Pts',(-14.7776129198827,-5.87549075136833,
7.60702303698604));
#14392=CARTESIAN_POINT('Ctrl Pts',(-14.5269765839982,-4.1122003669309,5.85068851113439));
#14393=CARTESIAN_POINT('Ctrl Pts',(-14.402176887142,-3.41051525358195,4.80513228098767));
#14394=CARTESIAN_POINT('Ctrl Pts',(-14.152310008838,-2.44844277306473,2.49636756975496));
#14395=CARTESIAN_POINT('Ctrl Pts',(-14.0239657950969,-2.19999999999999,
1.25438434751193));
#14396=CARTESIAN_POINT('Ctrl Pts',(-13.7760812749615,-2.20000000000001,
-1.25390805528599));
#14397=CARTESIAN_POINT('Ctrl Pts',(-13.6477361899215,-2.44826489212498,
-2.49594069418698));
#14398=CARTESIAN_POINT('Ctrl Pts',(-13.397823112858,-3.41051525358197,-4.80513228098764));
#14399=CARTESIAN_POINT('Ctrl Pts',(-13.2730234160018,-4.11220036693088,
-5.85068851113436));
#14400=CARTESIAN_POINT('Ctrl Pts',(-13.0223870801173,-5.87549075136848,
-7.60702303698617));
#14401=CARTESIAN_POINT('Ctrl Pts',(-12.9001032573487,-6.9185576085226,-8.30236799838268));
#14402=CARTESIAN_POINT('Ctrl Pts',(-12.6491124037424,-9.20987735813013,
-9.25110322734288));
#14403=CARTESIAN_POINT('Ctrl Pts',(-12.5281577488538,-10.4357116660553,
-9.49658163777797));
#14404=CARTESIAN_POINT('Ctrl Pts',(-12.2771987735922,-12.9114457325455,
-9.50334490259733));
#14405=CARTESIAN_POINT('Ctrl Pts',(-12.156283208623,-14.1377024264445,-9.26493007649772));
#14406=CARTESIAN_POINT('Ctrl Pts',(-11.9057456267867,-16.4310772867914,
-8.33076824399935));
#14407=CARTESIAN_POINT('Ctrl Pts',(-11.7835565420524,-17.4760938667978,
-7.64340926548411));
#14408=CARTESIAN_POINT('Ctrl Pts',(-11.5338134147834,-19.2459958496646,
-5.90361775701905));
#14409=CARTESIAN_POINT('Ctrl Pts',(-11.409098970611,-19.9527852055101,-4.86679898715208));
#14410=CARTESIAN_POINT('Ctrl Pts',(-11.1605513923387,-20.9293291909709,
-2.57468702777379));
#14411=CARTESIAN_POINT('Ctrl Pts',(-11.032751871026,-21.1875162370895,-1.34043950276079));
#14412=CARTESIAN_POINT('Ctrl Pts',(-10.9060378314048,-21.1998528492312,
-0.0610619861779927));
#14413=CARTESIAN_POINT('Ctrl Pts',(-10.9030169546117,-21.2,-0.03052794231788));
#14414=CARTESIAN_POINT('Ctrl Pts',(-10.9,-21.2,-2.0081840286763E-14));
#14415=CARTESIAN_POINT('Origin',(78.0000000000001,-11.7,-3.46944695195361E-15));
#14416=CARTESIAN_POINT('',(-4.90000000000003,-21.2,-1.98093323684911E-13));
#14417=CARTESIAN_POINT('',(-7.1,-21.2,-4.25932099866582E-15));
#14418=CARTESIAN_POINT('',(78.0000000000001,-21.2,-4.6328614111436E-15));
#14419=CARTESIAN_POINT('Ctrl Pts',(-7.1,-21.2,-1.04083408558609E-14));
#14420=CARTESIAN_POINT('Ctrl Pts',(-7.10301695461173,-21.2,-0.0305279423178875));
#14421=CARTESIAN_POINT('Ctrl Pts',(-7.10603783140479,-21.1998528492312,
-0.0610619861780148));
#14422=CARTESIAN_POINT('Ctrl Pts',(-7.23275187102597,-21.1875162370895,
-1.34043950276082));
#14423=CARTESIAN_POINT('Ctrl Pts',(-7.36055139233868,-20.9293291909709,
-2.57468702777381));
#14424=CARTESIAN_POINT('Ctrl Pts',(-7.60909897061095,-19.9527852055101,
-4.86679898715213));
#14425=CARTESIAN_POINT('Ctrl Pts',(-7.73381341478335,-19.2459958496646,
-5.90361775701912));
#14426=CARTESIAN_POINT('Ctrl Pts',(-7.98355654205236,-17.4760938667978,
-7.64340926548419));
#14427=CARTESIAN_POINT('Ctrl Pts',(-8.10574562678669,-16.4310772867913,
-8.33076824399942));
#14428=CARTESIAN_POINT('Ctrl Pts',(-8.35628320862303,-14.1377024264445,
-9.26493007649778));
#14429=CARTESIAN_POINT('Ctrl Pts',(-8.47719877359217,-12.9114457325455,
-9.50334490259736));
#14430=CARTESIAN_POINT('Ctrl Pts',(-8.72815774885374,-10.4357116660555,
-9.49658163777799));
#14431=CARTESIAN_POINT('Ctrl Pts',(-8.84911240374241,-9.2098773581302,-9.25110322734298));
#14432=CARTESIAN_POINT('Ctrl Pts',(-9.10010325734868,-6.91855760852233,
-8.30236799838263));
#14433=CARTESIAN_POINT('Ctrl Pts',(-9.22238708011727,-5.87549075136838,
-7.60702303698608));
#14434=CARTESIAN_POINT('Ctrl Pts',(-9.47302341600179,-4.1122003669308,-5.85068851113429));
#14435=CARTESIAN_POINT('Ctrl Pts',(-9.59782311285803,-3.41051525358196,
-4.80513228098758));
#14436=CARTESIAN_POINT('Ctrl Pts',(-9.84773618992147,-2.44826489212505,
-2.4959406941871));
#14437=CARTESIAN_POINT('Ctrl Pts',(-9.97608127496146,-2.2,-1.25390805528605));
#14438=CARTESIAN_POINT('Ctrl Pts',(-10.2239657950969,-2.19999999999999,
1.25438434751194));
#14439=CARTESIAN_POINT('Ctrl Pts',(-10.352310008838,-2.44844277306475,2.49636756975497));
#14440=CARTESIAN_POINT('Ctrl Pts',(-10.602176887142,-3.41051525358195,4.80513228098765));
#14441=CARTESIAN_POINT('Ctrl Pts',(-10.7269765839982,-4.11220036693091,
5.85068851113438));
#14442=CARTESIAN_POINT('Ctrl Pts',(-10.9776129198827,-5.87549075136841,
7.60702303698611));
#14443=CARTESIAN_POINT('Ctrl Pts',(-11.0998967426514,-6.91855760852248,
8.30236799838264));
#14444=CARTESIAN_POINT('Ctrl Pts',(-11.3508875962576,-9.20987735813005,
9.25110322734288));
#14445=CARTESIAN_POINT('Ctrl Pts',(-11.4718422511462,-10.4357116660552,
9.496581637778));
#14446=CARTESIAN_POINT('Ctrl Pts',(-11.7228012264078,-12.9114457325453,
9.50334490259737));
#14447=CARTESIAN_POINT('Ctrl Pts',(-11.843716791377,-14.1377024264444,9.26493007649785));
#14448=CARTESIAN_POINT('Ctrl Pts',(-12.0942543732133,-16.4310772867913,
8.33076824399947));
#14449=CARTESIAN_POINT('Ctrl Pts',(-12.2164434579477,-17.4760938667978,
7.64340926548424));
#14450=CARTESIAN_POINT('Ctrl Pts',(-12.4661865852167,-19.2459958496646,
5.90361775701917));
#14451=CARTESIAN_POINT('Ctrl Pts',(-12.5909010293891,-19.9527852055101,
4.8667989871522));
#14452=CARTESIAN_POINT('Ctrl Pts',(-12.8394486076613,-20.929329190971,2.57468702777389));
#14453=CARTESIAN_POINT('Ctrl Pts',(-12.9672481289741,-21.1875162370896,
1.3404395027609));
#14454=CARTESIAN_POINT('Ctrl Pts',(-13.0939621685952,-21.1998528492313,
0.0610619861780588));
#14455=CARTESIAN_POINT('Ctrl Pts',(-13.0969830453883,-21.2,0.0305279423179154));
#14456=CARTESIAN_POINT('Ctrl Pts',(-13.1,-21.2,1.94289029309403E-14));
#14457=CARTESIAN_POINT('Ctrl Pts',(-10.9,-21.2,-2.05391259555654E-14));
#14458=CARTESIAN_POINT('Ctrl Pts',(-10.7792854883044,-21.2,1.22148528043648));
#14459=CARTESIAN_POINT('Ctrl Pts',(-10.6543248572149,-20.9644157250573,
2.43216559502755));
#14460=CARTESIAN_POINT('Ctrl Pts',(-10.407311325678,-20.0379796864884,4.72019166334933));
#14461=CARTESIAN_POINT('Ctrl Pts',(-10.2830519498147,-19.3476995003352,
5.77191772591653));
#14462=CARTESIAN_POINT('Ctrl Pts',(-10.0323229281731,-17.6042062462672,
7.54520943878794));
#14463=CARTESIAN_POINT('Ctrl Pts',(-9.91037350082199,-16.5692015069558,
8.25108999017974));
#14464=CARTESIAN_POINT('Ctrl Pts',(-9.65935921798872,-14.2891812567473,
9.22382157527658));
#14465=CARTESIAN_POINT('Ctrl Pts',(-9.53850996698142,-13.0664139465299,
9.48238228915555));
#14466=CARTESIAN_POINT('Ctrl Pts',(-9.28759889551594,-10.5911524555268,
9.51587183654892));
#14467=CARTESIAN_POINT('Ctrl Pts',(-9.16654819825313,-9.36229409907269,
9.29067738573355));
#14468=CARTESIAN_POINT('Ctrl Pts',(-8.91612834663441,-7.05840175783258,
8.38103212678943));
#14469=CARTESIAN_POINT('Ctrl Pts',(-8.79356951655812,-6.00563654506221,
7.70457444607819));
#14470=CARTESIAN_POINT('Ctrl Pts',(-8.54400917814636,-4.21629480933569,
5.9825920401691));
#14471=CARTESIAN_POINT('Ctrl Pts',(-8.41870882166752,-3.49816598006753,
4.95240981504442));
#14472=CARTESIAN_POINT('Ctrl Pts',(-8.17042218264078,-2.49719213060864,
2.6685142031841));
#14473=CARTESIAN_POINT('Ctrl Pts',(-8.04247821816479,-2.22627476101526,
1.43571070081269));
#14474=CARTESIAN_POINT('Ctrl Pts',(-7.7942317997949,-2.17734057865542,-1.0650747678811));
#14475=CARTESIAN_POINT('Ctrl Pts',(-7.66729928940652,-2.40024227986408,
-2.30894656775598));
#14476=CARTESIAN_POINT('Ctrl Pts',(-7.41707867178707,-3.31314727879848,
-4.63251285108605));
#14477=CARTESIAN_POINT('Ctrl Pts',(-7.29333380378853,-3.99170948168244,
-5.69050173900314));
#14478=CARTESIAN_POINT('Ctrl Pts',(-7.04252304168434,-5.71485444423936,
-7.48105206828023));
#14479=CARTESIAN_POINT('Ctrl Pts',(-6.92087304401098,-6.74156121041487,
-8.19766790339084));
#14480=CARTESIAN_POINT('Ctrl Pts',(-6.66984812699976,-9.0099170399785,-9.19486269390227));
#14481=CARTESIAN_POINT('Ctrl Pts',(-6.54906175941734,-10.2294916214264,
-9.46676421981235));
#14482=CARTESIAN_POINT('Ctrl Pts',(-6.29821274278055,-12.7041409356655,
-9.52751127093382));
#14483=CARTESIAN_POINT('Ctrl Pts',(-6.17697944446328,-13.9355883064955,
-9.31580037992587));
#14484=CARTESIAN_POINT('Ctrl Pts',(-5.92669221714971,-16.25007296627,-8.4311657392535));
#14485=CARTESIAN_POINT('Ctrl Pts',(-5.80371405667172,-17.3106672228247,
-7.76583202293341));
#14486=CARTESIAN_POINT('Ctrl Pts',(-5.55435168263951,-19.1196837186765,
-6.06203761529504));
#14487=CARTESIAN_POINT('Ctrl Pts',(-5.42841638903915,-19.8492914847693,
-5.03864619904393));
#14488=CARTESIAN_POINT('Ctrl Pts',(-5.18041429727117,-20.8749735642954,
-2.76326935456374));
#14489=CARTESIAN_POINT('Ctrl Pts',(-5.05233723624973,-21.158782162885,-1.53206141455799));
#14490=CARTESIAN_POINT('Ctrl Pts',(-4.91856146743402,-21.1986129794595,
-0.187503087496173));
#14491=CARTESIAN_POINT('Ctrl Pts',(-4.90926253423129,-21.2,-0.0937256760942467));
#14492=CARTESIAN_POINT('Ctrl Pts',(-4.90000000000004,-21.2,-3.91553785958679E-13));
#14493=CARTESIAN_POINT('Origin',(78.0000000000001,-11.7,-3.46944695195361E-15));
#14494=CARTESIAN_POINT('',(1.10000000000044,-21.2,2.23339518513334E-12));
#14495=CARTESIAN_POINT('',(-1.10000000000004,-21.2,-2.02746363044123E-13));
#14496=CARTESIAN_POINT('',(78.0000000000001,-21.2,-4.6328614111436E-15));
#14497=CARTESIAN_POINT('Ctrl Pts',(-1.10000000000004,-21.2,-4.00859864677103E-13));
#14498=CARTESIAN_POINT('Ctrl Pts',(-1.10926253423131,-21.2,-0.0937256760943962));
#14499=CARTESIAN_POINT('Ctrl Pts',(-1.11856146743405,-21.1986129794596,
-0.187503087496459));
#14500=CARTESIAN_POINT('Ctrl Pts',(-1.25233723624978,-21.158782162885,-1.53206141455843));
#14501=CARTESIAN_POINT('Ctrl Pts',(-1.38041429727121,-20.8749735642953,
-2.76326935456418));
#14502=CARTESIAN_POINT('Ctrl Pts',(-1.62841638903919,-19.8492914847691,
-5.03864619904435));
#14503=CARTESIAN_POINT('Ctrl Pts',(-1.75435168263955,-19.1196837186762,
-6.06203761529545));
#14504=CARTESIAN_POINT('Ctrl Pts',(-2.00371405667176,-17.3106672228244,
-7.76583202293368));
#14505=CARTESIAN_POINT('Ctrl Pts',(-2.12669221714973,-16.2500729662697,
-8.43116573925373));
#14506=CARTESIAN_POINT('Ctrl Pts',(-2.37697944446329,-13.9355883064952,
-9.315800379926));
#14507=CARTESIAN_POINT('Ctrl Pts',(-2.49821274278056,-12.7041409356653,
-9.52751127093395));
#14508=CARTESIAN_POINT('Ctrl Pts',(-2.74906175941735,-10.2294916214261,
-9.46676421981238));
#14509=CARTESIAN_POINT('Ctrl Pts',(-2.86984812699978,-9.00991703997814,
-9.19486269390226));
#14510=CARTESIAN_POINT('Ctrl Pts',(-3.12087304401099,-6.74156121041458,
-8.19766790339077));
#14511=CARTESIAN_POINT('Ctrl Pts',(-3.24252304168436,-5.71485444423907,
-7.48105206828013));
#14512=CARTESIAN_POINT('Ctrl Pts',(-3.49333380378854,-3.9917094816822,-5.69050173900298));
#14513=CARTESIAN_POINT('Ctrl Pts',(-3.61707867178709,-3.31314727879827,
-4.63251285108587));
#14514=CARTESIAN_POINT('Ctrl Pts',(-3.86729928940655,-2.40024227986389,
-2.30894656775566));
#14515=CARTESIAN_POINT('Ctrl Pts',(-3.99423179979492,-2.17734057865532,
-1.06507476788081));
#14516=CARTESIAN_POINT('Ctrl Pts',(-4.24247821816481,-2.22627476101522,
1.43571070081288));
#14517=CARTESIAN_POINT('Ctrl Pts',(-4.3704221826408,-2.49719213060861,2.66851420318427));
#14518=CARTESIAN_POINT('Ctrl Pts',(-4.61870882166753,-3.49816598006755,
4.95240981504459));
#14519=CARTESIAN_POINT('Ctrl Pts',(-4.74400917814637,-4.21629480933573,
5.98259204016927));
#14520=CARTESIAN_POINT('Ctrl Pts',(-4.99356951655813,-6.00563654506232,
7.70457444607837));
#14521=CARTESIAN_POINT('Ctrl Pts',(-5.11612834663442,-7.05840175783277,
8.38103212678959));
#14522=CARTESIAN_POINT('Ctrl Pts',(-5.36654819825314,-9.36229409907284,
9.29067738573365));
#14523=CARTESIAN_POINT('Ctrl Pts',(-5.48759889551595,-10.591152455527,9.51587183654897));
#14524=CARTESIAN_POINT('Ctrl Pts',(-5.73850996698142,-13.06641394653,9.48238228915556));
#14525=CARTESIAN_POINT('Ctrl Pts',(-5.85935921798873,-14.2891812567474,
9.22382157527661));
#14526=CARTESIAN_POINT('Ctrl Pts',(-6.11037350082199,-16.5692015069559,
8.25108999017975));
#14527=CARTESIAN_POINT('Ctrl Pts',(-6.23232292817312,-17.6042062462673,
7.54520943878795));
#14528=CARTESIAN_POINT('Ctrl Pts',(-6.48305194981473,-19.3476995003354,
5.77191772591646));
#14529=CARTESIAN_POINT('Ctrl Pts',(-6.60731132567798,-20.0379796864884,
4.72019166334927));
#14530=CARTESIAN_POINT('Ctrl Pts',(-6.85432485721487,-20.9644157250573,
2.43216559502755));
#14531=CARTESIAN_POINT('Ctrl Pts',(-6.97928548830439,-21.2,1.22148528043648));
#14532=CARTESIAN_POINT('Ctrl Pts',(-7.1,-21.2,-9.71445146547012E-15));
#14533=CARTESIAN_POINT('',(-1.9,-2.2,0.));
#14534=CARTESIAN_POINT('Ctrl Pts',(-4.90000000000003,-21.2,-3.92186283448837E-13));
#14535=CARTESIAN_POINT('Ctrl Pts',(-4.78589463992307,-21.2,1.15460863648533));
#14536=CARTESIAN_POINT('Ctrl Pts',(-4.66790884158497,-20.9895203441914,
2.30044202055665));
#14537=CARTESIAN_POINT('Ctrl Pts',(-4.42697349753129,-20.1352887413487,
4.54344435292883));
#14538=CARTESIAN_POINT('Ctrl Pts',(-4.30370702740743,-19.468575729199,5.6076889832996));
#14539=CARTESIAN_POINT('Ctrl Pts',(-4.0528272950289,-17.7660153225651,7.41552521022513));
#14540=CARTESIAN_POINT('Ctrl Pts',(-3.93143494871502,-16.7477137680786,
8.14290619632631));
#14541=CARTESIAN_POINT('Ctrl Pts',(-3.68041314308496,-14.491210884508,9.16464314019071));
#14542=CARTESIAN_POINT('Ctrl Pts',(-3.55964376528457,-13.2749008689796,
9.44993444082394));
#14543=CARTESIAN_POINT('Ctrl Pts',(-3.30887066922413,-10.8010005184188,
9.53803958026867));
#14544=CARTESIAN_POINT('Ctrl Pts',(-3.18740883981607,-9.56702001222297,
9.33986229220452));
#14545=CARTESIAN_POINT('Ctrl Pts',(-2.93726735399162,-7.24203907542668,
8.48033707933681));
#14546=CARTESIAN_POINT('Ctrl Pts',(-2.81382602429882,-6.17366151377793,
7.82617419694249));
#14547=CARTESIAN_POINT('Ctrl Pts',(-2.56467391769076,-4.34505010391411,
6.14065935137722));
#14548=CARTESIAN_POINT('Ctrl Pts',(-2.43806428423111,-3.60400801504371,
5.12410600030631));
#14549=CARTESIAN_POINT('Ctrl Pts',(-2.24634089916518,-2.79107732111404,
3.36964268186199));
#14550=CARTESIAN_POINT('Ctrl Pts',(-2.17675453192557,-2.57052382279359,
2.71585246112379));
#14551=CARTESIAN_POINT('Ctrl Pts',(-2.03735749352367,-2.27462673223717,
1.37285912097279));
#14552=CARTESIAN_POINT('Ctrl Pts',(-1.96794156984213,-2.20000000000001,
0.687486751395415));
#14553=CARTESIAN_POINT('Ctrl Pts',(-1.9,-2.20000000000001,0.));
#14554=CARTESIAN_POINT('Ctrl Pts',(-1.9,-2.20000000000001,-9.71445146547012E-16));
#14555=CARTESIAN_POINT('Ctrl Pts',(-1.82240919606718,-2.20000000000001,
-0.785125363718995));
#14556=CARTESIAN_POINT('Ctrl Pts',(-1.742931224028,-2.29732921818939,-1.56713183388941));
#14557=CARTESIAN_POINT('Ctrl Pts',(-1.58397810910787,-2.68171790682092,
-3.08781145458966));
#14558=CARTESIAN_POINT('Ctrl Pts',(-1.50627788561728,-2.96698552223606,
-3.82077835789411));
#14559=CARTESIAN_POINT('Ctrl Pts',(-1.30309366168197,-3.93400067098277,
-5.61337377836322));
#14560=CARTESIAN_POINT('Ctrl Pts',(-1.17482924813685,-4.74147972021909,
-6.5878620867794));
#14561=CARTESIAN_POINT('Ctrl Pts',(-0.927331863007985,-6.68268234478074,
-8.16270927538555));
#14562=CARTESIAN_POINT('Ctrl Pts',(-0.800278464085321,-7.79598298912007,
-8.75006417475044));
#14563=CARTESIAN_POINT('Ctrl Pts',(-0.551264801242581,-10.1808762870929,
-9.45953708808233));
#14564=CARTESIAN_POINT('Ctrl Pts',(-0.427510001032243,-11.4286112335544,
-9.57690646451572));
#14565=CARTESIAN_POINT('Ctrl Pts',(-0.177466838670091,-13.8953107190287,
-9.32543555556563));
#14566=CARTESIAN_POINT('Ctrl Pts',(-0.0558377561646816,-15.090781291844,
-8.96021822335387));
#14567=CARTESIAN_POINT('Ctrl Pts',(0.194880480566995,-17.273490661377,-7.79214963085964));
#14568=CARTESIAN_POINT('Ctrl Pts',(0.315662999058585,-18.2400206930619,
-7.00067537881007));
#14569=CARTESIAN_POINT('Ctrl Pts',(0.566675728348146,-19.8162347312299,
-5.09040313956777));
#14570=CARTESIAN_POINT('Ctrl Pts',(0.687928012700195,-20.4103423716323,
-3.98943736487644));
#14571=CARTESIAN_POINT('Ctrl Pts',(0.909485604799865,-21.0576446211017,
-1.89528423874928));
#14572=CARTESIAN_POINT('Ctrl Pts',(1.00615236670273,-21.2,-0.949624871658705));
#14573=CARTESIAN_POINT('Ctrl Pts',(1.10000000000044,-21.2,4.47988868224058E-12));
#14574=CARTESIAN_POINT('Origin',(78.0000000000001,-11.7,-3.46944695195361E-15));
#14575=CARTESIAN_POINT('',(7.10000000000035,-21.2,1.74965019662244E-12));
#14576=CARTESIAN_POINT('',(4.90000000000003,-21.2,1.91358318085311E-13));
#14577=CARTESIAN_POINT('',(78.0000000000001,-21.2,-4.6328614111436E-15));
#14578=CARTESIAN_POINT('',(1.9,-2.19999999999999,0.));
#14579=CARTESIAN_POINT('Ctrl Pts',(4.90000000000004,-21.2,3.87190279838023E-13));
#14580=CARTESIAN_POINT('Ctrl Pts',(4.78589463992312,-21.2,-1.15460863648501));
#14581=CARTESIAN_POINT('Ctrl Pts',(4.66790884158501,-20.9895203441916,-2.30044202055602));
#14582=CARTESIAN_POINT('Ctrl Pts',(4.42697349753135,-20.1352887413493,-4.54344435292803));
#14583=CARTESIAN_POINT('Ctrl Pts',(4.30370702740749,-19.4685757291996,-5.60768898329891));
#14584=CARTESIAN_POINT('Ctrl Pts',(4.05282729502898,-17.7660153225659,-7.41552521022458));
#14585=CARTESIAN_POINT('Ctrl Pts',(3.9314349487151,-16.7477137680793,-8.14290619632586));
#14586=CARTESIAN_POINT('Ctrl Pts',(3.68041314308507,-14.4912108845091,-9.16464314019039));
#14587=CARTESIAN_POINT('Ctrl Pts',(3.55964376528467,-13.2749008689808,-9.44993444082381));
#14588=CARTESIAN_POINT('Ctrl Pts',(3.30887066922423,-10.8010005184199,-9.53803958026883));
#14589=CARTESIAN_POINT('Ctrl Pts',(3.18740883981617,-9.56702001222408,-9.33986229220482));
#14590=CARTESIAN_POINT('Ctrl Pts',(2.93726735399172,-7.24203907542763,-8.48033707933737));
#14591=CARTESIAN_POINT('Ctrl Pts',(2.81382602429894,-6.17366151377884,-7.82617419694316));
#14592=CARTESIAN_POINT('Ctrl Pts',(2.56467391769087,-4.34505010391488,-6.14065935137818));
#14593=CARTESIAN_POINT('Ctrl Pts',(2.43806428423122,-3.60400801504429,-5.12410600030733));
#14594=CARTESIAN_POINT('Ctrl Pts',(2.24634089916526,-2.79107732111432,-3.36964268186288));
#14595=CARTESIAN_POINT('Ctrl Pts',(2.17675453192563,-2.57052382279375,-2.71585246112451));
#14596=CARTESIAN_POINT('Ctrl Pts',(2.03735749352367,-2.2746267322371,-1.37285912097289));
#14597=CARTESIAN_POINT('Ctrl Pts',(1.96794156984213,-2.20000000000001,-0.687486751395457));
#14598=CARTESIAN_POINT('Ctrl Pts',(1.9,-2.20000000000001,4.16333634234434E-16));
#14599=CARTESIAN_POINT('Ctrl Pts',(1.9,-2.20000000000001,2.77555756156289E-16));
#14600=CARTESIAN_POINT('Ctrl Pts',(1.8320584301579,-2.20000000000001,0.687486751395224));
#14601=CARTESIAN_POINT('Ctrl Pts',(1.76264250647639,-2.27462673223699,1.37285912097244));
#14602=CARTESIAN_POINT('Ctrl Pts',(1.62324546807441,-2.57052382279363,2.7158524611242));
#14603=CARTESIAN_POINT('Ctrl Pts',(1.55365910083479,-2.79107732111415,3.36964268186248));
#14604=CARTESIAN_POINT('Ctrl Pts',(1.36193571576884,-3.60400801504399,5.1241060003069));
#14605=CARTESIAN_POINT('Ctrl Pts',(1.23532608230919,-4.34505010391456,6.14065935137781));
#14606=CARTESIAN_POINT('Ctrl Pts',(0.986173975701136,-6.17366151377839,
7.82617419694286));
#14607=CARTESIAN_POINT('Ctrl Pts',(0.862732646008349,-7.24203907542715,
8.48033707933712));
#14608=CARTESIAN_POINT('Ctrl Pts',(0.612591160183894,-9.56702001222349,
9.33986229220469));
#14609=CARTESIAN_POINT('Ctrl Pts',(0.491129330775837,-10.8010005184193,
9.5380395802688));
#14610=CARTESIAN_POINT('Ctrl Pts',(0.240356234715391,-13.2749008689802,
9.44993444082392));
#14611=CARTESIAN_POINT('Ctrl Pts',(0.119586856914992,-14.4912108845086,
9.16464314019056));
#14612=CARTESIAN_POINT('Ctrl Pts',(-0.131434948715058,-16.7477137680791,
8.14290619632607));
#14613=CARTESIAN_POINT('Ctrl Pts',(-0.252827295028933,-17.7660153225655,
7.41552521022482));
#14614=CARTESIAN_POINT('Ctrl Pts',(-0.503707027407458,-19.4685757291994,
5.60768898329921));
#14615=CARTESIAN_POINT('Ctrl Pts',(-0.626973497531317,-20.135288741349,
4.54344435292839));
#14616=CARTESIAN_POINT('Ctrl Pts',(-0.867908841584979,-20.9895203441915,
2.30044202055641));
#14617=CARTESIAN_POINT('Ctrl Pts',(-0.985894639923092,-21.2,1.15460863648521));
#14618=CARTESIAN_POINT('Ctrl Pts',(-1.10000000000004,-21.2,-3.99957844621213E-13));
#14619=CARTESIAN_POINT('Ctrl Pts',(1.10000000000044,-21.2,4.47669679104479E-12));
#14620=CARTESIAN_POINT('Ctrl Pts',(1.12861197762933,-21.2,0.289518708458957));
#14621=CARTESIAN_POINT('Ctrl Pts',(1.15755311853428,-21.1867657550865,0.579347522267127));
#14622=CARTESIAN_POINT('Ctrl Pts',(1.31226798453121,-21.0459766280402,2.11274118535634));
#14623=CARTESIAN_POINT('Ctrl Pts',(1.43812594008345,-20.687408477367,3.32214218001096));
#14624=CARTESIAN_POINT('Ctrl Pts',(1.68717348681367,-19.5218084280711,5.5350716129601));
#14625=CARTESIAN_POINT('Ctrl Pts',(1.81532810695294,-18.7250004034997,6.51668441409436));
#14626=CARTESIAN_POINT('Ctrl Pts',(2.06313890932384,-16.8019149156045,8.10993421382391));
#14627=CARTESIAN_POINT('Ctrl Pts',(2.18949911840483,-15.6958499037577,8.70833285820448));
#14628=CARTESIAN_POINT('Ctrl Pts',(2.43872900929925,-13.320528711054,9.44259877042744));
#14629=CARTESIAN_POINT('Ctrl Pts',(2.5619970700894,-12.0749025039173,9.57331164819956));
#14630=CARTESIAN_POINT('Ctrl Pts',(2.81219300304181,-9.60669592209691,9.34882097078356));
#14631=CARTESIAN_POINT('Ctrl Pts',(2.93356650916228,-8.40761994419821,8.99679824400882));
#14632=CARTESIAN_POINT('Ctrl Pts',(3.18436883977102,-6.21236435328532,7.85287012939994));
#14633=CARTESIAN_POINT('Ctrl Pts',(3.3051389283296,-5.23710293161833,7.07196332583943));
#14634=CARTESIAN_POINT('Ctrl Pts',(3.55616351811101,-3.6396095638801,5.17851113080937));
#14635=CARTESIAN_POINT('Ctrl Pts',(3.67764453489987,-3.0332911184828,4.0835346992797));
#14636=CARTESIAN_POINT('Ctrl Pts',(3.92850071102958,-2.27424266566553,1.71842057764594));
#14637=CARTESIAN_POINT('Ctrl Pts',(4.05193666142919,-2.13043722405992,0.470465773785534));
#14638=CARTESIAN_POINT('Ctrl Pts',(4.30224631097138,-2.33254511812152,-2.01623620603559));
#14639=CARTESIAN_POINT('Ctrl Pts',(4.42874911942666,-2.67908579453452,-3.23054604201975));
#14640=CARTESIAN_POINT('Ctrl Pts',(4.67731276154541,-3.82242011052979,-5.45512593035675));
#14641=CARTESIAN_POINT('Ctrl Pts',(4.80534284562397,-4.60834831586048,-6.44384371054323));
#14642=CARTESIAN_POINT('Ctrl Pts',(5.05345105369771,-6.51294888414738,-8.05558738602805));
#14643=CARTESIAN_POINT('Ctrl Pts',(5.17914998170505,-7.61164297709098,-8.66512040772011));
#14644=CARTESIAN_POINT('Ctrl Pts',(5.42858604607204,-9.97718208881188,-9.42438672970812));
#14645=CARTESIAN_POINT('Ctrl Pts',(5.5514060490949,-11.2206160705921,-9.56855818217814));
#14646=CARTESIAN_POINT('Ctrl Pts',(5.80174320770436,-13.6902158568989,-9.37127791725014));
#14647=CARTESIAN_POINT('Ctrl Pts',(5.92290454188791,-14.8928618977337,-9.03256486454203));
#14648=CARTESIAN_POINT('Ctrl Pts',(6.17377777989577,-17.1006241722849,-7.91299494415882));
#14649=CARTESIAN_POINT('Ctrl Pts',(6.2945818874263,-18.0846226647122,-7.14274957259232));
#14650=CARTESIAN_POINT('Ctrl Pts',(6.54560447338455,-19.7034081654102,-5.2663025710902));
#14651=CARTESIAN_POINT('Ctrl Pts',(6.66735898898658,-20.3219530488362,-4.17739679312542));
#14652=CARTESIAN_POINT('Ctrl Pts',(6.89553917980856,-21.0362589525294,-2.03152410141216));
#14653=CARTESIAN_POINT('Ctrl Pts',(6.99935185262614,-21.2,-1.01843787290684));
#14654=CARTESIAN_POINT('Ctrl Pts',(7.10000000000035,-21.2,3.51135787113321E-12));
#14655=CARTESIAN_POINT('Origin',(78.0000000000001,-11.7,-3.46944695195361E-15));
#14656=CARTESIAN_POINT('',(13.1000000000002,-21.2,7.83235748155766E-13));
#14657=CARTESIAN_POINT('',(10.9,-21.2,7.85595533902485E-16));
#14658=CARTESIAN_POINT('',(78.0000000000001,-21.2,-4.6328614111436E-15));
#14659=CARTESIAN_POINT('Ctrl Pts',(10.9,-21.2,7.7715611723761E-15));
#14660=CARTESIAN_POINT('Ctrl Pts',(10.7792854883044,-21.2,-1.22148528043641));
#14661=CARTESIAN_POINT('Ctrl Pts',(10.6543248572149,-20.9644157250575,-2.4321655950274));
#14662=CARTESIAN_POINT('Ctrl Pts',(10.407311325678,-20.0379796864886,-4.72019166334919));
#14663=CARTESIAN_POINT('Ctrl Pts',(10.2830519498147,-19.3476995003354,-5.77191772591644));
#14664=CARTESIAN_POINT('Ctrl Pts',(10.0323229281731,-17.6042062462675,-7.54520943878787));
#14665=CARTESIAN_POINT('Ctrl Pts',(9.91037350082199,-16.569201506956,-8.25108999017969));
#14666=CARTESIAN_POINT('Ctrl Pts',(9.65935921798875,-14.2891812567478,-9.22382157527654));
#14667=CARTESIAN_POINT('Ctrl Pts',(9.53850996698144,-13.0664139465303,-9.48238228915556));
#14668=CARTESIAN_POINT('Ctrl Pts',(9.28759889551597,-10.5911524555272,-9.51587183654906));
#14669=CARTESIAN_POINT('Ctrl Pts',(9.16654819825315,-9.36229409907313,-9.29067738573375));
#14670=CARTESIAN_POINT('Ctrl Pts',(8.91612834663444,-7.05840175783301,-8.38103212678977));
#14671=CARTESIAN_POINT('Ctrl Pts',(8.79356951655815,-6.00563654506256,-7.70457444607858));
#14672=CARTESIAN_POINT('Ctrl Pts',(8.54400917814639,-4.21629480933593,-5.98259204016955));
#14673=CARTESIAN_POINT('Ctrl Pts',(8.41870882166755,-3.49816598006771,-4.9524098150449));
#14674=CARTESIAN_POINT('Ctrl Pts',(8.17042218264081,-2.49719213060868,-2.66851420318459));
#14675=CARTESIAN_POINT('Ctrl Pts',(8.04247821816483,-2.22627476101527,-1.43571070081323));
#14676=CARTESIAN_POINT('Ctrl Pts',(7.79423179979495,-2.17734057865527,1.06507476788044));
#14677=CARTESIAN_POINT('Ctrl Pts',(7.66729928940657,-2.4002422798638,2.3089465677553));
#14678=CARTESIAN_POINT('Ctrl Pts',(7.41707867178712,-3.31314727879806,4.63251285108547));
#14679=CARTESIAN_POINT('Ctrl Pts',(7.29333380378858,-3.99170948168188,5.69050173900259));
#14680=CARTESIAN_POINT('Ctrl Pts',(7.04252304168439,-5.71485444423867,7.48105206827982));
#14681=CARTESIAN_POINT('Ctrl Pts',(6.92087304401103,-6.74156121041404,8.19766790339052));
#14682=CARTESIAN_POINT('Ctrl Pts',(6.6698481269998,-9.0099170399777,9.19486269390218));
#14683=CARTESIAN_POINT('Ctrl Pts',(6.54906175941738,-10.2294916214256,9.46676421981236));
#14684=CARTESIAN_POINT('Ctrl Pts',(6.29821274278059,-12.7041409356648,9.52751127093405));
#14685=CARTESIAN_POINT('Ctrl Pts',(6.17697944446333,-13.9355883064947,9.31580037992616));
#14686=CARTESIAN_POINT('Ctrl Pts',(5.92669221714976,-16.2500729662693,8.431165739254));
#14687=CARTESIAN_POINT('Ctrl Pts',(5.80371405667179,-17.3106672228241,7.765832022934));
#14688=CARTESIAN_POINT('Ctrl Pts',(5.55435168263957,-19.1196837186759,6.06203761529587));
#14689=CARTESIAN_POINT('Ctrl Pts',(5.42841638903921,-19.8492914847689,5.03864619904479));
#14690=CARTESIAN_POINT('Ctrl Pts',(5.18041429727123,-20.8749735642952,2.76326935456466));
#14691=CARTESIAN_POINT('Ctrl Pts',(5.0523372362498,-21.158782162885,1.53206141455891));
#14692=CARTESIAN_POINT('Ctrl Pts',(4.91856146743405,-21.1986129794596,0.187503087496786));
#14693=CARTESIAN_POINT('Ctrl Pts',(4.90926253423132,-21.2,0.0937256760945501));
#14694=CARTESIAN_POINT('Ctrl Pts',(4.90000000000004,-21.2,3.87349497581765E-13));
#14695=CARTESIAN_POINT('Ctrl Pts',(7.10000000000035,-21.2,3.5166661249697E-12));
#14696=CARTESIAN_POINT('Ctrl Pts',(7.12207987122531,-21.2,0.223421669166213));
#14697=CARTESIAN_POINT('Ctrl Pts',(7.14435953967788,-21.1921185564034,0.44706615725391));
#14698=CARTESIAN_POINT('Ctrl Pts',(7.29223738335333,-21.0879231886111,1.91962968643776));
#14699=CARTESIAN_POINT('Ctrl Pts',(7.4194215259546,-20.7534347853916,3.13878541973641));
#14700=CARTESIAN_POINT('Ctrl Pts',(7.66748388707429,-19.6323975705467,5.37482152444833));
#14701=CARTESIAN_POINT('Ctrl Pts',(7.79537640986638,-18.8573834318446,6.3705072436837));
#14702=CARTESIAN_POINT('Ctrl Pts',(8.04376099233663,-16.971339193686,8.00053637136689));
#14703=CARTESIAN_POINT('Ctrl Pts',(8.16884187858872,-15.8800332301411,8.62111552010978));
#14704=CARTESIAN_POINT('Ctrl Pts',(8.41847066603455,-13.5243301865345,9.40518853940912));
#14705=CARTESIAN_POINT('Ctrl Pts',(8.54088889269013,-12.2831366735295,9.56271760385075));
#14706=CARTESIAN_POINT('Ctrl Pts',(8.79149441040546,-9.81088949960649,9.39234590031904));
#14707=CARTESIAN_POINT('Ctrl Pts',(8.91262867718373,-8.60345185493481,9.06620679395304));
#14708=CARTESIAN_POINT('Ctrl Pts',(9.16362762048596,-6.38328003924247,7.96954742471251));
#14709=CARTESIAN_POINT('Ctrl Pts',(9.28443993174331,-5.39150745569497,7.21000831202632));
#14710=CARTESIAN_POINT('Ctrl Pts',(9.53510054053434,-3.75443704287751,5.3527104438323));
#14711=CARTESIAN_POINT('Ctrl Pts',(9.65690697436105,-3.12503593325824,4.27243364780206));
#14712=CARTESIAN_POINT('Ctrl Pts',(9.90685108889982,-2.31520599857457,1.92813903140674));
#14713=CARTESIAN_POINT('Ctrl Pts',(10.0309222657915,-2.14380040857977,0.686156174599459));
#14714=CARTESIAN_POINT('Ctrl Pts',(10.2797987797144,-2.28882098605427,-1.7990740085523));
#14715=CARTESIAN_POINT('Ctrl Pts',(10.407291499593,-2.60619987947592,-3.01791987958328));
#14716=CARTESIAN_POINT('Ctrl Pts',(10.6545894668201,-3.69624114641017,-5.26902935946357));
#14717=CARTESIAN_POINT('Ctrl Pts',(10.7829140402373,-4.46092664668805,-6.27840347743013));
#14718=CARTESIAN_POINT('Ctrl Pts',(11.0326896878941,-6.33288154406691,-7.93722084228424));
#14719=CARTESIAN_POINT('Ctrl Pts',(11.1576048875106,-7.42028041952419,-8.57262399701104));
#14720=CARTESIAN_POINT('Ctrl Pts',(11.4082206192069,-9.77313248509324,-9.38505701203718));
#14721=CARTESIAN_POINT('Ctrl Pts',(11.5305782041576,-11.0151474070822,-9.55630141627986));
#14722=CARTESIAN_POINT('Ctrl Pts',(11.7815626432234,-13.491132676413,-9.41146479449907));
#14723=CARTESIAN_POINT('Ctrl Pts',(11.9025443344209,-14.7014737928496,-9.09806778344008));
#14724=CARTESIAN_POINT('Ctrl Pts',(12.1535115728152,-16.9326549830229,-8.02499048160666));
#14725=CARTESIAN_POINT('Ctrl Pts',(12.2744047432598,-17.9323602347771,-7.27591812466932));
#14726=CARTESIAN_POINT('Ctrl Pts',(12.5249650266106,-19.58914911386,-5.4356111079513));
#14727=CARTESIAN_POINT('Ctrl Pts',(12.6470831688779,-20.2300252432785,-4.36158171888695));
#14728=CARTESIAN_POINT('Ctrl Pts',(12.8814900909201,-21.0132140553034,-2.1684240907917));
#14729=CARTESIAN_POINT('Ctrl Pts',(12.992505504308,-21.2,-1.08771466140479));
#14730=CARTESIAN_POINT('Ctrl Pts',(13.1000000000002,-21.2,1.5656920204776E-12));
#14731=CARTESIAN_POINT('Origin',(78.0000000000001,-11.7,-3.46944695195361E-15));
#14732=CARTESIAN_POINT('',(28.,-21.2,-4.6328614111436E-15));
#14733=CARTESIAN_POINT('Origin',(28.,-11.7,-6.93889390390723E-15));
#14734=CARTESIAN_POINT('',(22.9,-21.2,-1.91609456404162E-13));
#14735=CARTESIAN_POINT('',(78.0000000000001,-21.2,-4.6328614111436E-15));
#14736=CARTESIAN_POINT('',(16.9,-21.2,-2.31643070557181E-15));
#14737=CARTESIAN_POINT('Ctrl Pts',(22.9,-21.2,-3.7858605139718E-13));
#14738=CARTESIAN_POINT('Ctrl Pts',(22.8907374657687,-21.2,-0.0937256760943193));
#14739=CARTESIAN_POINT('Ctrl Pts',(22.881438532566,-21.1986129794595,-0.187503087496334));
#14740=CARTESIAN_POINT('Ctrl Pts',(22.7476627637503,-21.158782162885,-1.53206141455819));
#14741=CARTESIAN_POINT('Ctrl Pts',(22.6195857027288,-20.8749735642953,-2.76326935456397));
#14742=CARTESIAN_POINT('Ctrl Pts',(22.3715836109608,-19.8492914847691,-5.03864619904417));
#14743=CARTESIAN_POINT('Ctrl Pts',(22.2456483173605,-19.1196837186763,-6.06203761529527));
#14744=CARTESIAN_POINT('Ctrl Pts',(21.9962859433283,-17.3106672228245,-7.76583202293353));
#14745=CARTESIAN_POINT('Ctrl Pts',(21.8733077828503,-16.2500729662698,-8.43116573925361));
#14746=CARTESIAN_POINT('Ctrl Pts',(21.6230205555367,-13.9355883064952,-9.31580037992593));
#14747=CARTESIAN_POINT('Ctrl Pts',(21.5017872572195,-12.7041409356653,-9.52751127093387));
#14748=CARTESIAN_POINT('Ctrl Pts',(21.2509382405827,-10.2294916214262,-9.46676421981232));
#14749=CARTESIAN_POINT('Ctrl Pts',(21.1301518730002,-9.00991703997824,-9.19486269390221));
#14750=CARTESIAN_POINT('Ctrl Pts',(20.879126955989,-6.74156121041469,-8.19766790339075));
#14751=CARTESIAN_POINT('Ctrl Pts',(20.7574769583157,-5.71485444423917,-7.48105206828012));
#14752=CARTESIAN_POINT('Ctrl Pts',(20.5066661962115,-3.9917094816822,-5.69050173900289));
#14753=CARTESIAN_POINT('Ctrl Pts',(20.3829213282129,-3.31314727879835,-4.63251285108579));
#14754=CARTESIAN_POINT('Ctrl Pts',(20.1327007105935,-2.40024227986406,-2.30894656775584));
#14755=CARTESIAN_POINT('Ctrl Pts',(20.0057682002051,-2.17734057865537,-1.06507476788092));
#14756=CARTESIAN_POINT('Ctrl Pts',(19.7575217818352,-2.22627476101527,1.43571070081289));
#14757=CARTESIAN_POINT('Ctrl Pts',(19.6295778173592,-2.49719213060867,2.66851420318429));
#14758=CARTESIAN_POINT('Ctrl Pts',(19.3812911783325,-3.49816598006761,4.9524098150446));
#14759=CARTESIAN_POINT('Ctrl Pts',(19.2559908218536,-4.21629480933581,5.98259204016927));
#14760=CARTESIAN_POINT('Ctrl Pts',(19.0064304834419,-6.00563654506237,7.70457444607833));
#14761=CARTESIAN_POINT('Ctrl Pts',(18.8838716533656,-7.05840175783278,8.38103212678955));
#14762=CARTESIAN_POINT('Ctrl Pts',(18.6334518017469,-9.36229409907291,9.29067738573362));
#14763=CARTESIAN_POINT('Ctrl Pts',(18.512401104484,-10.591152455527,9.51587183654894));
#14764=CARTESIAN_POINT('Ctrl Pts',(18.2614900330186,-13.06641394653,9.48238228915551));
#14765=CARTESIAN_POINT('Ctrl Pts',(18.1406407820113,-14.2891812567475,9.22382157527653));
#14766=CARTESIAN_POINT('Ctrl Pts',(17.889626499178,-16.5692015069559,8.25108999017968));
#14767=CARTESIAN_POINT('Ctrl Pts',(17.7676770718269,-17.6042062462674,7.54520943878787));
#14768=CARTESIAN_POINT('Ctrl Pts',(17.5169480501853,-19.3476995003353,5.77191772591642));
#14769=CARTESIAN_POINT('Ctrl Pts',(17.392688674322,-20.0379796864885,4.72019166334919));
#14770=CARTESIAN_POINT('Ctrl Pts',(17.1456751427851,-20.9644157250573,2.4321655950276));
#14771=CARTESIAN_POINT('Ctrl Pts',(17.0207145116956,-21.2,1.22148528043652));
#14772=CARTESIAN_POINT('Ctrl Pts',(16.9,-21.2,8.32667268468867E-16));
#14773=CARTESIAN_POINT('',(19.1,-21.2,1.55474016669278E-13));
#14774=CARTESIAN_POINT('',(78.0000000000001,-21.2,-4.6328614111436E-15));
#14775=CARTESIAN_POINT('',(22.1,-2.2,0.));
#14776=CARTESIAN_POINT('Ctrl Pts',(19.1,-21.2,3.155808947497E-13));
#14777=CARTESIAN_POINT('Ctrl Pts',(19.1085990463697,-21.2,0.0870119790806313));
#14778=CARTESIAN_POINT('Ctrl Pts',(19.117229491272,-21.1988045700926,0.174068824370104));
#14779=CARTESIAN_POINT('Ctrl Pts',(19.250254599823,-21.1620196858175,1.51172658899612));
#14780=CARTESIAN_POINT('Ctrl Pts',(19.3783048394584,-20.8809326818491,2.74328431513305));
#14781=CARTESIAN_POINT('Ctrl Pts',(19.6269445678301,-19.8580958285676,5.02576267739737));
#14782=CARTESIAN_POINT('Ctrl Pts',(19.7533450987224,-19.1265285069368,6.05479514661026));
#14783=CARTESIAN_POINT('Ctrl Pts',(20.0036755920597,-17.3113998082999,7.76593089658135));
#14784=CARTESIAN_POINT('Ctrl Pts',(20.1270389541067,-16.2472803988743,8.43325057572791));
#14785=CARTESIAN_POINT('Ctrl Pts',(20.3779053449636,-13.9266113917878,9.31821156840541));
#14786=CARTESIAN_POINT('Ctrl Pts',(20.499348010147,-12.6929414155417,9.52894055092275));
#14787=CARTESIAN_POINT('Ctrl Pts',(20.7503716367565,-10.2165695573798,9.46472746246329));
#14788=CARTESIAN_POINT('Ctrl Pts',(20.8711406833289,-8.99752494041226,9.191206657545));
#14789=CARTESIAN_POINT('Ctrl Pts',(21.1219308163566,-6.73272231199642,8.19197178741145));
#14790=CARTESIAN_POINT('Ctrl Pts',(21.2433410956421,-5.70863128218638,7.47569272702411));
#14791=CARTESIAN_POINT('Ctrl Pts',(21.4935141130515,-3.99107778358669,5.6887303718073));
#14792=CARTESIAN_POINT('Ctrl Pts',(21.6168550679505,-3.3148092474812,4.63439611874689));
#14793=CARTESIAN_POINT('Ctrl Pts',(21.8605525202926,-2.424049175255,2.37178196627815));
#14794=CARTESIAN_POINT('Ctrl Pts',(21.9822771983424,-2.2,1.19121278276015));
#14795=CARTESIAN_POINT('Ctrl Pts',(22.1,-2.2,1.66533453693773E-15));
#14796=CARTESIAN_POINT('',(25.9,-2.20000000000001,-1.38777878078145E-14));
#14797=CARTESIAN_POINT('',(78.0000000000001,-2.19999999999999,-1.38777878078145E-14));
#14798=CARTESIAN_POINT('Ctrl Pts',(25.9,-2.2,-1.26287869051112E-14));
#14799=CARTESIAN_POINT('Ctrl Pts',(25.8320584301578,-2.2,0.687486751395677));
#14800=CARTESIAN_POINT('Ctrl Pts',(25.7626425064763,-2.27462673223733,1.37285912097331));
#14801=CARTESIAN_POINT('Ctrl Pts',(25.6232454680745,-2.57052382279369,2.71585246112393));
#14802=CARTESIAN_POINT('Ctrl Pts',(25.5536591008349,-2.79107732111416,3.36964268186213));
#14803=CARTESIAN_POINT('Ctrl Pts',(25.3619357157689,-3.60400801504387,5.12410600030646));
#14804=CARTESIAN_POINT('Ctrl Pts',(25.2353260823093,-4.34505010391429,6.14065935137735));
#14805=CARTESIAN_POINT('Ctrl Pts',(24.9861739757012,-6.17366151377811,7.82617419694253));
#14806=CARTESIAN_POINT('Ctrl Pts',(24.8627326460084,-7.24203907542681,8.48033707933684));
#14807=CARTESIAN_POINT('Ctrl Pts',(24.612591160184,-9.56702001222319,9.33986229220453));
#14808=CARTESIAN_POINT('Ctrl Pts',(24.4911293307759,-10.801000518419,9.53803958026865));
#14809=CARTESIAN_POINT('Ctrl Pts',(24.2403562347155,-13.2749008689799,9.44993444082386));
#14810=CARTESIAN_POINT('Ctrl Pts',(24.1195868569151,-14.4912108845082,9.16464314019057));
#14811=CARTESIAN_POINT('Ctrl Pts',(23.868565051285,-16.7477137680785,8.14290619632623));
#14812=CARTESIAN_POINT('Ctrl Pts',(23.7471727049711,-17.7660153225652,7.41552521022505));
#14813=CARTESIAN_POINT('Ctrl Pts',(23.4962929725926,-19.468575729199,5.60768898329955));
#14814=CARTESIAN_POINT('Ctrl Pts',(23.3730265024687,-20.1352887413488,4.54344435292872));
#14815=CARTESIAN_POINT('Ctrl Pts',(23.132091158415,-20.9895203441915,2.3004420205563));
#14816=CARTESIAN_POINT('Ctrl Pts',(23.0141053600769,-21.2,1.15460863648514));
#14817=CARTESIAN_POINT('Ctrl Pts',(22.9,-21.2,-3.81361608958741E-13));
#14818=CARTESIAN_POINT('Origin',(-58.,-11.7,0.));
#14819=CARTESIAN_POINT('',(-57.5,-19.2,-4.38793205131413E-15));
#14820=CARTESIAN_POINT('',(-57.5,-11.7,7.5));
#14821=CARTESIAN_POINT('Origin',(-57.5,-11.7,-6.93889390390723E-15));
#14822=CARTESIAN_POINT('Origin',(-57.5,-11.7,-6.93889390390723E-15));
#14823=CARTESIAN_POINT('',(-58.,-11.7,7.));
#14824=CARTESIAN_POINT('',(-58.,-11.7,7.));
#14825=CARTESIAN_POINT('Origin',(-58.,-11.7,0.));
#14826=CARTESIAN_POINT('Origin',(78.0000000000001,-11.7,-3.46944695195361E-15));
#14827=CARTESIAN_POINT('',(108.,-4.37815767719625,-1.62500000000001));
#14828=CARTESIAN_POINT('',(108.,-4.37815767719625,1.625));
#14829=CARTESIAN_POINT('Origin',(108.,-11.7,0.));
#14830=CARTESIAN_POINT('',(128.,-4.37815767719625,-1.625));
#14831=CARTESIAN_POINT('',(78.0000000000001,-4.37815767719626,-1.625));
#14832=CARTESIAN_POINT('',(128.,-19.2,-4.38793205131413E-15));
#14833=CARTESIAN_POINT('Origin',(128.,-11.7,-3.46944695195361E-15));
#14834=CARTESIAN_POINT('',(57.,-19.2,-4.38793205131413E-15));
#14835=CARTESIAN_POINT('',(78.0000000000001,-19.2,-4.38793205131413E-15));
#14836=CARTESIAN_POINT('Origin',(57.,-11.7,0.));
#14837=CARTESIAN_POINT('',(128.,-4.37815767719625,1.62499999999998));
#14838=CARTESIAN_POINT('Origin',(128.,-11.7,-3.46944695195361E-15));
#14839=CARTESIAN_POINT('',(78.,-4.37815767719627,1.62500000000001));
#14840=CARTESIAN_POINT('Origin',(78.0000000000001,-11.7,-3.46944695195361E-15));
#14841=CARTESIAN_POINT('',(57.,-19.7,-4.4491643912715E-15));
#14842=CARTESIAN_POINT('Origin',(57.,-11.7,0.));
#14843=CARTESIAN_POINT('',(28.,-19.7,-4.4491643912715E-15));
#14844=CARTESIAN_POINT('',(78.0000000000001,-19.7,-4.4491643912715E-15));
#14845=CARTESIAN_POINT('Origin',(28.,-11.7,-6.93889390390723E-15));
#14846=CARTESIAN_POINT('Origin',(78.0000000000001,-11.7,-3.46944695195361E-15));
#14847=CARTESIAN_POINT('',(-28.,-19.2,-4.38793205131413E-15));
#14848=CARTESIAN_POINT('Origin',(-28.,-11.7,-1.38777878078145E-14));
#14849=CARTESIAN_POINT('',(78.0000000000001,-19.2,-4.38793205131413E-15));
#14850=CARTESIAN_POINT('Origin',(78.0000000000001,-11.7,-3.46944695195361E-15));
#14851=CARTESIAN_POINT('Ctrl Pts',(16.9,-21.2,-8.2367941628566E-30));
#14852=CARTESIAN_POINT('Ctrl Pts',(16.8969830453883,-21.2,-0.0305279423179098));
#14853=CARTESIAN_POINT('Ctrl Pts',(16.8939621685952,-21.1998528492312,-0.061061986178079));
#14854=CARTESIAN_POINT('Ctrl Pts',(16.767248128974,-21.1875162370895,-1.34043950276093));
#14855=CARTESIAN_POINT('Ctrl Pts',(16.6394486076613,-20.9293291909709,-2.57468702777392));
#14856=CARTESIAN_POINT('Ctrl Pts',(16.390901029389,-19.9527852055101,-4.86679898715219));
#14857=CARTESIAN_POINT('Ctrl Pts',(16.2661865852166,-19.2459958496646,-5.90361775701915));
#14858=CARTESIAN_POINT('Ctrl Pts',(16.0164434579476,-17.4760938667979,-7.64340926548421));
#14859=CARTESIAN_POINT('Ctrl Pts',(15.8942543732133,-16.4310772867914,-8.33076824399945));
#14860=CARTESIAN_POINT('Ctrl Pts',(15.643716791377,-14.1377024264444,-9.26493007649783));
#14861=CARTESIAN_POINT('Ctrl Pts',(15.5228012264078,-12.9114457325454,-9.50334490259741));
#14862=CARTESIAN_POINT('Ctrl Pts',(15.2718422511462,-10.4357116660552,-9.49658163777804));
#14863=CARTESIAN_POINT('Ctrl Pts',(15.1508875962576,-9.20987735813006,-9.25110322734291));
#14864=CARTESIAN_POINT('Ctrl Pts',(14.8998967426513,-6.91855760852242,-8.30236799838266));
#14865=CARTESIAN_POINT('Ctrl Pts',(14.7776129198827,-5.87549075136839,-7.60702303698612));
#14866=CARTESIAN_POINT('Ctrl Pts',(14.5269765839982,-4.11220036693074,-5.85068851113425));
#14867=CARTESIAN_POINT('Ctrl Pts',(14.402176887142,-3.41051525358193,-4.80513228098754));
#14868=CARTESIAN_POINT('Ctrl Pts',(14.152310008838,-2.4484427730648,-2.49636756975503));
#14869=CARTESIAN_POINT('Ctrl Pts',(14.023965795097,-2.2,-1.25438434751197));
#14870=CARTESIAN_POINT('Ctrl Pts',(13.7760812749615,-2.2,1.253908055286));
#14871=CARTESIAN_POINT('Ctrl Pts',(13.6477361899215,-2.44826489212498,2.495940694187));
#14872=CARTESIAN_POINT('Ctrl Pts',(13.397823112858,-3.41051525358195,4.8051322809876));
#14873=CARTESIAN_POINT('Ctrl Pts',(13.2730234160018,-4.11220036693081,5.8506885111343));
#14874=CARTESIAN_POINT('Ctrl Pts',(13.0223870801173,-5.87549075136832,7.60702303698604));
#14875=CARTESIAN_POINT('Ctrl Pts',(12.9001032573487,-6.91855760852222,8.30236799838261));
#14876=CARTESIAN_POINT('Ctrl Pts',(12.6491124037424,-9.20987735813006,9.25110322734295));
#14877=CARTESIAN_POINT('Ctrl Pts',(12.5281577488538,-10.4357116660552,9.49658163777806));
#14878=CARTESIAN_POINT('Ctrl Pts',(12.2771987735922,-12.9114457325453,9.50334490259743));
#14879=CARTESIAN_POINT('Ctrl Pts',(12.156283208623,-14.1377024264444,9.26493007649789));
#14880=CARTESIAN_POINT('Ctrl Pts',(11.9057456267867,-16.4310772867913,8.33076824399952));
#14881=CARTESIAN_POINT('Ctrl Pts',(11.7835565420523,-17.4760938667978,7.64340926548429));
#14882=CARTESIAN_POINT('Ctrl Pts',(11.5338134147833,-19.2459958496645,5.90361775701927));
#14883=CARTESIAN_POINT('Ctrl Pts',(11.4090989706109,-19.9527852055101,4.86679898715229));
#14884=CARTESIAN_POINT('Ctrl Pts',(11.1605513923387,-20.929329190971,2.574687027774));
#14885=CARTESIAN_POINT('Ctrl Pts',(11.032751871026,-21.1875162370896,1.340439502761));
#14886=CARTESIAN_POINT('Ctrl Pts',(10.9060378314048,-21.1998528492313,0.0610619861781323));
#14887=CARTESIAN_POINT('Ctrl Pts',(10.9030169546117,-21.2,0.0305279423179378));
#14888=CARTESIAN_POINT('Ctrl Pts',(10.9,-21.2,6.20405247894856E-15));
#14889=CARTESIAN_POINT('Ctrl Pts',(13.1000000000002,-21.2,1.5694563704205E-12));
#14890=CARTESIAN_POINT('Ctrl Pts',(13.1150618716887,-21.2,0.152407977343253));
#14891=CARTESIAN_POINT('Ctrl Pts',(13.1302184694214,-21.1963324367572,0.304937370638801));
#14892=CARTESIAN_POINT('Ctrl Pts',(13.2700599843257,-21.1288573016021,1.70456409769737));
#14893=CARTESIAN_POINT('Ctrl Pts',(13.3978280547826,-20.8234635749735,2.92771876120427));
#14894=CARTESIAN_POINT('Ctrl Pts',(13.6454592566918,-19.755260072567,5.18963741030103));
#14895=CARTESIAN_POINT('Ctrl Pts',(13.7732390331541,-19.0012386404909,6.20590007975632));
#14896=CARTESIAN_POINT('Ctrl Pts',(14.0232777368833,-17.1471853740769,7.88231274196907));
#14897=CARTESIAN_POINT('Ctrl Pts',(14.1476486571035,-16.0673203360107,8.52815677935463));
#14898=CARTESIAN_POINT('Ctrl Pts',(14.3983590751342,-13.7248517892438,9.36430425037921));
#14899=CARTESIAN_POINT('Ctrl Pts',(14.520375998781,-12.4854983155022,9.54845471360794));
#14900=CARTESIAN_POINT('Ctrl Pts',(14.7713863912166,-10.0092570137193,9.42996830424106));
#14901=CARTESIAN_POINT('Ctrl Pts',(14.8922543670058,-8.79600881109443,9.1296032176108));
#14902=CARTESIAN_POINT('Ctrl Pts',(15.1431766592368,-6.55370184479103,8.08065075646646));
#14903=CARTESIAN_POINT('Ctrl Pts',(15.2641950892462,-5.54595419660828,7.34228914700703));
#14904=CARTESIAN_POINT('Ctrl Pts',(15.5146409061442,-3.86915103688522,5.51938731615909));
#14905=CARTESIAN_POINT('Ctrl Pts',(15.6371179553,-3.21662243900297,4.4517706334838));
#14906=CARTESIAN_POINT('Ctrl Pts',(15.8867179619448,-2.35695918963997,2.12233210287465));
#14907=CARTESIAN_POINT('Ctrl Pts',(16.0118911216994,-2.15969596306437,0.882356458430438));
#14908=CARTESIAN_POINT('Ctrl Pts',(16.2602345530853,-2.25420339436364,-1.60900886831394));
#14909=CARTESIAN_POINT('Ctrl Pts',(16.3881490721731,-2.5475691743667,-2.8363907156804));
#14910=CARTESIAN_POINT('Ctrl Pts',(16.6362896776214,-3.59330951586658,-5.10859098415954));
#14911=CARTESIAN_POINT('Ctrl Pts',(16.7633666485782,-4.33619714865433,-6.13122431775599));
#14912=CARTESIAN_POINT('Ctrl Pts',(17.0135568268943,-6.17095257434411,-7.82493779010911));
#14913=CARTESIAN_POINT('Ctrl Pts',(17.1374069120597,-7.24301853066505,-8.48147631282628));
#14914=CARTESIAN_POINT('Ctrl Pts',(17.3882015412574,-9.57470582039923,-9.34192598080633));
#14915=CARTESIAN_POINT('Ctrl Pts',(17.5099110598593,-10.8112640706003,-9.53930664709422));
#14916=CARTESIAN_POINT('Ctrl Pts',(17.7609348528615,-13.2876375702419,-9.44783485576954));
#14917=CARTESIAN_POINT('Ctrl Pts',(17.8817307023484,-14.5038018029798,-9.16083147073306));
#14918=CARTESIAN_POINT('Ctrl Pts',(18.1325938901276,-16.7573768406909,-8.13662124256136));
#14919=CARTESIAN_POINT('Ctrl Pts',(18.2537849940001,-17.7732966317507,-7.40924768217617));
#14920=CARTESIAN_POINT('Ctrl Pts',(18.5041011927066,-19.4704623912838,-5.60421999604294));
#14921=CARTESIAN_POINT('Ctrl Pts',(18.6269875482744,-20.1348513062228,-4.54320233464012));
#14922=CARTESIAN_POINT('Ctrl Pts',(18.8676457342621,-20.9890409731633,-2.30299493605579));
#14923=CARTESIAN_POINT('Ctrl Pts',(18.9857650877243,-21.2,-1.15591954850146));
#14924=CARTESIAN_POINT('Ctrl Pts',(19.1,-21.2,3.13915560212763E-13));
#14925=CARTESIAN_POINT('Origin',(-28.,-4.2,-6.93889390390723E-15));
#14926=CARTESIAN_POINT('Origin',(28.,-2.2,3.46944695195361E-15));
#14927=CARTESIAN_POINT('Origin',(57.,-3.69999999999999,-2.08166817117217E-14));
#14928=CARTESIAN_POINT('Origin',(24.,2.3,-3.46944695195361E-15));
#14929=CARTESIAN_POINT('',(24.9704939903643,1.5411253090549,0.));
#14930=CARTESIAN_POINT('',(25.4352469951821,-0.329437345472555,0.));
#14931=CARTESIAN_POINT('',(23.0295060096357,1.5411253090549,0.));
#14932=CARTESIAN_POINT('',(22.5647530048179,-0.329437345472541,-2.08166817117217E-14));
#14933=CARTESIAN_POINT('Origin',(24.,1.3,-6.93889390390723E-15));
#14934=CARTESIAN_POINT('Ctrl Pts',(-0.97049399036428,1.5411253090549,-6.93889390390723E-15));
#14935=CARTESIAN_POINT('Ctrl Pts',(-0.756208276078568,1.5411253090549,-3.02220044537404));
#14936=CARTESIAN_POINT('Ctrl Pts',(-0.541922561792853,0.229841679453259,
-5.74510895921687));
#14937=CARTESIAN_POINT('Ctrl Pts',(-0.327636847507138,-1.08144195014838,
-8.4680174730597));
#14938=CARTESIAN_POINT('Ctrl Pts',(-0.113351133221425,-3.4442934046707,
-10.3523286299233));
#14939=CARTESIAN_POINT('Ctrl Pts',(0.100934581064289,-5.80714485919302,
-12.236639786787));
#14940=CARTESIAN_POINT('Ctrl Pts',(0.315220295350005,-8.75357242959651,
-12.9091426524948));
#14941=CARTESIAN_POINT('Ctrl Pts',(0.529506009635718,-11.7,-13.5816455182026));
#14942=CARTESIAN_POINT('Ctrl Pts',(0.743791723921435,-14.6464275704035,
-12.9091426524948));
#14943=CARTESIAN_POINT('Ctrl Pts',(0.958077438207147,-17.592855140807,-12.236639786787));
#14944=CARTESIAN_POINT('Ctrl Pts',(1.17236315249286,-19.9557065953293,-10.3523286299233));
#14945=CARTESIAN_POINT('Ctrl Pts',(1.38664886677857,-22.3185580498516,-8.4680174730597));
#14946=CARTESIAN_POINT('Ctrl Pts',(1.60093458106429,-23.6298416794532,-5.74510895921687));
#14947=CARTESIAN_POINT('Ctrl Pts',(1.81522029535,-24.9411253090549,-3.02220044537404));
#14948=CARTESIAN_POINT('Ctrl Pts',(2.02950600963572,-24.9411253090549,6.93889390390723E-15));
#14949=CARTESIAN_POINT('Ctrl Pts',(2.24379172392143,-24.9411253090549,3.02220044537403));
#14950=CARTESIAN_POINT('Ctrl Pts',(2.45807743820715,-23.6298416794532,5.74510895921686));
#14951=CARTESIAN_POINT('Ctrl Pts',(2.67236315249286,-22.3185580498516,8.4680174730597));
#14952=CARTESIAN_POINT('Ctrl Pts',(2.88664886677858,-19.9557065953293,10.3523286299233));
#14953=CARTESIAN_POINT('Ctrl Pts',(3.10093458106429,-17.592855140807,12.236639786787));
#14954=CARTESIAN_POINT('Ctrl Pts',(3.31522029535001,-14.6464275704035,12.9091426524948));
#14955=CARTESIAN_POINT('Ctrl Pts',(3.52950600963572,-11.7,13.5816455182026));
#14956=CARTESIAN_POINT('Ctrl Pts',(3.74379172392143,-8.7535724295965,12.9091426524948));
#14957=CARTESIAN_POINT('Ctrl Pts',(3.95807743820715,-5.80714485919301,12.236639786787));
#14958=CARTESIAN_POINT('Ctrl Pts',(4.17236315249286,-3.4442934046707,10.3523286299233));
#14959=CARTESIAN_POINT('Ctrl Pts',(4.38664886677858,-1.08144195014837,8.46801747305969));
#14960=CARTESIAN_POINT('Ctrl Pts',(4.60093458106429,0.229841679453252,5.74510895921686));
#14961=CARTESIAN_POINT('Ctrl Pts',(4.81522029535,1.5411253090549,3.02220044537404));
#14962=CARTESIAN_POINT('Ctrl Pts',(5.02950600963572,1.5411253090549,0.));
#14963=CARTESIAN_POINT('Ctrl Pts',(5.24379172392143,1.5411253090549,-3.02220044537404));
#14964=CARTESIAN_POINT('Ctrl Pts',(5.45807743820715,0.229841679453252,-5.74510895921687));
#14965=CARTESIAN_POINT('Ctrl Pts',(5.67236315249286,-1.08144195014837,-8.4680174730597));
#14966=CARTESIAN_POINT('Ctrl Pts',(5.88664886677858,-3.4442934046707,-10.3523286299233));
#14967=CARTESIAN_POINT('Ctrl Pts',(6.10093458106429,-5.80714485919301,-12.236639786787));
#14968=CARTESIAN_POINT('Ctrl Pts',(6.31522029535001,-8.75357242959651,-12.9091426524948));
#14969=CARTESIAN_POINT('Ctrl Pts',(6.52950600963572,-11.7,-13.5816455182026));
#14970=CARTESIAN_POINT('Ctrl Pts',(6.74379172392144,-14.6464275704035,-12.9091426524948));
#14971=CARTESIAN_POINT('Ctrl Pts',(6.95807743820715,-17.592855140807,-12.236639786787));
#14972=CARTESIAN_POINT('Ctrl Pts',(7.17236315249286,-19.9557065953293,-10.3523286299233));
#14973=CARTESIAN_POINT('Ctrl Pts',(7.38664886677858,-22.3185580498516,-8.4680174730597));
#14974=CARTESIAN_POINT('Ctrl Pts',(7.60093458106429,-23.6298416794532,-5.74510895921687));
#14975=CARTESIAN_POINT('Ctrl Pts',(7.81522029535,-24.9411253090549,-3.02220044537404));
#14976=CARTESIAN_POINT('Ctrl Pts',(8.02950600963572,-24.9411253090549,-6.93889390390723E-15));
#14977=CARTESIAN_POINT('Ctrl Pts',(8.24379172392143,-24.9411253090549,3.02220044537402));
#14978=CARTESIAN_POINT('Ctrl Pts',(8.45807743820715,-23.6298416794532,5.74510895921685));
#14979=CARTESIAN_POINT('Ctrl Pts',(8.67236315249286,-22.3185580498516,8.4680174730597));
#14980=CARTESIAN_POINT('Ctrl Pts',(8.88664886677858,-19.9557065953293,10.3523286299233));
#14981=CARTESIAN_POINT('Ctrl Pts',(9.10093458106429,-17.592855140807,12.236639786787));
#14982=CARTESIAN_POINT('Ctrl Pts',(9.31522029535001,-14.6464275704035,12.9091426524948));
#14983=CARTESIAN_POINT('Ctrl Pts',(9.52950600963572,-11.7,13.5816455182026));
#14984=CARTESIAN_POINT('Ctrl Pts',(9.74379172392144,-8.75357242959651,12.9091426524948));
#14985=CARTESIAN_POINT('Ctrl Pts',(9.95807743820714,-5.80714485919302,12.236639786787));
#14986=CARTESIAN_POINT('Ctrl Pts',(10.1723631524929,-3.4442934046707,10.3523286299233));
#14987=CARTESIAN_POINT('Ctrl Pts',(10.3866488667786,-1.08144195014837,8.4680174730597));
#14988=CARTESIAN_POINT('Ctrl Pts',(10.6009345810643,0.229841679453252,5.74510895921686));
#14989=CARTESIAN_POINT('Ctrl Pts',(10.81522029535,1.5411253090549,3.02220044537402));
#14990=CARTESIAN_POINT('Ctrl Pts',(11.0295060096357,1.5411253090549,6.93889390390723E-15));
#14991=CARTESIAN_POINT('Ctrl Pts',(11.2437917239214,1.54112530905489,-3.02220044537404));
#14992=CARTESIAN_POINT('Ctrl Pts',(11.4580774382071,0.229841679453259,-5.74510895921686));
#14993=CARTESIAN_POINT('Ctrl Pts',(11.6723631524929,-1.08144195014837,-8.4680174730597));
#14994=CARTESIAN_POINT('Ctrl Pts',(11.8866488667786,-3.4442934046707,-10.3523286299233));
#14995=CARTESIAN_POINT('Ctrl Pts',(12.1009345810643,-5.80714485919302,-12.236639786787));
#14996=CARTESIAN_POINT('Ctrl Pts',(12.31522029535,-8.75357242959649,-12.9091426524948));
#14997=CARTESIAN_POINT('Ctrl Pts',(12.5295060096357,-11.7,-13.5816455182026));
#14998=CARTESIAN_POINT('Ctrl Pts',(12.7437917239214,-14.6464275704035,-12.9091426524948));
#14999=CARTESIAN_POINT('Ctrl Pts',(12.9580774382071,-17.592855140807,-12.236639786787));
#15000=CARTESIAN_POINT('Ctrl Pts',(13.1723631524929,-19.9557065953293,-10.3523286299233));
#15001=CARTESIAN_POINT('Ctrl Pts',(13.3866488667786,-22.3185580498516,-8.4680174730597));
#15002=CARTESIAN_POINT('Ctrl Pts',(13.6009345810643,-23.6298416794532,-5.74510895921687));
#15003=CARTESIAN_POINT('Ctrl Pts',(13.81522029535,-24.9411253090549,-3.02220044537403));
#15004=CARTESIAN_POINT('Ctrl Pts',(14.0295060096357,-24.9411253090549,-6.93889390390723E-15));
#15005=CARTESIAN_POINT('Ctrl Pts',(14.2437917239214,-24.9411253090549,3.02220044537403));
#15006=CARTESIAN_POINT('Ctrl Pts',(14.4580774382072,-23.6298416794532,5.74510895921685));
#15007=CARTESIAN_POINT('Ctrl Pts',(14.6723631524929,-22.3185580498516,8.46801747305969));
#15008=CARTESIAN_POINT('Ctrl Pts',(14.8866488667786,-19.9557065953293,10.3523286299233));
#15009=CARTESIAN_POINT('Ctrl Pts',(15.1009345810643,-17.592855140807,12.236639786787));
#15010=CARTESIAN_POINT('Ctrl Pts',(15.31522029535,-14.6464275704035,12.9091426524948));
#15011=CARTESIAN_POINT('Ctrl Pts',(15.5295060096357,-11.7,13.5816455182026));
#15012=CARTESIAN_POINT('Ctrl Pts',(15.7437917239214,-8.75357242959651,12.9091426524948));
#15013=CARTESIAN_POINT('Ctrl Pts',(15.9580774382071,-5.80714485919302,12.236639786787));
#15014=CARTESIAN_POINT('Ctrl Pts',(16.1723631524929,-3.4442934046707,10.3523286299233));
#15015=CARTESIAN_POINT('Ctrl Pts',(16.3866488667786,-1.08144195014837,8.46801747305969));
#15016=CARTESIAN_POINT('Ctrl Pts',(16.6009345810643,0.229841679453266,5.74510895921686));
#15017=CARTESIAN_POINT('Ctrl Pts',(16.81522029535,1.5411253090549,3.02220044537404));
#15018=CARTESIAN_POINT('Ctrl Pts',(17.0295060096357,1.5411253090549,-2.08166817117217E-14));
#15019=CARTESIAN_POINT('Ctrl Pts',(17.2437917239214,1.5411253090549,-3.02220044537405));
#15020=CARTESIAN_POINT('Ctrl Pts',(17.4580774382072,0.229841679453266,-5.74510895921688));
#15021=CARTESIAN_POINT('Ctrl Pts',(17.6723631524929,-1.08144195014837,-8.46801747305971));
#15022=CARTESIAN_POINT('Ctrl Pts',(17.8866488667786,-3.44429340467071,-10.3523286299233));
#15023=CARTESIAN_POINT('Ctrl Pts',(18.1009345810643,-5.80714485919302,-12.236639786787));
#15024=CARTESIAN_POINT('Ctrl Pts',(18.31522029535,-8.75357242959651,-12.9091426524948));
#15025=CARTESIAN_POINT('Ctrl Pts',(18.5295060096357,-11.7,-13.5816455182026));
#15026=CARTESIAN_POINT('Ctrl Pts',(18.7437917239214,-14.6464275704035,-12.9091426524948));
#15027=CARTESIAN_POINT('Ctrl Pts',(18.9580774382071,-17.592855140807,-12.236639786787));
#15028=CARTESIAN_POINT('Ctrl Pts',(19.1723631524929,-19.9557065953293,-10.3523286299233));
#15029=CARTESIAN_POINT('Ctrl Pts',(19.3866488667786,-22.3185580498516,-8.4680174730597));
#15030=CARTESIAN_POINT('Ctrl Pts',(19.6009345810643,-23.6298416794532,-5.74510895921687));
#15031=CARTESIAN_POINT('Ctrl Pts',(19.81522029535,-24.9411253090549,-3.02220044537404));
#15032=CARTESIAN_POINT('Ctrl Pts',(20.0295060096357,-24.9411253090549,0.));
#15033=CARTESIAN_POINT('Ctrl Pts',(20.2437917239214,-24.9411253090549,3.02220044537403));
#15034=CARTESIAN_POINT('Ctrl Pts',(20.4580774382071,-23.6298416794532,5.74510895921685));
#15035=CARTESIAN_POINT('Ctrl Pts',(20.6723631524929,-22.3185580498516,8.46801747305969));
#15036=CARTESIAN_POINT('Ctrl Pts',(20.8866488667786,-19.9557065953293,10.3523286299233));
#15037=CARTESIAN_POINT('Ctrl Pts',(21.1009345810643,-17.5928551408069,12.236639786787));
#15038=CARTESIAN_POINT('Ctrl Pts',(21.31522029535,-14.6464275704035,12.9091426524948));
#15039=CARTESIAN_POINT('Ctrl Pts',(21.5295060096357,-11.7,13.5816455182026));
#15040=CARTESIAN_POINT('Ctrl Pts',(21.7437917239214,-8.75357242959651,12.9091426524948));
#15041=CARTESIAN_POINT('Ctrl Pts',(21.9580774382071,-5.80714485919301,12.236639786787));
#15042=CARTESIAN_POINT('Ctrl Pts',(22.1723631524929,-3.4442934046707,10.3523286299233));
#15043=CARTESIAN_POINT('Ctrl Pts',(22.3866488667786,-1.08144195014837,8.4680174730597));
#15044=CARTESIAN_POINT('Ctrl Pts',(22.6009345810643,0.229841679453259,5.74510895921686));
#15045=CARTESIAN_POINT('Ctrl Pts',(22.81522029535,1.54112530905491,3.02220044537404));
#15046=CARTESIAN_POINT('Ctrl Pts',(23.0295060096357,1.5411253090549,0.));
#15047=CARTESIAN_POINT('Ctrl Pts',(-1.9,-2.2,0.));
#15048=CARTESIAN_POINT('Ctrl Pts',(-1.68571428571429,-2.19999999999999,
-2.16831300670641));
#15049=CARTESIAN_POINT('Ctrl Pts',(-1.47142857142857,-3.14079575492701,
-4.1218955216168));
#15050=CARTESIAN_POINT('Ctrl Pts',(-1.25714285714286,-4.08159150985404,
-6.07547803652718));
#15051=CARTESIAN_POINT('Ctrl Pts',(-1.04285714285715,-5.77684688234203,
-7.42739908344627));
#15052=CARTESIAN_POINT('Ctrl Pts',(-0.828571428571431,-7.47210225483002,
-8.77932013036538));
#15053=CARTESIAN_POINT('Ctrl Pts',(-0.614285714285715,-9.58605112741501,
-9.26181516572732));
#15054=CARTESIAN_POINT('Ctrl Pts',(-0.400000000000003,-11.7,-9.74431020108925));
#15055=CARTESIAN_POINT('Ctrl Pts',(-0.185714285714288,-13.813948872585,
-9.26181516572733));
#15056=CARTESIAN_POINT('Ctrl Pts',(0.0285714285714265,-15.92789774517,-8.7793201303654));
#15057=CARTESIAN_POINT('Ctrl Pts',(0.242857142857143,-17.6231531176579,
-7.42739908344628));
#15058=CARTESIAN_POINT('Ctrl Pts',(0.457142857142854,-19.3184084901459,
-6.07547803652718));
#15059=CARTESIAN_POINT('Ctrl Pts',(0.671428571428569,-20.259204245073,-4.1218955216168));
#15060=CARTESIAN_POINT('Ctrl Pts',(0.885714285714283,-21.2,-2.16831300670643));
#15061=CARTESIAN_POINT('Ctrl Pts',(1.1,-21.2,-6.93889390390723E-15));
#15062=CARTESIAN_POINT('Ctrl Pts',(1.31428571428571,-21.2,2.16831300670641));
#15063=CARTESIAN_POINT('Ctrl Pts',(1.52857142857143,-20.259204245073,4.1218955216168));
#15064=CARTESIAN_POINT('Ctrl Pts',(1.74285714285714,-19.318408490146,6.07547803652716));
#15065=CARTESIAN_POINT('Ctrl Pts',(1.95714285714286,-17.623153117658,7.42739908344628));
#15066=CARTESIAN_POINT('Ctrl Pts',(2.17142857142857,-15.92789774517,8.77932013036537));
#15067=CARTESIAN_POINT('Ctrl Pts',(2.38571428571428,-13.813948872585,9.26181516572731));
#15068=CARTESIAN_POINT('Ctrl Pts',(2.6,-11.7,9.74431020108925));
#15069=CARTESIAN_POINT('Ctrl Pts',(2.81428571428571,-9.586051127415,9.26181516572731));
#15070=CARTESIAN_POINT('Ctrl Pts',(3.02857142857143,-7.47210225483002,8.77932013036537));
#15071=CARTESIAN_POINT('Ctrl Pts',(3.24285714285714,-5.77684688234203,7.42739908344628));
#15072=CARTESIAN_POINT('Ctrl Pts',(3.45714285714285,-4.08159150985404,6.07547803652717));
#15073=CARTESIAN_POINT('Ctrl Pts',(3.67142857142857,-3.14079575492702,4.1218955216168));
#15074=CARTESIAN_POINT('Ctrl Pts',(3.88571428571428,-2.2,2.16831300670642));
#15075=CARTESIAN_POINT('Ctrl Pts',(4.1,-2.20000000000001,-6.93889390390723E-15));
#15076=CARTESIAN_POINT('Ctrl Pts',(4.31428571428571,-2.19999999999999,-2.16831300670641));
#15077=CARTESIAN_POINT('Ctrl Pts',(4.52857142857143,-3.14079575492703,-4.1218955216168));
#15078=CARTESIAN_POINT('Ctrl Pts',(4.74285714285714,-4.08159150985404,-6.07547803652716));
#15079=CARTESIAN_POINT('Ctrl Pts',(4.95714285714286,-5.77684688234202,-7.42739908344627));
#15080=CARTESIAN_POINT('Ctrl Pts',(5.17142857142857,-7.47210225483002,-8.77932013036537));
#15081=CARTESIAN_POINT('Ctrl Pts',(5.38571428571428,-9.58605112741501,-9.26181516572731));
#15082=CARTESIAN_POINT('Ctrl Pts',(5.6,-11.7,-9.74431020108925));
#15083=CARTESIAN_POINT('Ctrl Pts',(5.81428571428571,-13.813948872585,-9.26181516572731));
#15084=CARTESIAN_POINT('Ctrl Pts',(6.02857142857142,-15.92789774517,-8.77932013036537));
#15085=CARTESIAN_POINT('Ctrl Pts',(6.24285714285714,-17.623153117658,-7.42739908344628));
#15086=CARTESIAN_POINT('Ctrl Pts',(6.45714285714286,-19.3184084901459,-6.07547803652718));
#15087=CARTESIAN_POINT('Ctrl Pts',(6.67142857142857,-20.259204245073,-4.12189552161681));
#15088=CARTESIAN_POINT('Ctrl Pts',(6.88571428571428,-21.2,-2.16831300670643));
#15089=CARTESIAN_POINT('Ctrl Pts',(7.1,-21.2,-1.04083408558608E-14));
#15090=CARTESIAN_POINT('Ctrl Pts',(7.31428571428571,-21.2,2.16831300670641));
#15091=CARTESIAN_POINT('Ctrl Pts',(7.52857142857143,-20.259204245073,4.12189552161679));
#15092=CARTESIAN_POINT('Ctrl Pts',(7.74285714285714,-19.3184084901459,6.07547803652717));
#15093=CARTESIAN_POINT('Ctrl Pts',(7.95714285714285,-17.623153117658,7.42739908344627));
#15094=CARTESIAN_POINT('Ctrl Pts',(8.17142857142857,-15.92789774517,8.77932013036537));
#15095=CARTESIAN_POINT('Ctrl Pts',(8.38571428571429,-13.813948872585,9.26181516572731));
#15096=CARTESIAN_POINT('Ctrl Pts',(8.6,-11.7,9.74431020108926));
#15097=CARTESIAN_POINT('Ctrl Pts',(8.81428571428571,-9.58605112741501,9.26181516572732));
#15098=CARTESIAN_POINT('Ctrl Pts',(9.02857142857143,-7.47210225483001,8.77932013036537));
#15099=CARTESIAN_POINT('Ctrl Pts',(9.24285714285714,-5.77684688234203,7.42739908344627));
#15100=CARTESIAN_POINT('Ctrl Pts',(9.45714285714285,-4.08159150985402,6.07547803652717));
#15101=CARTESIAN_POINT('Ctrl Pts',(9.67142857142857,-3.14079575492703,4.12189552161679));
#15102=CARTESIAN_POINT('Ctrl Pts',(9.88571428571429,-2.20000000000001,2.16831300670642));
#15103=CARTESIAN_POINT('Ctrl Pts',(10.1,-2.19999999999999,0.));
#15104=CARTESIAN_POINT('Ctrl Pts',(10.3142857142857,-2.2,-2.16831300670643));
#15105=CARTESIAN_POINT('Ctrl Pts',(10.5285714285714,-3.14079575492703,-4.12189552161681));
#15106=CARTESIAN_POINT('Ctrl Pts',(10.7428571428571,-4.08159150985404,-6.07547803652718));
#15107=CARTESIAN_POINT('Ctrl Pts',(10.9571428571429,-5.77684688234203,-7.42739908344627));
#15108=CARTESIAN_POINT('Ctrl Pts',(11.1714285714286,-7.47210225483002,-8.77932013036538));
#15109=CARTESIAN_POINT('Ctrl Pts',(11.3857142857143,-9.58605112741501,-9.26181516572732));
#15110=CARTESIAN_POINT('Ctrl Pts',(11.6,-11.7,-9.74431020108924));
#15111=CARTESIAN_POINT('Ctrl Pts',(11.8142857142857,-13.813948872585,-9.26181516572731));
#15112=CARTESIAN_POINT('Ctrl Pts',(12.0285714285714,-15.92789774517,-8.77932013036537));
#15113=CARTESIAN_POINT('Ctrl Pts',(12.2428571428571,-17.623153117658,-7.42739908344628));
#15114=CARTESIAN_POINT('Ctrl Pts',(12.4571428571429,-19.3184084901459,-6.07547803652717));
#15115=CARTESIAN_POINT('Ctrl Pts',(12.6714285714286,-20.259204245073,-4.1218955216168));
#15116=CARTESIAN_POINT('Ctrl Pts',(12.8857142857143,-21.2,-2.16831300670643));
#15117=CARTESIAN_POINT('Ctrl Pts',(13.1,-21.2,-1.04083408558608E-14));
#15118=CARTESIAN_POINT('Ctrl Pts',(13.3142857142857,-21.2,2.16831300670641));
#15119=CARTESIAN_POINT('Ctrl Pts',(13.5285714285714,-20.259204245073,4.12189552161679));
#15120=CARTESIAN_POINT('Ctrl Pts',(13.7428571428571,-19.3184084901459,6.07547803652717));
#15121=CARTESIAN_POINT('Ctrl Pts',(13.9571428571429,-17.623153117658,7.42739908344627));
#15122=CARTESIAN_POINT('Ctrl Pts',(14.1714285714286,-15.92789774517,8.77932013036537));
#15123=CARTESIAN_POINT('Ctrl Pts',(14.3857142857143,-13.813948872585,9.26181516572731));
#15124=CARTESIAN_POINT('Ctrl Pts',(14.6,-11.7,9.74431020108925));
#15125=CARTESIAN_POINT('Ctrl Pts',(14.8142857142857,-9.58605112741501,9.26181516572731));
#15126=CARTESIAN_POINT('Ctrl Pts',(15.0285714285714,-7.47210225483002,8.77932013036537));
#15127=CARTESIAN_POINT('Ctrl Pts',(15.2428571428571,-5.77684688234202,7.42739908344628));
#15128=CARTESIAN_POINT('Ctrl Pts',(15.4571428571429,-4.08159150985404,6.07547803652717));
#15129=CARTESIAN_POINT('Ctrl Pts',(15.6714285714286,-3.14079575492702,4.1218955216168));
#15130=CARTESIAN_POINT('Ctrl Pts',(15.8857142857143,-2.20000000000001,2.16831300670642));
#15131=CARTESIAN_POINT('Ctrl Pts',(16.1,-2.19999999999999,-6.93889390390723E-15));
#15132=CARTESIAN_POINT('Ctrl Pts',(16.3142857142857,-2.19999999999999,-2.16831300670641));
#15133=CARTESIAN_POINT('Ctrl Pts',(16.5285714285714,-3.14079575492702,-4.1218955216168));
#15134=CARTESIAN_POINT('Ctrl Pts',(16.7428571428571,-4.08159150985404,-6.07547803652718));
#15135=CARTESIAN_POINT('Ctrl Pts',(16.9571428571428,-5.77684688234203,-7.42739908344629));
#15136=CARTESIAN_POINT('Ctrl Pts',(17.1714285714286,-7.47210225483002,-8.77932013036539));
#15137=CARTESIAN_POINT('Ctrl Pts',(17.3857142857143,-9.58605112741501,-9.26181516572732));
#15138=CARTESIAN_POINT('Ctrl Pts',(17.6,-11.7,-9.74431020108926));
#15139=CARTESIAN_POINT('Ctrl Pts',(17.8142857142857,-13.813948872585,-9.2618151657273));
#15140=CARTESIAN_POINT('Ctrl Pts',(18.0285714285714,-15.92789774517,-8.77932013036537));
#15141=CARTESIAN_POINT('Ctrl Pts',(18.2428571428571,-17.6231531176579,-7.42739908344628));
#15142=CARTESIAN_POINT('Ctrl Pts',(18.4571428571428,-19.3184084901459,-6.07547803652718));
#15143=CARTESIAN_POINT('Ctrl Pts',(18.6714285714286,-20.259204245073,-4.1218955216168));
#15144=CARTESIAN_POINT('Ctrl Pts',(18.8857142857143,-21.2,-2.16831300670642));
#15145=CARTESIAN_POINT('Ctrl Pts',(19.1,-21.2,0.));
#15146=CARTESIAN_POINT('Ctrl Pts',(19.3142857142857,-21.2,2.16831300670641));
#15147=CARTESIAN_POINT('Ctrl Pts',(19.5285714285714,-20.259204245073,4.12189552161679));
#15148=CARTESIAN_POINT('Ctrl Pts',(19.7428571428572,-19.318408490146,6.07547803652717));
#15149=CARTESIAN_POINT('Ctrl Pts',(19.9571428571429,-17.623153117658,7.42739908344627));
#15150=CARTESIAN_POINT('Ctrl Pts',(20.1714285714286,-15.92789774517,8.77932013036537));
#15151=CARTESIAN_POINT('Ctrl Pts',(20.3857142857143,-13.813948872585,9.26181516572731));
#15152=CARTESIAN_POINT('Ctrl Pts',(20.6,-11.7,9.74431020108925));
#15153=CARTESIAN_POINT('Ctrl Pts',(20.8142857142857,-9.58605112741501,9.2618151657273));
#15154=CARTESIAN_POINT('Ctrl Pts',(21.0285714285714,-7.47210225483003,8.77932013036538));
#15155=CARTESIAN_POINT('Ctrl Pts',(21.2428571428572,-5.77684688234203,7.42739908344627));
#15156=CARTESIAN_POINT('Ctrl Pts',(21.4571428571429,-4.08159150985404,6.07547803652717));
#15157=CARTESIAN_POINT('Ctrl Pts',(21.6714285714286,-3.14079575492702,4.1218955216168));
#15158=CARTESIAN_POINT('Ctrl Pts',(21.8857142857143,-2.2,2.16831300670641));
#15159=CARTESIAN_POINT('Ctrl Pts',(22.1,-2.2,0.));
#15160=CARTESIAN_POINT('',(-0.97049399036428,1.5411253090549,-6.93889390390723E-15));
#15161=CARTESIAN_POINT('',(-1.43524699518214,-0.329437345472555,0.));
#15162=CARTESIAN_POINT('Ctrl Pts',(-0.97049399036428,1.5411253090549,-6.93889390390723E-15));
#15163=CARTESIAN_POINT('Ctrl Pts',(-0.756208276078568,1.5411253090549,-3.02220044537404));
#15164=CARTESIAN_POINT('Ctrl Pts',(-0.541922561792853,0.229841679453259,
-5.74510895921687));
#15165=CARTESIAN_POINT('Ctrl Pts',(-0.327636847507139,-1.08144195014838,
-8.4680174730597));
#15166=CARTESIAN_POINT('Ctrl Pts',(-0.113351133221425,-3.4442934046707,
-10.3523286299233));
#15167=CARTESIAN_POINT('Ctrl Pts',(0.10093458106429,-5.80714485919302,-12.236639786787));
#15168=CARTESIAN_POINT('Ctrl Pts',(0.315220295350005,-8.75357242959651,
-12.9091426524948));
#15169=CARTESIAN_POINT('Ctrl Pts',(0.529506009635718,-11.7,-13.5816455182026));
#15170=CARTESIAN_POINT('Ctrl Pts',(0.743791723921435,-14.6464275704035,
-12.9091426524948));
#15171=CARTESIAN_POINT('Ctrl Pts',(0.958077438207147,-17.592855140807,-12.236639786787));
#15172=CARTESIAN_POINT('Ctrl Pts',(1.17236315249286,-19.9557065953293,-10.3523286299233));
#15173=CARTESIAN_POINT('Ctrl Pts',(1.38664886677857,-22.3185580498516,-8.4680174730597));
#15174=CARTESIAN_POINT('Ctrl Pts',(1.60093458106429,-23.6298416794532,-5.74510895921687));
#15175=CARTESIAN_POINT('Ctrl Pts',(1.81522029535,-24.9411253090549,-3.02220044537404));
#15176=CARTESIAN_POINT('Ctrl Pts',(2.02950600963572,-24.9411253090549,6.93889390390723E-15));
#15177=CARTESIAN_POINT('Ctrl Pts',(2.24379172392143,-24.9411253090549,3.02220044537403));
#15178=CARTESIAN_POINT('Ctrl Pts',(2.45807743820715,-23.6298416794532,5.74510895921686));
#15179=CARTESIAN_POINT('Ctrl Pts',(2.67236315249286,-22.3185580498516,8.4680174730597));
#15180=CARTESIAN_POINT('Ctrl Pts',(2.88664886677858,-19.9557065953293,10.3523286299233));
#15181=CARTESIAN_POINT('Ctrl Pts',(3.10093458106429,-17.592855140807,12.236639786787));
#15182=CARTESIAN_POINT('Ctrl Pts',(3.31522029535001,-14.6464275704035,12.9091426524948));
#15183=CARTESIAN_POINT('Ctrl Pts',(3.52950600963572,-11.7,13.5816455182026));
#15184=CARTESIAN_POINT('Ctrl Pts',(3.74379172392143,-8.7535724295965,12.9091426524948));
#15185=CARTESIAN_POINT('Ctrl Pts',(3.95807743820715,-5.80714485919301,12.236639786787));
#15186=CARTESIAN_POINT('Ctrl Pts',(4.17236315249286,-3.4442934046707,10.3523286299233));
#15187=CARTESIAN_POINT('Ctrl Pts',(4.38664886677858,-1.08144195014837,8.46801747305969));
#15188=CARTESIAN_POINT('Ctrl Pts',(4.60093458106429,0.229841679453252,5.74510895921686));
#15189=CARTESIAN_POINT('Ctrl Pts',(4.81522029535,1.5411253090549,3.02220044537404));
#15190=CARTESIAN_POINT('Ctrl Pts',(5.02950600963572,1.5411253090549,0.));
#15191=CARTESIAN_POINT('Ctrl Pts',(5.24379172392143,1.5411253090549,-3.02220044537404));
#15192=CARTESIAN_POINT('Ctrl Pts',(5.45807743820715,0.229841679453252,-5.74510895921687));
#15193=CARTESIAN_POINT('Ctrl Pts',(5.67236315249286,-1.08144195014837,-8.4680174730597));
#15194=CARTESIAN_POINT('Ctrl Pts',(5.88664886677858,-3.4442934046707,-10.3523286299233));
#15195=CARTESIAN_POINT('Ctrl Pts',(6.10093458106429,-5.80714485919301,-12.236639786787));
#15196=CARTESIAN_POINT('Ctrl Pts',(6.31522029535001,-8.75357242959651,-12.9091426524948));
#15197=CARTESIAN_POINT('Ctrl Pts',(6.52950600963572,-11.7,-13.5816455182026));
#15198=CARTESIAN_POINT('Ctrl Pts',(6.74379172392144,-14.6464275704035,-12.9091426524948));
#15199=CARTESIAN_POINT('Ctrl Pts',(6.95807743820715,-17.592855140807,-12.236639786787));
#15200=CARTESIAN_POINT('Ctrl Pts',(7.17236315249286,-19.9557065953293,-10.3523286299233));
#15201=CARTESIAN_POINT('Ctrl Pts',(7.38664886677858,-22.3185580498516,-8.4680174730597));
#15202=CARTESIAN_POINT('Ctrl Pts',(7.60093458106429,-23.6298416794532,-5.74510895921687));
#15203=CARTESIAN_POINT('Ctrl Pts',(7.81522029535,-24.9411253090549,-3.02220044537404));
#15204=CARTESIAN_POINT('Ctrl Pts',(8.02950600963572,-24.9411253090549,-6.93889390390723E-15));
#15205=CARTESIAN_POINT('Ctrl Pts',(8.24379172392143,-24.9411253090549,3.02220044537402));
#15206=CARTESIAN_POINT('Ctrl Pts',(8.45807743820715,-23.6298416794532,5.74510895921685));
#15207=CARTESIAN_POINT('Ctrl Pts',(8.67236315249286,-22.3185580498516,8.4680174730597));
#15208=CARTESIAN_POINT('Ctrl Pts',(8.88664886677858,-19.9557065953293,10.3523286299233));
#15209=CARTESIAN_POINT('Ctrl Pts',(9.10093458106429,-17.592855140807,12.236639786787));
#15210=CARTESIAN_POINT('Ctrl Pts',(9.31522029535001,-14.6464275704035,12.9091426524948));
#15211=CARTESIAN_POINT('Ctrl Pts',(9.52950600963572,-11.7,13.5816455182026));
#15212=CARTESIAN_POINT('Ctrl Pts',(9.74379172392144,-8.75357242959651,12.9091426524948));
#15213=CARTESIAN_POINT('Ctrl Pts',(9.95807743820714,-5.80714485919302,12.236639786787));
#15214=CARTESIAN_POINT('Ctrl Pts',(10.1723631524929,-3.4442934046707,10.3523286299233));
#15215=CARTESIAN_POINT('Ctrl Pts',(10.3866488667786,-1.08144195014837,8.4680174730597));
#15216=CARTESIAN_POINT('Ctrl Pts',(10.6009345810643,0.229841679453252,5.74510895921686));
#15217=CARTESIAN_POINT('Ctrl Pts',(10.81522029535,1.5411253090549,3.02220044537402));
#15218=CARTESIAN_POINT('Ctrl Pts',(11.0295060096357,1.5411253090549,6.93889390390723E-15));
#15219=CARTESIAN_POINT('Ctrl Pts',(11.2437917239214,1.54112530905489,-3.02220044537404));
#15220=CARTESIAN_POINT('Ctrl Pts',(11.4580774382071,0.229841679453259,-5.74510895921686));
#15221=CARTESIAN_POINT('Ctrl Pts',(11.6723631524929,-1.08144195014837,-8.4680174730597));
#15222=CARTESIAN_POINT('Ctrl Pts',(11.8866488667786,-3.4442934046707,-10.3523286299233));
#15223=CARTESIAN_POINT('Ctrl Pts',(12.1009345810643,-5.80714485919302,-12.236639786787));
#15224=CARTESIAN_POINT('Ctrl Pts',(12.31522029535,-8.75357242959649,-12.9091426524948));
#15225=CARTESIAN_POINT('Ctrl Pts',(12.5295060096357,-11.7,-13.5816455182026));
#15226=CARTESIAN_POINT('Ctrl Pts',(12.7437917239214,-14.6464275704035,-12.9091426524948));
#15227=CARTESIAN_POINT('Ctrl Pts',(12.9580774382072,-17.592855140807,-12.236639786787));
#15228=CARTESIAN_POINT('Ctrl Pts',(13.1723631524929,-19.9557065953293,-10.3523286299233));
#15229=CARTESIAN_POINT('Ctrl Pts',(13.3866488667786,-22.3185580498516,-8.4680174730597));
#15230=CARTESIAN_POINT('Ctrl Pts',(13.6009345810643,-23.6298416794532,-5.74510895921687));
#15231=CARTESIAN_POINT('Ctrl Pts',(13.81522029535,-24.9411253090549,-3.02220044537403));
#15232=CARTESIAN_POINT('Ctrl Pts',(14.0295060096357,-24.9411253090549,-6.93889390390723E-15));
#15233=CARTESIAN_POINT('Ctrl Pts',(14.2437917239214,-24.9411253090549,3.02220044537403));
#15234=CARTESIAN_POINT('Ctrl Pts',(14.4580774382072,-23.6298416794532,5.74510895921685));
#15235=CARTESIAN_POINT('Ctrl Pts',(14.6723631524929,-22.3185580498516,8.46801747305969));
#15236=CARTESIAN_POINT('Ctrl Pts',(14.8866488667786,-19.9557065953293,10.3523286299233));
#15237=CARTESIAN_POINT('Ctrl Pts',(15.1009345810643,-17.592855140807,12.236639786787));
#15238=CARTESIAN_POINT('Ctrl Pts',(15.31522029535,-14.6464275704035,12.9091426524948));
#15239=CARTESIAN_POINT('Ctrl Pts',(15.5295060096357,-11.7,13.5816455182026));
#15240=CARTESIAN_POINT('Ctrl Pts',(15.7437917239214,-8.75357242959651,12.9091426524948));
#15241=CARTESIAN_POINT('Ctrl Pts',(15.9580774382071,-5.80714485919302,12.236639786787));
#15242=CARTESIAN_POINT('Ctrl Pts',(16.1723631524929,-3.4442934046707,10.3523286299233));
#15243=CARTESIAN_POINT('Ctrl Pts',(16.3866488667786,-1.08144195014837,8.46801747305969));
#15244=CARTESIAN_POINT('Ctrl Pts',(16.6009345810643,0.229841679453266,5.74510895921686));
#15245=CARTESIAN_POINT('Ctrl Pts',(16.81522029535,1.5411253090549,3.02220044537404));
#15246=CARTESIAN_POINT('Ctrl Pts',(17.0295060096357,1.5411253090549,-2.08166817117217E-14));
#15247=CARTESIAN_POINT('Ctrl Pts',(17.2437917239214,1.5411253090549,-3.02220044537405));
#15248=CARTESIAN_POINT('Ctrl Pts',(17.4580774382072,0.229841679453266,-5.74510895921688));
#15249=CARTESIAN_POINT('Ctrl Pts',(17.6723631524929,-1.08144195014837,-8.46801747305971));
#15250=CARTESIAN_POINT('Ctrl Pts',(17.8866488667786,-3.44429340467071,-10.3523286299233));
#15251=CARTESIAN_POINT('Ctrl Pts',(18.1009345810643,-5.80714485919302,-12.236639786787));
#15252=CARTESIAN_POINT('Ctrl Pts',(18.31522029535,-8.75357242959651,-12.9091426524948));
#15253=CARTESIAN_POINT('Ctrl Pts',(18.5295060096357,-11.7,-13.5816455182026));
#15254=CARTESIAN_POINT('Ctrl Pts',(18.7437917239214,-14.6464275704035,-12.9091426524948));
#15255=CARTESIAN_POINT('Ctrl Pts',(18.9580774382071,-17.592855140807,-12.236639786787));
#15256=CARTESIAN_POINT('Ctrl Pts',(19.1723631524929,-19.9557065953293,-10.3523286299233));
#15257=CARTESIAN_POINT('Ctrl Pts',(19.3866488667786,-22.3185580498516,-8.4680174730597));
#15258=CARTESIAN_POINT('Ctrl Pts',(19.6009345810643,-23.6298416794532,-5.74510895921687));
#15259=CARTESIAN_POINT('Ctrl Pts',(19.81522029535,-24.9411253090549,-3.02220044537404));
#15260=CARTESIAN_POINT('Ctrl Pts',(20.0295060096357,-24.9411253090549,0.));
#15261=CARTESIAN_POINT('Ctrl Pts',(20.2437917239214,-24.9411253090549,3.02220044537403));
#15262=CARTESIAN_POINT('Ctrl Pts',(20.4580774382071,-23.6298416794532,5.74510895921685));
#15263=CARTESIAN_POINT('Ctrl Pts',(20.6723631524929,-22.3185580498516,8.46801747305969));
#15264=CARTESIAN_POINT('Ctrl Pts',(20.8866488667786,-19.9557065953293,10.3523286299233));
#15265=CARTESIAN_POINT('Ctrl Pts',(21.1009345810643,-17.5928551408069,12.236639786787));
#15266=CARTESIAN_POINT('Ctrl Pts',(21.31522029535,-14.6464275704035,12.9091426524948));
#15267=CARTESIAN_POINT('Ctrl Pts',(21.5295060096357,-11.7,13.5816455182026));
#15268=CARTESIAN_POINT('Ctrl Pts',(21.7437917239214,-8.75357242959651,12.9091426524948));
#15269=CARTESIAN_POINT('Ctrl Pts',(21.9580774382071,-5.80714485919301,12.236639786787));
#15270=CARTESIAN_POINT('Ctrl Pts',(22.1723631524929,-3.4442934046707,10.3523286299233));
#15271=CARTESIAN_POINT('Ctrl Pts',(22.3866488667786,-1.08144195014837,8.4680174730597));
#15272=CARTESIAN_POINT('Ctrl Pts',(22.6009345810643,0.229841679453259,5.74510895921686));
#15273=CARTESIAN_POINT('Ctrl Pts',(22.81522029535,1.54112530905491,3.02220044537404));
#15274=CARTESIAN_POINT('Ctrl Pts',(23.0295060096357,1.5411253090549,0.));
#15275=CARTESIAN_POINT('Ctrl Pts',(0.970493990364278,1.5411253090549,-1.38777878078145E-14));
#15276=CARTESIAN_POINT('Ctrl Pts',(1.18477970464999,1.54112530905491,-3.02220044537403));
#15277=CARTESIAN_POINT('Ctrl Pts',(1.39906541893571,0.229841679453259,-5.74510895921686));
#15278=CARTESIAN_POINT('Ctrl Pts',(1.61335113322142,-1.08144195014838,-8.4680174730597));
#15279=CARTESIAN_POINT('Ctrl Pts',(1.82763684750713,-3.44429340467071,-10.3523286299233));
#15280=CARTESIAN_POINT('Ctrl Pts',(2.04192256179285,-5.80714485919301,-12.236639786787));
#15281=CARTESIAN_POINT('Ctrl Pts',(2.25620827607856,-8.75357242959651,-12.9091426524948));
#15282=CARTESIAN_POINT('Ctrl Pts',(2.47049399036428,-11.7,-13.5816455182026));
#15283=CARTESIAN_POINT('Ctrl Pts',(2.68477970464999,-14.6464275704035,-12.9091426524948));
#15284=CARTESIAN_POINT('Ctrl Pts',(2.89906541893571,-17.592855140807,-12.236639786787));
#15285=CARTESIAN_POINT('Ctrl Pts',(3.11335113322142,-19.9557065953293,-10.3523286299233));
#15286=CARTESIAN_POINT('Ctrl Pts',(3.32763684750713,-22.3185580498516,-8.4680174730597));
#15287=CARTESIAN_POINT('Ctrl Pts',(3.54192256179285,-23.6298416794532,-5.74510895921686));
#15288=CARTESIAN_POINT('Ctrl Pts',(3.75620827607856,-24.9411253090549,-3.02220044537403));
#15289=CARTESIAN_POINT('Ctrl Pts',(3.97049399036428,-24.9411253090549,3.46944695195361E-15));
#15290=CARTESIAN_POINT('Ctrl Pts',(4.18477970464999,-24.9411253090549,3.02220044537403));
#15291=CARTESIAN_POINT('Ctrl Pts',(4.39906541893571,-23.6298416794532,5.74510895921686));
#15292=CARTESIAN_POINT('Ctrl Pts',(4.61335113322142,-22.3185580498516,8.46801747305969));
#15293=CARTESIAN_POINT('Ctrl Pts',(4.82763684750714,-19.9557065953293,10.3523286299233));
#15294=CARTESIAN_POINT('Ctrl Pts',(5.04192256179285,-17.592855140807,12.2366397867869));
#15295=CARTESIAN_POINT('Ctrl Pts',(5.25620827607856,-14.6464275704035,12.9091426524948));
#15296=CARTESIAN_POINT('Ctrl Pts',(5.47049399036428,-11.7,13.5816455182026));
#15297=CARTESIAN_POINT('Ctrl Pts',(5.68477970464999,-8.75357242959651,12.9091426524948));
#15298=CARTESIAN_POINT('Ctrl Pts',(5.89906541893571,-5.80714485919302,12.236639786787));
#15299=CARTESIAN_POINT('Ctrl Pts',(6.11335113322142,-3.4442934046707,10.3523286299233));
#15300=CARTESIAN_POINT('Ctrl Pts',(6.32763684750713,-1.08144195014838,8.4680174730597));
#15301=CARTESIAN_POINT('Ctrl Pts',(6.54192256179285,0.229841679453252,5.74510895921686));
#15302=CARTESIAN_POINT('Ctrl Pts',(6.75620827607856,1.5411253090549,3.02220044537404));
#15303=CARTESIAN_POINT('Ctrl Pts',(6.97049399036428,1.5411253090549,-1.38777878078145E-14));
#15304=CARTESIAN_POINT('Ctrl Pts',(7.18477970464999,1.5411253090549,-3.02220044537404));
#15305=CARTESIAN_POINT('Ctrl Pts',(7.39906541893571,0.229841679453259,-5.74510895921689));
#15306=CARTESIAN_POINT('Ctrl Pts',(7.61335113322142,-1.08144195014838,-8.46801747305971));
#15307=CARTESIAN_POINT('Ctrl Pts',(7.82763684750713,-3.4442934046707,-10.3523286299233));
#15308=CARTESIAN_POINT('Ctrl Pts',(8.04192256179285,-5.80714485919302,-12.236639786787));
#15309=CARTESIAN_POINT('Ctrl Pts',(8.25620827607856,-8.75357242959651,-12.9091426524948));
#15310=CARTESIAN_POINT('Ctrl Pts',(8.47049399036428,-11.7,-13.5816455182026));
#15311=CARTESIAN_POINT('Ctrl Pts',(8.68477970464999,-14.6464275704035,-12.9091426524948));
#15312=CARTESIAN_POINT('Ctrl Pts',(8.89906541893571,-17.592855140807,-12.236639786787));
#15313=CARTESIAN_POINT('Ctrl Pts',(9.11335113322142,-19.9557065953293,-10.3523286299233));
#15314=CARTESIAN_POINT('Ctrl Pts',(9.32763684750714,-22.3185580498516,-8.4680174730597));
#15315=CARTESIAN_POINT('Ctrl Pts',(9.54192256179285,-23.6298416794532,-5.74510895921687));
#15316=CARTESIAN_POINT('Ctrl Pts',(9.75620827607856,-24.9411253090549,-3.02220044537404));
#15317=CARTESIAN_POINT('Ctrl Pts',(9.97049399036428,-24.9411253090549,-6.93889390390723E-15));
#15318=CARTESIAN_POINT('Ctrl Pts',(10.18477970465,-24.9411253090549,3.02220044537403));
#15319=CARTESIAN_POINT('Ctrl Pts',(10.3990654189357,-23.6298416794532,5.74510895921686));
#15320=CARTESIAN_POINT('Ctrl Pts',(10.6133511332214,-22.3185580498516,8.4680174730597));
#15321=CARTESIAN_POINT('Ctrl Pts',(10.8276368475071,-19.9557065953293,10.3523286299233));
#15322=CARTESIAN_POINT('Ctrl Pts',(11.0419225617928,-17.592855140807,12.236639786787));
#15323=CARTESIAN_POINT('Ctrl Pts',(11.2562082760786,-14.6464275704035,12.9091426524948));
#15324=CARTESIAN_POINT('Ctrl Pts',(11.4704939903643,-11.7,13.5816455182026));
#15325=CARTESIAN_POINT('Ctrl Pts',(11.68477970465,-8.75357242959651,12.9091426524948));
#15326=CARTESIAN_POINT('Ctrl Pts',(11.8990654189357,-5.80714485919301,12.236639786787));
#15327=CARTESIAN_POINT('Ctrl Pts',(12.1133511332214,-3.4442934046707,10.3523286299233));
#15328=CARTESIAN_POINT('Ctrl Pts',(12.3276368475071,-1.08144195014836,8.4680174730597));
#15329=CARTESIAN_POINT('Ctrl Pts',(12.5419225617929,0.229841679453266,5.74510895921686));
#15330=CARTESIAN_POINT('Ctrl Pts',(12.7562082760786,1.5411253090549,3.02220044537403));
#15331=CARTESIAN_POINT('Ctrl Pts',(12.9704939903643,1.5411253090549,-2.08166817117217E-14));
#15332=CARTESIAN_POINT('Ctrl Pts',(13.18477970465,1.5411253090549,-3.02220044537405));
#15333=CARTESIAN_POINT('Ctrl Pts',(13.3990654189357,0.229841679453252,-5.74510895921687));
#15334=CARTESIAN_POINT('Ctrl Pts',(13.6133511332214,-1.08144195014838,-8.46801747305971));
#15335=CARTESIAN_POINT('Ctrl Pts',(13.8276368475071,-3.44429340467069,-10.3523286299233));
#15336=CARTESIAN_POINT('Ctrl Pts',(14.0419225617929,-5.80714485919301,-12.236639786787));
#15337=CARTESIAN_POINT('Ctrl Pts',(14.2562082760786,-8.75357242959651,-12.9091426524948));
#15338=CARTESIAN_POINT('Ctrl Pts',(14.4704939903643,-11.7,-13.5816455182026));
#15339=CARTESIAN_POINT('Ctrl Pts',(14.68477970465,-14.6464275704035,-12.9091426524948));
#15340=CARTESIAN_POINT('Ctrl Pts',(14.8990654189357,-17.592855140807,-12.236639786787));
#15341=CARTESIAN_POINT('Ctrl Pts',(15.1133511332214,-19.9557065953293,-10.3523286299233));
#15342=CARTESIAN_POINT('Ctrl Pts',(15.3276368475071,-22.3185580498516,-8.46801747305969));
#15343=CARTESIAN_POINT('Ctrl Pts',(15.5419225617929,-23.6298416794532,-5.74510895921687));
#15344=CARTESIAN_POINT('Ctrl Pts',(15.7562082760786,-24.9411253090549,-3.02220044537403));
#15345=CARTESIAN_POINT('Ctrl Pts',(15.9704939903643,-24.9411253090549,-6.93889390390723E-15));
#15346=CARTESIAN_POINT('Ctrl Pts',(16.18477970465,-24.9411253090549,3.02220044537403));
#15347=CARTESIAN_POINT('Ctrl Pts',(16.3990654189357,-23.6298416794532,5.74510895921686));
#15348=CARTESIAN_POINT('Ctrl Pts',(16.6133511332214,-22.3185580498516,8.46801747305969));
#15349=CARTESIAN_POINT('Ctrl Pts',(16.8276368475071,-19.9557065953293,10.3523286299233));
#15350=CARTESIAN_POINT('Ctrl Pts',(17.0419225617928,-17.592855140807,12.236639786787));
#15351=CARTESIAN_POINT('Ctrl Pts',(17.2562082760786,-14.6464275704035,12.9091426524948));
#15352=CARTESIAN_POINT('Ctrl Pts',(17.4704939903643,-11.7,13.5816455182026));
#15353=CARTESIAN_POINT('Ctrl Pts',(17.68477970465,-8.75357242959651,12.9091426524948));
#15354=CARTESIAN_POINT('Ctrl Pts',(17.8990654189357,-5.80714485919301,12.236639786787));
#15355=CARTESIAN_POINT('Ctrl Pts',(18.1133511332214,-3.4442934046707,10.3523286299233));
#15356=CARTESIAN_POINT('Ctrl Pts',(18.3276368475071,-1.08144195014837,8.46801747305969));
#15357=CARTESIAN_POINT('Ctrl Pts',(18.5419225617928,0.229841679453252,5.74510895921686));
#15358=CARTESIAN_POINT('Ctrl Pts',(18.7562082760786,1.5411253090549,3.02220044537405));
#15359=CARTESIAN_POINT('Ctrl Pts',(18.9704939903643,1.5411253090549,-1.38777878078145E-14));
#15360=CARTESIAN_POINT('Ctrl Pts',(19.18477970465,1.5411253090549,-3.02220044537404));
#15361=CARTESIAN_POINT('Ctrl Pts',(19.3990654189357,0.229841679453259,-5.74510895921686));
#15362=CARTESIAN_POINT('Ctrl Pts',(19.6133511332214,-1.08144195014838,-8.4680174730597));
#15363=CARTESIAN_POINT('Ctrl Pts',(19.8276368475071,-3.4442934046707,-10.3523286299233));
#15364=CARTESIAN_POINT('Ctrl Pts',(20.0419225617929,-5.80714485919302,-12.236639786787));
#15365=CARTESIAN_POINT('Ctrl Pts',(20.2562082760786,-8.75357242959651,-12.9091426524948));
#15366=CARTESIAN_POINT('Ctrl Pts',(20.4704939903643,-11.7,-13.5816455182026));
#15367=CARTESIAN_POINT('Ctrl Pts',(20.68477970465,-14.6464275704035,-12.9091426524948));
#15368=CARTESIAN_POINT('Ctrl Pts',(20.8990654189357,-17.592855140807,-12.236639786787));
#15369=CARTESIAN_POINT('Ctrl Pts',(21.1133511332214,-19.9557065953293,-10.3523286299233));
#15370=CARTESIAN_POINT('Ctrl Pts',(21.3276368475071,-22.3185580498516,-8.4680174730597));
#15371=CARTESIAN_POINT('Ctrl Pts',(21.5419225617929,-23.6298416794532,-5.74510895921687));
#15372=CARTESIAN_POINT('Ctrl Pts',(21.7562082760786,-24.9411253090549,-3.02220044537404));
#15373=CARTESIAN_POINT('Ctrl Pts',(21.9704939903643,-24.9411253090549,-3.46944695195361E-15));
#15374=CARTESIAN_POINT('Ctrl Pts',(22.18477970465,-24.9411253090549,3.02220044537403));
#15375=CARTESIAN_POINT('Ctrl Pts',(22.3990654189357,-23.6298416794532,5.74510895921686));
#15376=CARTESIAN_POINT('Ctrl Pts',(22.6133511332214,-22.3185580498516,8.46801747305969));
#15377=CARTESIAN_POINT('Ctrl Pts',(22.8276368475071,-19.9557065953293,10.3523286299233));
#15378=CARTESIAN_POINT('Ctrl Pts',(23.0419225617928,-17.592855140807,12.236639786787));
#15379=CARTESIAN_POINT('Ctrl Pts',(23.2562082760786,-14.6464275704035,12.9091426524948));
#15380=CARTESIAN_POINT('Ctrl Pts',(23.4704939903643,-11.7,13.5816455182026));
#15381=CARTESIAN_POINT('Ctrl Pts',(23.68477970465,-8.75357242959651,12.9091426524948));
#15382=CARTESIAN_POINT('Ctrl Pts',(23.8990654189357,-5.80714485919302,12.236639786787));
#15383=CARTESIAN_POINT('Ctrl Pts',(24.1133511332214,-3.4442934046707,10.3523286299233));
#15384=CARTESIAN_POINT('Ctrl Pts',(24.3276368475071,-1.08144195014837,8.46801747305969));
#15385=CARTESIAN_POINT('Ctrl Pts',(24.5419225617928,0.229841679453252,5.74510895921686));
#15386=CARTESIAN_POINT('Ctrl Pts',(24.7562082760786,1.5411253090549,3.02220044537404));
#15387=CARTESIAN_POINT('Ctrl Pts',(24.9704939903643,1.5411253090549,0.));
#15388=CARTESIAN_POINT('Ctrl Pts',(0.654743522119005,2.81197461594778,-1.40439689870177E-14));
#15389=CARTESIAN_POINT('Ctrl Pts',(0.869029236404722,2.81197461594777,-3.31226350660561));
#15390=CARTESIAN_POINT('Ctrl Pts',(1.08331495069043,1.37483734075911,-6.2965098083465));
#15391=CARTESIAN_POINT('Ctrl Pts',(1.29760066497615,-0.0622999344295592,
-9.28075611008744));
#15392=CARTESIAN_POINT('Ctrl Pts',(1.51188637926186,-2.65193182212374,-11.3459186275249));
#15393=CARTESIAN_POINT('Ctrl Pts',(1.72617209354758,-5.24156370981795,-13.4110811449623));
#15394=CARTESIAN_POINT('Ctrl Pts',(1.94045780783329,-8.47078185490896,-14.1481291139616));
#15395=CARTESIAN_POINT('Ctrl Pts',(2.15474352211901,-11.7,-14.8851770829609));
#15396=CARTESIAN_POINT('Ctrl Pts',(2.36902923640472,-14.929218145091,-14.1481291139616));
#15397=CARTESIAN_POINT('Ctrl Pts',(2.58331495069044,-18.158436290182,-13.4110811449623));
#15398=CARTESIAN_POINT('Ctrl Pts',(2.79760066497615,-20.7480681778762,-11.3459186275249));
#15399=CARTESIAN_POINT('Ctrl Pts',(3.01188637926186,-23.3377000655704,-9.28075611008745));
#15400=CARTESIAN_POINT('Ctrl Pts',(3.22617209354758,-24.7748373407591,-6.29650980834652));
#15401=CARTESIAN_POINT('Ctrl Pts',(3.44045780783329,-26.2119746159478,-3.31226350660559));
#15402=CARTESIAN_POINT('Ctrl Pts',(3.65474352211901,-26.2119746159477,0.));
#15403=CARTESIAN_POINT('Ctrl Pts',(3.86902923640472,-26.2119746159478,3.31226350660556));
#15404=CARTESIAN_POINT('Ctrl Pts',(4.08331495069043,-24.7748373407591,6.2965098083465));
#15405=CARTESIAN_POINT('Ctrl Pts',(4.29760066497615,-23.3377000655704,9.28075611008741));
#15406=CARTESIAN_POINT('Ctrl Pts',(4.51188637926187,-20.7480681778762,11.3459186275248));
#15407=CARTESIAN_POINT('Ctrl Pts',(4.72617209354758,-18.158436290182,13.4110811449623));
#15408=CARTESIAN_POINT('Ctrl Pts',(4.94045780783329,-14.929218145091,14.1481291139616));
#15409=CARTESIAN_POINT('Ctrl Pts',(5.15474352211901,-11.7,14.8851770829609));
#15410=CARTESIAN_POINT('Ctrl Pts',(5.36902923640472,-8.47078185490897,14.1481291139616));
#15411=CARTESIAN_POINT('Ctrl Pts',(5.58331495069043,-5.24156370981795,13.4110811449623));
#15412=CARTESIAN_POINT('Ctrl Pts',(5.79760066497615,-2.65193182212374,11.3459186275248));
#15413=CARTESIAN_POINT('Ctrl Pts',(6.01188637926187,-0.0622999344295592,
9.28075611008741));
#15414=CARTESIAN_POINT('Ctrl Pts',(6.22617209354758,1.3748373407591,6.2965098083465));
#15415=CARTESIAN_POINT('Ctrl Pts',(6.44045780783329,2.81197461594777,3.31226350660556));
#15416=CARTESIAN_POINT('Ctrl Pts',(6.65474352211901,2.81197461594778,-2.10659534805265E-14));
#15417=CARTESIAN_POINT('Ctrl Pts',(6.86902923640472,2.81197461594777,-3.31226350660559));
#15418=CARTESIAN_POINT('Ctrl Pts',(7.08331495069044,1.37483734075912,-6.29650980834652));
#15419=CARTESIAN_POINT('Ctrl Pts',(7.29760066497615,-0.0622999344295448,
-9.28075611008746));
#15420=CARTESIAN_POINT('Ctrl Pts',(7.51188637926187,-2.65193182212374,-11.3459186275249));
#15421=CARTESIAN_POINT('Ctrl Pts',(7.72617209354758,-5.24156370981795,-13.4110811449623));
#15422=CARTESIAN_POINT('Ctrl Pts',(7.9404578078333,-8.47078185490895,-14.1481291139616));
#15423=CARTESIAN_POINT('Ctrl Pts',(8.15474352211901,-11.7,-14.8851770829609));
#15424=CARTESIAN_POINT('Ctrl Pts',(8.36902923640472,-14.929218145091,-14.1481291139616));
#15425=CARTESIAN_POINT('Ctrl Pts',(8.58331495069044,-18.158436290182,-13.4110811449623));
#15426=CARTESIAN_POINT('Ctrl Pts',(8.79760066497615,-20.7480681778762,-11.3459186275249));
#15427=CARTESIAN_POINT('Ctrl Pts',(9.01188637926186,-23.3377000655704,-9.28075611008744));
#15428=CARTESIAN_POINT('Ctrl Pts',(9.22617209354758,-24.7748373407591,-6.29650980834652));
#15429=CARTESIAN_POINT('Ctrl Pts',(9.44045780783329,-26.2119746159478,-3.3122635066056));
#15430=CARTESIAN_POINT('Ctrl Pts',(9.65474352211901,-26.2119746159477,-1.40439689870177E-14));
#15431=CARTESIAN_POINT('Ctrl Pts',(9.86902923640472,-26.2119746159478,3.31226350660556));
#15432=CARTESIAN_POINT('Ctrl Pts',(10.0833149506904,-24.7748373407591,6.29650980834649));
#15433=CARTESIAN_POINT('Ctrl Pts',(10.2976006649762,-23.3377000655704,9.28075611008742));
#15434=CARTESIAN_POINT('Ctrl Pts',(10.5118863792619,-20.7480681778762,11.3459186275248));
#15435=CARTESIAN_POINT('Ctrl Pts',(10.7261720935476,-18.158436290182,13.4110811449623));
#15436=CARTESIAN_POINT('Ctrl Pts',(10.9404578078333,-14.929218145091,14.1481291139616));
#15437=CARTESIAN_POINT('Ctrl Pts',(11.154743522119,-11.7,14.8851770829608));
#15438=CARTESIAN_POINT('Ctrl Pts',(11.3690292364047,-8.47078185490896,14.1481291139616));
#15439=CARTESIAN_POINT('Ctrl Pts',(11.5833149506904,-5.24156370981795,13.4110811449623));
#15440=CARTESIAN_POINT('Ctrl Pts',(11.7976006649762,-2.65193182212374,11.3459186275248));
#15441=CARTESIAN_POINT('Ctrl Pts',(12.0118863792619,-0.0622999344295592,
9.28075611008742));
#15442=CARTESIAN_POINT('Ctrl Pts',(12.2261720935476,1.3748373407591,6.29650980834649));
#15443=CARTESIAN_POINT('Ctrl Pts',(12.4404578078333,2.81197461594777,3.31226350660557));
#15444=CARTESIAN_POINT('Ctrl Pts',(12.654743522119,2.81197461594777,0.));
#15445=CARTESIAN_POINT('Ctrl Pts',(12.8690292364047,2.81197461594777,-3.31226350660558));
#15446=CARTESIAN_POINT('Ctrl Pts',(13.0833149506904,1.37483734075912,-6.29650980834652));
#15447=CARTESIAN_POINT('Ctrl Pts',(13.2976006649762,-0.0622999344295448,
-9.28075611008746));
#15448=CARTESIAN_POINT('Ctrl Pts',(13.5118863792619,-2.65193182212374,-11.3459186275249));
#15449=CARTESIAN_POINT('Ctrl Pts',(13.7261720935476,-5.24156370981795,-13.4110811449623));
#15450=CARTESIAN_POINT('Ctrl Pts',(13.9404578078333,-8.47078185490895,-14.1481291139616));
#15451=CARTESIAN_POINT('Ctrl Pts',(14.154743522119,-11.7,-14.8851770829609));
#15452=CARTESIAN_POINT('Ctrl Pts',(14.3690292364047,-14.929218145091,-14.1481291139616));
#15453=CARTESIAN_POINT('Ctrl Pts',(14.5833149506904,-18.158436290182,-13.4110811449623));
#15454=CARTESIAN_POINT('Ctrl Pts',(14.7976006649761,-20.7480681778762,-11.3459186275249));
#15455=CARTESIAN_POINT('Ctrl Pts',(15.0118863792619,-23.3377000655704,-9.28075611008744));
#15456=CARTESIAN_POINT('Ctrl Pts',(15.2261720935476,-24.7748373407591,-6.29650980834651));
#15457=CARTESIAN_POINT('Ctrl Pts',(15.4404578078333,-26.2119746159478,-3.31226350660559));
#15458=CARTESIAN_POINT('Ctrl Pts',(15.654743522119,-26.2119746159478,-1.40439689870177E-14));
#15459=CARTESIAN_POINT('Ctrl Pts',(15.8690292364047,-26.2119746159478,3.31226350660556));
#15460=CARTESIAN_POINT('Ctrl Pts',(16.0833149506904,-24.7748373407591,6.29650980834649));
#15461=CARTESIAN_POINT('Ctrl Pts',(16.2976006649761,-23.3377000655704,9.28075611008742));
#15462=CARTESIAN_POINT('Ctrl Pts',(16.5118863792619,-20.7480681778762,11.3459186275248));
#15463=CARTESIAN_POINT('Ctrl Pts',(16.7261720935476,-18.158436290182,13.4110811449623));
#15464=CARTESIAN_POINT('Ctrl Pts',(16.9404578078333,-14.929218145091,14.1481291139616));
#15465=CARTESIAN_POINT('Ctrl Pts',(17.154743522119,-11.7,14.8851770829609));
#15466=CARTESIAN_POINT('Ctrl Pts',(17.3690292364047,-8.47078185490896,14.1481291139616));
#15467=CARTESIAN_POINT('Ctrl Pts',(17.5833149506904,-5.24156370981795,13.4110811449623));
#15468=CARTESIAN_POINT('Ctrl Pts',(17.7976006649762,-2.65193182212374,11.3459186275248));
#15469=CARTESIAN_POINT('Ctrl Pts',(18.0118863792619,-0.0622999344295592,
9.28075611008742));
#15470=CARTESIAN_POINT('Ctrl Pts',(18.2261720935476,1.37483734075912,6.29650980834649));
#15471=CARTESIAN_POINT('Ctrl Pts',(18.4404578078333,2.81197461594777,3.31226350660556));
#15472=CARTESIAN_POINT('Ctrl Pts',(18.654743522119,2.81197461594778,0.));
#15473=CARTESIAN_POINT('Ctrl Pts',(18.8690292364047,2.81197461594775,-3.31226350660559));
#15474=CARTESIAN_POINT('Ctrl Pts',(19.0833149506904,1.37483734075912,-6.29650980834651));
#15475=CARTESIAN_POINT('Ctrl Pts',(19.2976006649762,-0.0622999344295592,
-9.28075611008743));
#15476=CARTESIAN_POINT('Ctrl Pts',(19.5118863792619,-2.65193182212375,-11.3459186275249));
#15477=CARTESIAN_POINT('Ctrl Pts',(19.7261720935476,-5.24156370981795,-13.4110811449623));
#15478=CARTESIAN_POINT('Ctrl Pts',(19.9404578078333,-8.47078185490895,-14.1481291139616));
#15479=CARTESIAN_POINT('Ctrl Pts',(20.154743522119,-11.7,-14.8851770829609));
#15480=CARTESIAN_POINT('Ctrl Pts',(20.3690292364047,-14.929218145091,-14.1481291139616));
#15481=CARTESIAN_POINT('Ctrl Pts',(20.5833149506904,-18.158436290182,-13.4110811449623));
#15482=CARTESIAN_POINT('Ctrl Pts',(20.7976006649762,-20.7480681778762,-11.3459186275249));
#15483=CARTESIAN_POINT('Ctrl Pts',(21.0118863792619,-23.3377000655704,-9.28075611008745));
#15484=CARTESIAN_POINT('Ctrl Pts',(21.2261720935476,-24.7748373407591,-6.29650980834651));
#15485=CARTESIAN_POINT('Ctrl Pts',(21.4404578078333,-26.2119746159478,-3.3122635066056));
#15486=CARTESIAN_POINT('Ctrl Pts',(21.654743522119,-26.2119746159478,-1.75549612337721E-14));
#15487=CARTESIAN_POINT('Ctrl Pts',(21.8690292364047,-26.2119746159478,3.31226350660556));
#15488=CARTESIAN_POINT('Ctrl Pts',(22.0833149506904,-24.7748373407591,6.2965098083465));
#15489=CARTESIAN_POINT('Ctrl Pts',(22.2976006649761,-23.3377000655704,9.28075611008742));
#15490=CARTESIAN_POINT('Ctrl Pts',(22.5118863792619,-20.7480681778762,11.3459186275248));
#15491=CARTESIAN_POINT('Ctrl Pts',(22.7261720935476,-18.158436290182,13.4110811449623));
#15492=CARTESIAN_POINT('Ctrl Pts',(22.9404578078333,-14.929218145091,14.1481291139616));
#15493=CARTESIAN_POINT('Ctrl Pts',(23.154743522119,-11.7,14.8851770829608));
#15494=CARTESIAN_POINT('Ctrl Pts',(23.3690292364047,-8.47078185490898,14.1481291139616));
#15495=CARTESIAN_POINT('Ctrl Pts',(23.5833149506904,-5.24156370981795,13.4110811449623));
#15496=CARTESIAN_POINT('Ctrl Pts',(23.7976006649762,-2.65193182212374,11.3459186275248));
#15497=CARTESIAN_POINT('Ctrl Pts',(24.0118863792619,-0.0622999344295592,
9.28075611008742));
#15498=CARTESIAN_POINT('Ctrl Pts',(24.2261720935476,1.37483734075911,6.29650980834651));
#15499=CARTESIAN_POINT('Ctrl Pts',(24.4404578078333,2.81197461594777,3.31226350660555));
#15500=CARTESIAN_POINT('Ctrl Pts',(24.654743522119,2.81197461594778,-7.02198449350884E-15));
#15501=CARTESIAN_POINT('Ctrl Pts',(-0.65474352211901,2.81197461594778,-2.10659534805265E-14));
#15502=CARTESIAN_POINT('Ctrl Pts',(-0.440457807833293,2.81197461594777,
-3.31226350660559));
#15503=CARTESIAN_POINT('Ctrl Pts',(-0.226172093547581,1.37483734075912,
-6.29650980834653));
#15504=CARTESIAN_POINT('Ctrl Pts',(-0.0118863792618643,-0.0622999344295592,
-9.28075611008746));
#15505=CARTESIAN_POINT('Ctrl Pts',(0.202399335023847,-2.65193182212374,
-11.3459186275249));
#15506=CARTESIAN_POINT('Ctrl Pts',(0.416685049309566,-5.24156370981794,
-13.4110811449623));
#15507=CARTESIAN_POINT('Ctrl Pts',(0.630970763595276,-8.47078185490896,
-14.1481291139616));
#15508=CARTESIAN_POINT('Ctrl Pts',(0.845256477880995,-11.7,-14.8851770829609));
#15509=CARTESIAN_POINT('Ctrl Pts',(1.05954219216671,-14.929218145091,-14.1481291139616));
#15510=CARTESIAN_POINT('Ctrl Pts',(1.27382790645242,-18.158436290182,-13.4110811449623));
#15511=CARTESIAN_POINT('Ctrl Pts',(1.48811362073813,-20.7480681778762,-11.3459186275249));
#15512=CARTESIAN_POINT('Ctrl Pts',(1.70239933502385,-23.3377000655704,-9.28075611008745));
#15513=CARTESIAN_POINT('Ctrl Pts',(1.91668504930956,-24.7748373407591,-6.29650980834651));
#15514=CARTESIAN_POINT('Ctrl Pts',(2.13097076359528,-26.2119746159478,-3.31226350660559));
#15515=CARTESIAN_POINT('Ctrl Pts',(2.34525647788099,-26.2119746159477,-1.05329767402633E-14));
#15516=CARTESIAN_POINT('Ctrl Pts',(2.55954219216671,-26.2119746159478,3.31226350660556));
#15517=CARTESIAN_POINT('Ctrl Pts',(2.77382790645242,-24.7748373407591,6.29650980834649));
#15518=CARTESIAN_POINT('Ctrl Pts',(2.98811362073814,-23.3377000655704,9.28075611008741));
#15519=CARTESIAN_POINT('Ctrl Pts',(3.20239933502385,-20.7480681778762,11.3459186275248));
#15520=CARTESIAN_POINT('Ctrl Pts',(3.41668504930956,-18.158436290182,13.4110811449623));
#15521=CARTESIAN_POINT('Ctrl Pts',(3.63097076359528,-14.929218145091,14.1481291139616));
#15522=CARTESIAN_POINT('Ctrl Pts',(3.84525647788099,-11.7,14.8851770829609));
#15523=CARTESIAN_POINT('Ctrl Pts',(4.05954219216671,-8.47078185490896,14.1481291139616));
#15524=CARTESIAN_POINT('Ctrl Pts',(4.27382790645242,-5.24156370981795,13.4110811449623));
#15525=CARTESIAN_POINT('Ctrl Pts',(4.48811362073814,-2.65193182212374,11.3459186275248));
#15526=CARTESIAN_POINT('Ctrl Pts',(4.70239933502385,-0.0622999344295592,
9.28075611008741));
#15527=CARTESIAN_POINT('Ctrl Pts',(4.91668504930956,1.37483734075912,6.2965098083465));
#15528=CARTESIAN_POINT('Ctrl Pts',(5.13097076359528,2.81197461594777,3.31226350660557));
#15529=CARTESIAN_POINT('Ctrl Pts',(5.34525647788099,2.81197461594778,0.));
#15530=CARTESIAN_POINT('Ctrl Pts',(5.55954219216671,2.81197461594777,-3.31226350660558));
#15531=CARTESIAN_POINT('Ctrl Pts',(5.77382790645242,1.37483734075912,-6.29650980834652));
#15532=CARTESIAN_POINT('Ctrl Pts',(5.98811362073814,-0.0622999344295592,
-9.28075611008745));
#15533=CARTESIAN_POINT('Ctrl Pts',(6.20239933502385,-2.65193182212375,-11.3459186275249));
#15534=CARTESIAN_POINT('Ctrl Pts',(6.41668504930957,-5.24156370981794,-13.4110811449623));
#15535=CARTESIAN_POINT('Ctrl Pts',(6.63097076359528,-8.47078185490895,-14.1481291139616));
#15536=CARTESIAN_POINT('Ctrl Pts',(6.84525647788099,-11.7,-14.8851770829609));
#15537=CARTESIAN_POINT('Ctrl Pts',(7.05954219216671,-14.929218145091,-14.1481291139616));
#15538=CARTESIAN_POINT('Ctrl Pts',(7.27382790645242,-18.158436290182,-13.4110811449623));
#15539=CARTESIAN_POINT('Ctrl Pts',(7.48811362073814,-20.7480681778762,-11.3459186275249));
#15540=CARTESIAN_POINT('Ctrl Pts',(7.70239933502385,-23.3377000655704,-9.28075611008746));
#15541=CARTESIAN_POINT('Ctrl Pts',(7.91668504930956,-24.7748373407591,-6.29650980834652));
#15542=CARTESIAN_POINT('Ctrl Pts',(8.13097076359528,-26.2119746159478,-3.3122635066056));
#15543=CARTESIAN_POINT('Ctrl Pts',(8.34525647788099,-26.2119746159478,-1.40439689870177E-14));
#15544=CARTESIAN_POINT('Ctrl Pts',(8.55954219216671,-26.2119746159478,3.31226350660556));
#15545=CARTESIAN_POINT('Ctrl Pts',(8.77382790645242,-24.7748373407591,6.29650980834649));
#15546=CARTESIAN_POINT('Ctrl Pts',(8.98811362073814,-23.3377000655704,9.28075611008742));
#15547=CARTESIAN_POINT('Ctrl Pts',(9.20239933502385,-20.7480681778762,11.3459186275248));
#15548=CARTESIAN_POINT('Ctrl Pts',(9.41668504930956,-18.158436290182,13.4110811449623));
#15549=CARTESIAN_POINT('Ctrl Pts',(9.63097076359528,-14.929218145091,14.1481291139616));
#15550=CARTESIAN_POINT('Ctrl Pts',(9.84525647788099,-11.7,14.8851770829608));
#15551=CARTESIAN_POINT('Ctrl Pts',(10.0595421921667,-8.47078185490896,14.1481291139616));
#15552=CARTESIAN_POINT('Ctrl Pts',(10.2738279064524,-5.24156370981795,13.4110811449623));
#15553=CARTESIAN_POINT('Ctrl Pts',(10.4881136207381,-2.65193182212374,11.3459186275248));
#15554=CARTESIAN_POINT('Ctrl Pts',(10.7023993350239,-0.0622999344295592,
9.28075611008741));
#15555=CARTESIAN_POINT('Ctrl Pts',(10.9166850493096,1.37483734075912,6.29650980834649));
#15556=CARTESIAN_POINT('Ctrl Pts',(11.1309707635953,2.81197461594777,3.31226350660557));
#15557=CARTESIAN_POINT('Ctrl Pts',(11.345256477881,2.81197461594777,3.51099224675442E-15));
#15558=CARTESIAN_POINT('Ctrl Pts',(11.5595421921667,2.81197461594777,-3.31226350660558));
#15559=CARTESIAN_POINT('Ctrl Pts',(11.7738279064524,1.37483734075912,-6.29650980834651));
#15560=CARTESIAN_POINT('Ctrl Pts',(11.9881136207381,-0.062299934429552,
-9.28075611008743));
#15561=CARTESIAN_POINT('Ctrl Pts',(12.2023993350239,-2.65193182212375,-11.3459186275249));
#15562=CARTESIAN_POINT('Ctrl Pts',(12.4166850493096,-5.24156370981794,-13.4110811449623));
#15563=CARTESIAN_POINT('Ctrl Pts',(12.6309707635953,-8.47078185490895,-14.1481291139616));
#15564=CARTESIAN_POINT('Ctrl Pts',(12.845256477881,-11.7,-14.8851770829609));
#15565=CARTESIAN_POINT('Ctrl Pts',(13.0595421921667,-14.929218145091,-14.1481291139616));
#15566=CARTESIAN_POINT('Ctrl Pts',(13.2738279064524,-18.158436290182,-13.4110811449623));
#15567=CARTESIAN_POINT('Ctrl Pts',(13.4881136207381,-20.7480681778762,-11.3459186275249));
#15568=CARTESIAN_POINT('Ctrl Pts',(13.7023993350239,-23.3377000655704,-9.28075611008744));
#15569=CARTESIAN_POINT('Ctrl Pts',(13.9166850493096,-24.7748373407591,-6.29650980834652));
#15570=CARTESIAN_POINT('Ctrl Pts',(14.1309707635953,-26.2119746159478,-3.3122635066056));
#15571=CARTESIAN_POINT('Ctrl Pts',(14.345256477881,-26.2119746159477,-7.02198449350884E-15));
#15572=CARTESIAN_POINT('Ctrl Pts',(14.5595421921667,-26.2119746159478,3.31226350660556));
#15573=CARTESIAN_POINT('Ctrl Pts',(14.7738279064524,-24.7748373407591,6.29650980834649));
#15574=CARTESIAN_POINT('Ctrl Pts',(14.9881136207381,-23.3377000655704,9.28075611008741));
#15575=CARTESIAN_POINT('Ctrl Pts',(15.2023993350239,-20.7480681778762,11.3459186275248));
#15576=CARTESIAN_POINT('Ctrl Pts',(15.4166850493096,-18.158436290182,13.4110811449623));
#15577=CARTESIAN_POINT('Ctrl Pts',(15.6309707635953,-14.929218145091,14.1481291139616));
#15578=CARTESIAN_POINT('Ctrl Pts',(15.845256477881,-11.7,14.8851770829609));
#15579=CARTESIAN_POINT('Ctrl Pts',(16.0595421921667,-8.47078185490896,14.1481291139616));
#15580=CARTESIAN_POINT('Ctrl Pts',(16.2738279064524,-5.24156370981795,13.4110811449623));
#15581=CARTESIAN_POINT('Ctrl Pts',(16.4881136207381,-2.65193182212376,11.3459186275248));
#15582=CARTESIAN_POINT('Ctrl Pts',(16.7023993350239,-0.0622999344295592,
9.28075611008741));
#15583=CARTESIAN_POINT('Ctrl Pts',(16.9166850493096,1.37483734075912,6.2965098083465));
#15584=CARTESIAN_POINT('Ctrl Pts',(17.1309707635953,2.81197461594777,3.31226350660556));
#15585=CARTESIAN_POINT('Ctrl Pts',(17.345256477881,2.81197461594778,-2.10659534805265E-14));
#15586=CARTESIAN_POINT('Ctrl Pts',(17.5595421921667,2.81197461594776,-3.31226350660559));
#15587=CARTESIAN_POINT('Ctrl Pts',(17.7738279064524,1.37483734075912,-6.2965098083465));
#15588=CARTESIAN_POINT('Ctrl Pts',(17.9881136207381,-0.0622999344295592,
-9.28075611008743));
#15589=CARTESIAN_POINT('Ctrl Pts',(18.2023993350238,-2.65193182212374,-11.3459186275249));
#15590=CARTESIAN_POINT('Ctrl Pts',(18.4166850493096,-5.24156370981794,-13.4110811449623));
#15591=CARTESIAN_POINT('Ctrl Pts',(18.6309707635953,-8.47078185490896,-14.1481291139616));
#15592=CARTESIAN_POINT('Ctrl Pts',(18.845256477881,-11.7,-14.8851770829609));
#15593=CARTESIAN_POINT('Ctrl Pts',(19.0595421921667,-14.929218145091,-14.1481291139616));
#15594=CARTESIAN_POINT('Ctrl Pts',(19.2738279064524,-18.158436290182,-13.4110811449623));
#15595=CARTESIAN_POINT('Ctrl Pts',(19.4881136207381,-20.7480681778762,-11.3459186275249));
#15596=CARTESIAN_POINT('Ctrl Pts',(19.7023993350239,-23.3377000655704,-9.28075611008744));
#15597=CARTESIAN_POINT('Ctrl Pts',(19.9166850493096,-24.7748373407591,-6.29650980834651));
#15598=CARTESIAN_POINT('Ctrl Pts',(20.1309707635953,-26.2119746159478,-3.3122635066056));
#15599=CARTESIAN_POINT('Ctrl Pts',(20.345256477881,-26.2119746159477,-1.05329767402633E-14));
#15600=CARTESIAN_POINT('Ctrl Pts',(20.5595421921667,-26.2119746159478,3.31226350660556));
#15601=CARTESIAN_POINT('Ctrl Pts',(20.7738279064524,-24.7748373407591,6.29650980834649));
#15602=CARTESIAN_POINT('Ctrl Pts',(20.9881136207381,-23.3377000655704,9.28075611008741));
#15603=CARTESIAN_POINT('Ctrl Pts',(21.2023993350239,-20.7480681778762,11.3459186275248));
#15604=CARTESIAN_POINT('Ctrl Pts',(21.4166850493096,-18.158436290182,13.4110811449623));
#15605=CARTESIAN_POINT('Ctrl Pts',(21.6309707635953,-14.929218145091,14.1481291139616));
#15606=CARTESIAN_POINT('Ctrl Pts',(21.845256477881,-11.7,14.8851770829608));
#15607=CARTESIAN_POINT('Ctrl Pts',(22.0595421921667,-8.47078185490896,14.1481291139616));
#15608=CARTESIAN_POINT('Ctrl Pts',(22.2738279064524,-5.24156370981795,13.4110811449623));
#15609=CARTESIAN_POINT('Ctrl Pts',(22.4881136207381,-2.65193182212374,11.3459186275248));
#15610=CARTESIAN_POINT('Ctrl Pts',(22.7023993350238,-0.0622999344295592,
9.28075611008741));
#15611=CARTESIAN_POINT('Ctrl Pts',(22.9166850493096,1.37483734075912,6.2965098083465));
#15612=CARTESIAN_POINT('Ctrl Pts',(23.1309707635953,2.81197461594777,3.31226350660557));
#15613=CARTESIAN_POINT('Ctrl Pts',(23.345256477881,2.81197461594778,-7.02198449350884E-15));
#15614=CARTESIAN_POINT('Ctrl Pts',(-0.97049399036428,1.5411253090549,-6.93889390390723E-15));
#15615=CARTESIAN_POINT('Ctrl Pts',(-0.756208276078568,1.5411253090549,-3.02220044537404));
#15616=CARTESIAN_POINT('Ctrl Pts',(-0.541922561792853,0.229841679453259,
-5.74510895921687));
#15617=CARTESIAN_POINT('Ctrl Pts',(-0.327636847507138,-1.08144195014838,
-8.4680174730597));
#15618=CARTESIAN_POINT('Ctrl Pts',(-0.113351133221425,-3.4442934046707,
-10.3523286299233));
#15619=CARTESIAN_POINT('Ctrl Pts',(0.10093458106429,-5.80714485919302,-12.236639786787));
#15620=CARTESIAN_POINT('Ctrl Pts',(0.315220295350005,-8.75357242959651,
-12.9091426524948));
#15621=CARTESIAN_POINT('Ctrl Pts',(0.529506009635718,-11.7,-13.5816455182026));
#15622=CARTESIAN_POINT('Ctrl Pts',(0.743791723921435,-14.6464275704035,
-12.9091426524948));
#15623=CARTESIAN_POINT('Ctrl Pts',(0.958077438207147,-17.592855140807,-12.236639786787));
#15624=CARTESIAN_POINT('Ctrl Pts',(1.17236315249286,-19.9557065953293,-10.3523286299233));
#15625=CARTESIAN_POINT('Ctrl Pts',(1.38664886677857,-22.3185580498516,-8.4680174730597));
#15626=CARTESIAN_POINT('Ctrl Pts',(1.60093458106429,-23.6298416794532,-5.74510895921687));
#15627=CARTESIAN_POINT('Ctrl Pts',(1.81522029535,-24.9411253090549,-3.02220044537404));
#15628=CARTESIAN_POINT('Ctrl Pts',(2.02950600963572,-24.9411253090549,6.93889390390723E-15));
#15629=CARTESIAN_POINT('Ctrl Pts',(2.24379172392143,-24.9411253090549,3.02220044537403));
#15630=CARTESIAN_POINT('Ctrl Pts',(2.45807743820715,-23.6298416794532,5.74510895921686));
#15631=CARTESIAN_POINT('Ctrl Pts',(2.67236315249286,-22.3185580498516,8.4680174730597));
#15632=CARTESIAN_POINT('Ctrl Pts',(2.88664886677858,-19.9557065953293,10.3523286299233));
#15633=CARTESIAN_POINT('Ctrl Pts',(3.10093458106429,-17.592855140807,12.236639786787));
#15634=CARTESIAN_POINT('Ctrl Pts',(3.31522029535001,-14.6464275704035,12.9091426524948));
#15635=CARTESIAN_POINT('Ctrl Pts',(3.52950600963572,-11.7,13.5816455182026));
#15636=CARTESIAN_POINT('Ctrl Pts',(3.74379172392143,-8.7535724295965,12.9091426524948));
#15637=CARTESIAN_POINT('Ctrl Pts',(3.95807743820715,-5.80714485919301,12.236639786787));
#15638=CARTESIAN_POINT('Ctrl Pts',(4.17236315249286,-3.4442934046707,10.3523286299233));
#15639=CARTESIAN_POINT('Ctrl Pts',(4.38664886677858,-1.08144195014837,8.46801747305969));
#15640=CARTESIAN_POINT('Ctrl Pts',(4.60093458106429,0.229841679453252,5.74510895921686));
#15641=CARTESIAN_POINT('Ctrl Pts',(4.81522029535,1.5411253090549,3.02220044537404));
#15642=CARTESIAN_POINT('Ctrl Pts',(5.02950600963572,1.5411253090549,0.));
#15643=CARTESIAN_POINT('Ctrl Pts',(5.24379172392143,1.5411253090549,-3.02220044537404));
#15644=CARTESIAN_POINT('Ctrl Pts',(5.45807743820715,0.229841679453252,-5.74510895921687));
#15645=CARTESIAN_POINT('Ctrl Pts',(5.67236315249286,-1.08144195014837,-8.4680174730597));
#15646=CARTESIAN_POINT('Ctrl Pts',(5.88664886677858,-3.4442934046707,-10.3523286299233));
#15647=CARTESIAN_POINT('Ctrl Pts',(6.10093458106429,-5.80714485919301,-12.236639786787));
#15648=CARTESIAN_POINT('Ctrl Pts',(6.31522029535001,-8.75357242959651,-12.9091426524948));
#15649=CARTESIAN_POINT('Ctrl Pts',(6.52950600963572,-11.7,-13.5816455182026));
#15650=CARTESIAN_POINT('Ctrl Pts',(6.74379172392144,-14.6464275704035,-12.9091426524948));
#15651=CARTESIAN_POINT('Ctrl Pts',(6.95807743820715,-17.592855140807,-12.236639786787));
#15652=CARTESIAN_POINT('Ctrl Pts',(7.17236315249286,-19.9557065953293,-10.3523286299233));
#15653=CARTESIAN_POINT('Ctrl Pts',(7.38664886677858,-22.3185580498516,-8.4680174730597));
#15654=CARTESIAN_POINT('Ctrl Pts',(7.60093458106429,-23.6298416794532,-5.74510895921687));
#15655=CARTESIAN_POINT('Ctrl Pts',(7.81522029535,-24.9411253090549,-3.02220044537404));
#15656=CARTESIAN_POINT('Ctrl Pts',(8.02950600963572,-24.9411253090549,-6.93889390390723E-15));
#15657=CARTESIAN_POINT('Ctrl Pts',(8.24379172392143,-24.9411253090549,3.02220044537402));
#15658=CARTESIAN_POINT('Ctrl Pts',(8.45807743820715,-23.6298416794532,5.74510895921685));
#15659=CARTESIAN_POINT('Ctrl Pts',(8.67236315249286,-22.3185580498516,8.4680174730597));
#15660=CARTESIAN_POINT('Ctrl Pts',(8.88664886677858,-19.9557065953293,10.3523286299233));
#15661=CARTESIAN_POINT('Ctrl Pts',(9.10093458106429,-17.592855140807,12.236639786787));
#15662=CARTESIAN_POINT('Ctrl Pts',(9.31522029535001,-14.6464275704035,12.9091426524948));
#15663=CARTESIAN_POINT('Ctrl Pts',(9.52950600963572,-11.7,13.5816455182026));
#15664=CARTESIAN_POINT('Ctrl Pts',(9.74379172392144,-8.75357242959651,12.9091426524948));
#15665=CARTESIAN_POINT('Ctrl Pts',(9.95807743820714,-5.80714485919302,12.236639786787));
#15666=CARTESIAN_POINT('Ctrl Pts',(10.1723631524929,-3.4442934046707,10.3523286299233));
#15667=CARTESIAN_POINT('Ctrl Pts',(10.3866488667786,-1.08144195014837,8.4680174730597));
#15668=CARTESIAN_POINT('Ctrl Pts',(10.6009345810643,0.229841679453252,5.74510895921686));
#15669=CARTESIAN_POINT('Ctrl Pts',(10.81522029535,1.5411253090549,3.02220044537402));
#15670=CARTESIAN_POINT('Ctrl Pts',(11.0295060096357,1.5411253090549,6.93889390390723E-15));
#15671=CARTESIAN_POINT('Ctrl Pts',(11.2437917239214,1.54112530905489,-3.02220044537404));
#15672=CARTESIAN_POINT('Ctrl Pts',(11.4580774382071,0.229841679453259,-5.74510895921686));
#15673=CARTESIAN_POINT('Ctrl Pts',(11.6723631524929,-1.08144195014837,-8.4680174730597));
#15674=CARTESIAN_POINT('Ctrl Pts',(11.8866488667786,-3.4442934046707,-10.3523286299233));
#15675=CARTESIAN_POINT('Ctrl Pts',(12.1009345810643,-5.80714485919302,-12.236639786787));
#15676=CARTESIAN_POINT('Ctrl Pts',(12.31522029535,-8.75357242959649,-12.9091426524948));
#15677=CARTESIAN_POINT('Ctrl Pts',(12.5295060096357,-11.7,-13.5816455182026));
#15678=CARTESIAN_POINT('Ctrl Pts',(12.7437917239214,-14.6464275704035,-12.9091426524948));
#15679=CARTESIAN_POINT('Ctrl Pts',(12.9580774382071,-17.592855140807,-12.236639786787));
#15680=CARTESIAN_POINT('Ctrl Pts',(13.1723631524929,-19.9557065953293,-10.3523286299233));
#15681=CARTESIAN_POINT('Ctrl Pts',(13.3866488667786,-22.3185580498516,-8.4680174730597));
#15682=CARTESIAN_POINT('Ctrl Pts',(13.6009345810643,-23.6298416794532,-5.74510895921687));
#15683=CARTESIAN_POINT('Ctrl Pts',(13.81522029535,-24.9411253090549,-3.02220044537403));
#15684=CARTESIAN_POINT('Ctrl Pts',(14.0295060096357,-24.9411253090549,-6.93889390390723E-15));
#15685=CARTESIAN_POINT('Ctrl Pts',(14.2437917239214,-24.9411253090549,3.02220044537403));
#15686=CARTESIAN_POINT('Ctrl Pts',(14.4580774382072,-23.6298416794532,5.74510895921685));
#15687=CARTESIAN_POINT('Ctrl Pts',(14.6723631524929,-22.3185580498516,8.46801747305969));
#15688=CARTESIAN_POINT('Ctrl Pts',(14.8866488667786,-19.9557065953293,10.3523286299233));
#15689=CARTESIAN_POINT('Ctrl Pts',(15.1009345810643,-17.592855140807,12.236639786787));
#15690=CARTESIAN_POINT('Ctrl Pts',(15.31522029535,-14.6464275704035,12.9091426524948));
#15691=CARTESIAN_POINT('Ctrl Pts',(15.5295060096357,-11.7,13.5816455182026));
#15692=CARTESIAN_POINT('Ctrl Pts',(15.7437917239214,-8.75357242959651,12.9091426524948));
#15693=CARTESIAN_POINT('Ctrl Pts',(15.9580774382071,-5.80714485919302,12.236639786787));
#15694=CARTESIAN_POINT('Ctrl Pts',(16.1723631524929,-3.4442934046707,10.3523286299233));
#15695=CARTESIAN_POINT('Ctrl Pts',(16.3866488667786,-1.08144195014837,8.46801747305969));
#15696=CARTESIAN_POINT('Ctrl Pts',(16.6009345810643,0.229841679453266,5.74510895921686));
#15697=CARTESIAN_POINT('Ctrl Pts',(16.81522029535,1.5411253090549,3.02220044537404));
#15698=CARTESIAN_POINT('Ctrl Pts',(17.0295060096357,1.5411253090549,-2.08166817117217E-14));
#15699=CARTESIAN_POINT('Ctrl Pts',(17.2437917239214,1.5411253090549,-3.02220044537405));
#15700=CARTESIAN_POINT('Ctrl Pts',(17.4580774382072,0.229841679453266,-5.74510895921688));
#15701=CARTESIAN_POINT('Ctrl Pts',(17.6723631524929,-1.08144195014837,-8.46801747305971));
#15702=CARTESIAN_POINT('Ctrl Pts',(17.8866488667786,-3.44429340467071,-10.3523286299233));
#15703=CARTESIAN_POINT('Ctrl Pts',(18.1009345810643,-5.80714485919302,-12.236639786787));
#15704=CARTESIAN_POINT('Ctrl Pts',(18.31522029535,-8.75357242959651,-12.9091426524948));
#15705=CARTESIAN_POINT('Ctrl Pts',(18.5295060096357,-11.7,-13.5816455182026));
#15706=CARTESIAN_POINT('Ctrl Pts',(18.7437917239214,-14.6464275704035,-12.9091426524948));
#15707=CARTESIAN_POINT('Ctrl Pts',(18.9580774382071,-17.592855140807,-12.236639786787));
#15708=CARTESIAN_POINT('Ctrl Pts',(19.1723631524929,-19.9557065953293,-10.3523286299233));
#15709=CARTESIAN_POINT('Ctrl Pts',(19.3866488667786,-22.3185580498516,-8.4680174730597));
#15710=CARTESIAN_POINT('Ctrl Pts',(19.6009345810643,-23.6298416794532,-5.74510895921687));
#15711=CARTESIAN_POINT('Ctrl Pts',(19.81522029535,-24.9411253090549,-3.02220044537404));
#15712=CARTESIAN_POINT('Ctrl Pts',(20.0295060096357,-24.9411253090549,0.));
#15713=CARTESIAN_POINT('Ctrl Pts',(20.2437917239214,-24.9411253090549,3.02220044537403));
#15714=CARTESIAN_POINT('Ctrl Pts',(20.4580774382071,-23.6298416794532,5.74510895921685));
#15715=CARTESIAN_POINT('Ctrl Pts',(20.6723631524929,-22.3185580498516,8.46801747305969));
#15716=CARTESIAN_POINT('Ctrl Pts',(20.8866488667786,-19.9557065953293,10.3523286299233));
#15717=CARTESIAN_POINT('Ctrl Pts',(21.1009345810643,-17.5928551408069,12.236639786787));
#15718=CARTESIAN_POINT('Ctrl Pts',(21.31522029535,-14.6464275704035,12.9091426524948));
#15719=CARTESIAN_POINT('Ctrl Pts',(21.5295060096357,-11.7,13.5816455182026));
#15720=CARTESIAN_POINT('Ctrl Pts',(21.7437917239214,-8.75357242959651,12.9091426524948));
#15721=CARTESIAN_POINT('Ctrl Pts',(21.9580774382071,-5.80714485919301,12.236639786787));
#15722=CARTESIAN_POINT('Ctrl Pts',(22.1723631524929,-3.4442934046707,10.3523286299233));
#15723=CARTESIAN_POINT('Ctrl Pts',(22.3866488667786,-1.08144195014837,8.4680174730597));
#15724=CARTESIAN_POINT('Ctrl Pts',(22.6009345810643,0.229841679453259,5.74510895921686));
#15725=CARTESIAN_POINT('Ctrl Pts',(22.81522029535,1.54112530905491,3.02220044537404));
#15726=CARTESIAN_POINT('Ctrl Pts',(23.0295060096357,1.5411253090549,0.));
#15727=CARTESIAN_POINT('',(0.970493990364278,1.5411253090549,-1.38777878078145E-14));
#15728=CARTESIAN_POINT('Origin',(-2.60208521396521E-15,1.30000000000001,
-2.08166817117217E-14));
#15729=CARTESIAN_POINT('Ctrl Pts',(0.970493990364278,1.5411253090549,-1.38777878078145E-14));
#15730=CARTESIAN_POINT('Ctrl Pts',(1.18477970464999,1.54112530905491,-3.02220044537403));
#15731=CARTESIAN_POINT('Ctrl Pts',(1.39906541893571,0.229841679453259,-5.74510895921686));
#15732=CARTESIAN_POINT('Ctrl Pts',(1.61335113322142,-1.08144195014838,-8.4680174730597));
#15733=CARTESIAN_POINT('Ctrl Pts',(1.82763684750713,-3.44429340467071,-10.3523286299233));
#15734=CARTESIAN_POINT('Ctrl Pts',(2.04192256179285,-5.80714485919301,-12.236639786787));
#15735=CARTESIAN_POINT('Ctrl Pts',(2.25620827607856,-8.75357242959651,-12.9091426524948));
#15736=CARTESIAN_POINT('Ctrl Pts',(2.47049399036428,-11.7,-13.5816455182026));
#15737=CARTESIAN_POINT('Ctrl Pts',(2.68477970464999,-14.6464275704035,-12.9091426524948));
#15738=CARTESIAN_POINT('Ctrl Pts',(2.89906541893571,-17.592855140807,-12.236639786787));
#15739=CARTESIAN_POINT('Ctrl Pts',(3.11335113322142,-19.9557065953293,-10.3523286299233));
#15740=CARTESIAN_POINT('Ctrl Pts',(3.32763684750713,-22.3185580498516,-8.4680174730597));
#15741=CARTESIAN_POINT('Ctrl Pts',(3.54192256179285,-23.6298416794532,-5.74510895921686));
#15742=CARTESIAN_POINT('Ctrl Pts',(3.75620827607856,-24.9411253090549,-3.02220044537403));
#15743=CARTESIAN_POINT('Ctrl Pts',(3.97049399036428,-24.9411253090549,3.46944695195361E-15));
#15744=CARTESIAN_POINT('Ctrl Pts',(4.18477970464999,-24.9411253090549,3.02220044537403));
#15745=CARTESIAN_POINT('Ctrl Pts',(4.39906541893571,-23.6298416794532,5.74510895921686));
#15746=CARTESIAN_POINT('Ctrl Pts',(4.61335113322142,-22.3185580498516,8.46801747305969));
#15747=CARTESIAN_POINT('Ctrl Pts',(4.82763684750714,-19.9557065953293,10.3523286299233));
#15748=CARTESIAN_POINT('Ctrl Pts',(5.04192256179285,-17.592855140807,12.2366397867869));
#15749=CARTESIAN_POINT('Ctrl Pts',(5.25620827607856,-14.6464275704035,12.9091426524948));
#15750=CARTESIAN_POINT('Ctrl Pts',(5.47049399036428,-11.7,13.5816455182026));
#15751=CARTESIAN_POINT('Ctrl Pts',(5.68477970464999,-8.75357242959651,12.9091426524948));
#15752=CARTESIAN_POINT('Ctrl Pts',(5.89906541893571,-5.80714485919302,12.236639786787));
#15753=CARTESIAN_POINT('Ctrl Pts',(6.11335113322142,-3.4442934046707,10.3523286299233));
#15754=CARTESIAN_POINT('Ctrl Pts',(6.32763684750713,-1.08144195014838,8.4680174730597));
#15755=CARTESIAN_POINT('Ctrl Pts',(6.54192256179285,0.229841679453252,5.74510895921686));
#15756=CARTESIAN_POINT('Ctrl Pts',(6.75620827607856,1.5411253090549,3.02220044537404));
#15757=CARTESIAN_POINT('Ctrl Pts',(6.97049399036428,1.5411253090549,-1.38777878078145E-14));
#15758=CARTESIAN_POINT('Ctrl Pts',(7.18477970464999,1.5411253090549,-3.02220044537404));
#15759=CARTESIAN_POINT('Ctrl Pts',(7.39906541893571,0.229841679453259,-5.74510895921689));
#15760=CARTESIAN_POINT('Ctrl Pts',(7.61335113322142,-1.08144195014838,-8.46801747305971));
#15761=CARTESIAN_POINT('Ctrl Pts',(7.82763684750713,-3.4442934046707,-10.3523286299233));
#15762=CARTESIAN_POINT('Ctrl Pts',(8.04192256179285,-5.80714485919302,-12.236639786787));
#15763=CARTESIAN_POINT('Ctrl Pts',(8.25620827607856,-8.75357242959651,-12.9091426524948));
#15764=CARTESIAN_POINT('Ctrl Pts',(8.47049399036428,-11.7,-13.5816455182026));
#15765=CARTESIAN_POINT('Ctrl Pts',(8.68477970464999,-14.6464275704035,-12.9091426524948));
#15766=CARTESIAN_POINT('Ctrl Pts',(8.89906541893571,-17.592855140807,-12.236639786787));
#15767=CARTESIAN_POINT('Ctrl Pts',(9.11335113322142,-19.9557065953293,-10.3523286299233));
#15768=CARTESIAN_POINT('Ctrl Pts',(9.32763684750714,-22.3185580498516,-8.4680174730597));
#15769=CARTESIAN_POINT('Ctrl Pts',(9.54192256179285,-23.6298416794532,-5.74510895921687));
#15770=CARTESIAN_POINT('Ctrl Pts',(9.75620827607856,-24.9411253090549,-3.02220044537404));
#15771=CARTESIAN_POINT('Ctrl Pts',(9.97049399036428,-24.9411253090549,-6.93889390390723E-15));
#15772=CARTESIAN_POINT('Ctrl Pts',(10.18477970465,-24.9411253090549,3.02220044537403));
#15773=CARTESIAN_POINT('Ctrl Pts',(10.3990654189357,-23.6298416794532,5.74510895921686));
#15774=CARTESIAN_POINT('Ctrl Pts',(10.6133511332214,-22.3185580498516,8.4680174730597));
#15775=CARTESIAN_POINT('Ctrl Pts',(10.8276368475071,-19.9557065953293,10.3523286299233));
#15776=CARTESIAN_POINT('Ctrl Pts',(11.0419225617928,-17.592855140807,12.236639786787));
#15777=CARTESIAN_POINT('Ctrl Pts',(11.2562082760786,-14.6464275704035,12.9091426524948));
#15778=CARTESIAN_POINT('Ctrl Pts',(11.4704939903643,-11.7,13.5816455182026));
#15779=CARTESIAN_POINT('Ctrl Pts',(11.68477970465,-8.75357242959651,12.9091426524948));
#15780=CARTESIAN_POINT('Ctrl Pts',(11.8990654189357,-5.80714485919301,12.236639786787));
#15781=CARTESIAN_POINT('Ctrl Pts',(12.1133511332214,-3.4442934046707,10.3523286299233));
#15782=CARTESIAN_POINT('Ctrl Pts',(12.3276368475071,-1.08144195014836,8.4680174730597));
#15783=CARTESIAN_POINT('Ctrl Pts',(12.5419225617929,0.229841679453266,5.74510895921686));
#15784=CARTESIAN_POINT('Ctrl Pts',(12.7562082760786,1.5411253090549,3.02220044537403));
#15785=CARTESIAN_POINT('Ctrl Pts',(12.9704939903643,1.5411253090549,-2.08166817117217E-14));
#15786=CARTESIAN_POINT('Ctrl Pts',(13.18477970465,1.5411253090549,-3.02220044537405));
#15787=CARTESIAN_POINT('Ctrl Pts',(13.3990654189357,0.229841679453252,-5.74510895921687));
#15788=CARTESIAN_POINT('Ctrl Pts',(13.6133511332214,-1.08144195014838,-8.46801747305971));
#15789=CARTESIAN_POINT('Ctrl Pts',(13.8276368475071,-3.44429340467069,-10.3523286299233));
#15790=CARTESIAN_POINT('Ctrl Pts',(14.0419225617929,-5.80714485919301,-12.236639786787));
#15791=CARTESIAN_POINT('Ctrl Pts',(14.2562082760786,-8.75357242959651,-12.9091426524948));
#15792=CARTESIAN_POINT('Ctrl Pts',(14.4704939903643,-11.7,-13.5816455182026));
#15793=CARTESIAN_POINT('Ctrl Pts',(14.68477970465,-14.6464275704035,-12.9091426524948));
#15794=CARTESIAN_POINT('Ctrl Pts',(14.8990654189357,-17.592855140807,-12.236639786787));
#15795=CARTESIAN_POINT('Ctrl Pts',(15.1133511332214,-19.9557065953293,-10.3523286299233));
#15796=CARTESIAN_POINT('Ctrl Pts',(15.3276368475071,-22.3185580498516,-8.46801747305969));
#15797=CARTESIAN_POINT('Ctrl Pts',(15.5419225617929,-23.6298416794532,-5.74510895921687));
#15798=CARTESIAN_POINT('Ctrl Pts',(15.7562082760786,-24.9411253090549,-3.02220044537403));
#15799=CARTESIAN_POINT('Ctrl Pts',(15.9704939903643,-24.9411253090549,-6.93889390390723E-15));
#15800=CARTESIAN_POINT('Ctrl Pts',(16.18477970465,-24.9411253090549,3.02220044537403));
#15801=CARTESIAN_POINT('Ctrl Pts',(16.3990654189357,-23.6298416794532,5.74510895921686));
#15802=CARTESIAN_POINT('Ctrl Pts',(16.6133511332214,-22.3185580498516,8.46801747305969));
#15803=CARTESIAN_POINT('Ctrl Pts',(16.8276368475071,-19.9557065953293,10.3523286299233));
#15804=CARTESIAN_POINT('Ctrl Pts',(17.0419225617928,-17.592855140807,12.236639786787));
#15805=CARTESIAN_POINT('Ctrl Pts',(17.2562082760786,-14.6464275704035,12.9091426524948));
#15806=CARTESIAN_POINT('Ctrl Pts',(17.4704939903643,-11.7,13.5816455182026));
#15807=CARTESIAN_POINT('Ctrl Pts',(17.68477970465,-8.75357242959651,12.9091426524948));
#15808=CARTESIAN_POINT('Ctrl Pts',(17.8990654189357,-5.80714485919301,12.236639786787));
#15809=CARTESIAN_POINT('Ctrl Pts',(18.1133511332214,-3.4442934046707,10.3523286299233));
#15810=CARTESIAN_POINT('Ctrl Pts',(18.3276368475071,-1.08144195014837,8.46801747305969));
#15811=CARTESIAN_POINT('Ctrl Pts',(18.5419225617928,0.229841679453252,5.74510895921686));
#15812=CARTESIAN_POINT('Ctrl Pts',(18.7562082760786,1.5411253090549,3.02220044537405));
#15813=CARTESIAN_POINT('Ctrl Pts',(18.9704939903643,1.5411253090549,-1.38777878078145E-14));
#15814=CARTESIAN_POINT('Ctrl Pts',(19.18477970465,1.5411253090549,-3.02220044537404));
#15815=CARTESIAN_POINT('Ctrl Pts',(19.3990654189357,0.229841679453259,-5.74510895921686));
#15816=CARTESIAN_POINT('Ctrl Pts',(19.6133511332214,-1.08144195014838,-8.4680174730597));
#15817=CARTESIAN_POINT('Ctrl Pts',(19.8276368475071,-3.4442934046707,-10.3523286299233));
#15818=CARTESIAN_POINT('Ctrl Pts',(20.0419225617929,-5.80714485919302,-12.236639786787));
#15819=CARTESIAN_POINT('Ctrl Pts',(20.2562082760786,-8.75357242959651,-12.9091426524948));
#15820=CARTESIAN_POINT('Ctrl Pts',(20.4704939903643,-11.7,-13.5816455182026));
#15821=CARTESIAN_POINT('Ctrl Pts',(20.68477970465,-14.6464275704035,-12.9091426524948));
#15822=CARTESIAN_POINT('Ctrl Pts',(20.8990654189357,-17.592855140807,-12.236639786787));
#15823=CARTESIAN_POINT('Ctrl Pts',(21.1133511332214,-19.9557065953293,-10.3523286299233));
#15824=CARTESIAN_POINT('Ctrl Pts',(21.3276368475071,-22.3185580498516,-8.4680174730597));
#15825=CARTESIAN_POINT('Ctrl Pts',(21.5419225617929,-23.6298416794532,-5.74510895921687));
#15826=CARTESIAN_POINT('Ctrl Pts',(21.7562082760786,-24.9411253090549,-3.02220044537404));
#15827=CARTESIAN_POINT('Ctrl Pts',(21.9704939903643,-24.9411253090549,-3.46944695195361E-15));
#15828=CARTESIAN_POINT('Ctrl Pts',(22.18477970465,-24.9411253090549,3.02220044537403));
#15829=CARTESIAN_POINT('Ctrl Pts',(22.3990654189357,-23.6298416794532,5.74510895921686));
#15830=CARTESIAN_POINT('Ctrl Pts',(22.6133511332214,-22.3185580498516,8.46801747305969));
#15831=CARTESIAN_POINT('Ctrl Pts',(22.8276368475071,-19.9557065953293,10.3523286299233));
#15832=CARTESIAN_POINT('Ctrl Pts',(23.0419225617928,-17.592855140807,12.236639786787));
#15833=CARTESIAN_POINT('Ctrl Pts',(23.2562082760786,-14.6464275704035,12.9091426524948));
#15834=CARTESIAN_POINT('Ctrl Pts',(23.4704939903643,-11.7,13.5816455182026));
#15835=CARTESIAN_POINT('Ctrl Pts',(23.68477970465,-8.75357242959651,12.9091426524948));
#15836=CARTESIAN_POINT('Ctrl Pts',(23.8990654189357,-5.80714485919302,12.236639786787));
#15837=CARTESIAN_POINT('Ctrl Pts',(24.1133511332214,-3.4442934046707,10.3523286299233));
#15838=CARTESIAN_POINT('Ctrl Pts',(24.3276368475071,-1.08144195014837,8.46801747305969));
#15839=CARTESIAN_POINT('Ctrl Pts',(24.5419225617928,0.229841679453252,5.74510895921686));
#15840=CARTESIAN_POINT('Ctrl Pts',(24.7562082760786,1.5411253090549,3.02220044537404));
#15841=CARTESIAN_POINT('Ctrl Pts',(24.9704939903643,1.5411253090549,0.));
#15842=CARTESIAN_POINT('Ctrl Pts',(1.9,-2.19999999999999,0.));
#15843=CARTESIAN_POINT('Ctrl Pts',(2.11428571428571,-2.19999999999999,-2.16831300670642));
#15844=CARTESIAN_POINT('Ctrl Pts',(2.32857142857143,-3.14079575492701,-4.12189552161681));
#15845=CARTESIAN_POINT('Ctrl Pts',(2.54285714285714,-4.08159150985404,-6.07547803652717));
#15846=CARTESIAN_POINT('Ctrl Pts',(2.75714285714286,-5.77684688234201,-7.42739908344628));
#15847=CARTESIAN_POINT('Ctrl Pts',(2.97142857142857,-7.47210225483002,-8.77932013036538));
#15848=CARTESIAN_POINT('Ctrl Pts',(3.18571428571428,-9.58605112741501,-9.26181516572732));
#15849=CARTESIAN_POINT('Ctrl Pts',(3.4,-11.7,-9.74431020108927));
#15850=CARTESIAN_POINT('Ctrl Pts',(3.61428571428571,-13.813948872585,-9.26181516572732));
#15851=CARTESIAN_POINT('Ctrl Pts',(3.82857142857143,-15.92789774517,-8.77932013036538));
#15852=CARTESIAN_POINT('Ctrl Pts',(4.04285714285714,-17.623153117658,-7.42739908344629));
#15853=CARTESIAN_POINT('Ctrl Pts',(4.25714285714286,-19.3184084901459,-6.07547803652718));
#15854=CARTESIAN_POINT('Ctrl Pts',(4.47142857142857,-20.259204245073,-4.12189552161681));
#15855=CARTESIAN_POINT('Ctrl Pts',(4.68571428571428,-21.2,-2.16831300670643));
#15856=CARTESIAN_POINT('Ctrl Pts',(4.9,-21.2,-6.93889390390723E-15));
#15857=CARTESIAN_POINT('Ctrl Pts',(5.11428571428571,-21.2,2.16831300670641));
#15858=CARTESIAN_POINT('Ctrl Pts',(5.32857142857143,-20.259204245073,4.12189552161679));
#15859=CARTESIAN_POINT('Ctrl Pts',(5.54285714285714,-19.3184084901459,6.07547803652717));
#15860=CARTESIAN_POINT('Ctrl Pts',(5.75714285714286,-17.623153117658,7.42739908344627));
#15861=CARTESIAN_POINT('Ctrl Pts',(5.97142857142857,-15.92789774517,8.77932013036537));
#15862=CARTESIAN_POINT('Ctrl Pts',(6.18571428571429,-13.813948872585,9.26181516572732));
#15863=CARTESIAN_POINT('Ctrl Pts',(6.4,-11.7,9.74431020108925));
#15864=CARTESIAN_POINT('Ctrl Pts',(6.61428571428571,-9.586051127415,9.26181516572731));
#15865=CARTESIAN_POINT('Ctrl Pts',(6.82857142857143,-7.47210225483002,8.77932013036537));
#15866=CARTESIAN_POINT('Ctrl Pts',(7.04285714285714,-5.77684688234203,7.42739908344628));
#15867=CARTESIAN_POINT('Ctrl Pts',(7.25714285714285,-4.08159150985402,6.07547803652718));
#15868=CARTESIAN_POINT('Ctrl Pts',(7.47142857142857,-3.14079575492702,4.12189552161681));
#15869=CARTESIAN_POINT('Ctrl Pts',(7.68571428571429,-2.2,2.16831300670643));
#15870=CARTESIAN_POINT('Ctrl Pts',(7.9,-2.19999999999999,6.93889390390723E-15));
#15871=CARTESIAN_POINT('Ctrl Pts',(8.11428571428571,-2.19999999999999,-2.16831300670641));
#15872=CARTESIAN_POINT('Ctrl Pts',(8.32857142857143,-3.14079575492703,-4.1218955216168));
#15873=CARTESIAN_POINT('Ctrl Pts',(8.54285714285714,-4.08159150985404,-6.07547803652717));
#15874=CARTESIAN_POINT('Ctrl Pts',(8.75714285714286,-5.77684688234202,-7.42739908344627));
#15875=CARTESIAN_POINT('Ctrl Pts',(8.97142857142857,-7.47210225483002,-8.77932013036538));
#15876=CARTESIAN_POINT('Ctrl Pts',(9.18571428571429,-9.58605112741501,-9.26181516572732));
#15877=CARTESIAN_POINT('Ctrl Pts',(9.4,-11.7,-9.74431020108925));
#15878=CARTESIAN_POINT('Ctrl Pts',(9.61428571428572,-13.813948872585,-9.26181516572732));
#15879=CARTESIAN_POINT('Ctrl Pts',(9.82857142857143,-15.92789774517,-8.77932013036538));
#15880=CARTESIAN_POINT('Ctrl Pts',(10.0428571428571,-17.6231531176579,-7.42739908344629));
#15881=CARTESIAN_POINT('Ctrl Pts',(10.2571428571429,-19.3184084901459,-6.07547803652717));
#15882=CARTESIAN_POINT('Ctrl Pts',(10.4714285714286,-20.259204245073,-4.1218955216168));
#15883=CARTESIAN_POINT('Ctrl Pts',(10.6857142857143,-21.2,-2.16831300670643));
#15884=CARTESIAN_POINT('Ctrl Pts',(10.9,-21.2,-6.93889390390723E-15));
#15885=CARTESIAN_POINT('Ctrl Pts',(11.1142857142857,-21.2,2.16831300670642));
#15886=CARTESIAN_POINT('Ctrl Pts',(11.3285714285714,-20.259204245073,4.12189552161679));
#15887=CARTESIAN_POINT('Ctrl Pts',(11.5428571428571,-19.3184084901459,6.07547803652716));
#15888=CARTESIAN_POINT('Ctrl Pts',(11.7571428571429,-17.623153117658,7.42739908344626));
#15889=CARTESIAN_POINT('Ctrl Pts',(11.9714285714286,-15.92789774517,8.77932013036537));
#15890=CARTESIAN_POINT('Ctrl Pts',(12.1857142857143,-13.813948872585,9.26181516572731));
#15891=CARTESIAN_POINT('Ctrl Pts',(12.4,-11.7,9.74431020108925));
#15892=CARTESIAN_POINT('Ctrl Pts',(12.6142857142857,-9.58605112741501,9.26181516572731));
#15893=CARTESIAN_POINT('Ctrl Pts',(12.8285714285714,-7.47210225483002,8.77932013036537));
#15894=CARTESIAN_POINT('Ctrl Pts',(13.0428571428571,-5.77684688234202,7.42739908344626));
#15895=CARTESIAN_POINT('Ctrl Pts',(13.2571428571429,-4.08159150985402,6.07547803652717));
#15896=CARTESIAN_POINT('Ctrl Pts',(13.4714285714286,-3.14079575492703,4.1218955216168));
#15897=CARTESIAN_POINT('Ctrl Pts',(13.6857142857143,-2.2,2.16831300670642));
#15898=CARTESIAN_POINT('Ctrl Pts',(13.9,-2.2,-6.93889390390723E-15));
#15899=CARTESIAN_POINT('Ctrl Pts',(14.1142857142857,-2.19999999999999,-2.16831300670644));
#15900=CARTESIAN_POINT('Ctrl Pts',(14.3285714285714,-3.14079575492702,-4.1218955216168));
#15901=CARTESIAN_POINT('Ctrl Pts',(14.5428571428571,-4.08159150985404,-6.07547803652717));
#15902=CARTESIAN_POINT('Ctrl Pts',(14.7571428571429,-5.77684688234202,-7.42739908344627));
#15903=CARTESIAN_POINT('Ctrl Pts',(14.9714285714286,-7.47210225483002,-8.77932013036538));
#15904=CARTESIAN_POINT('Ctrl Pts',(15.1857142857143,-9.58605112741499,-9.26181516572731));
#15905=CARTESIAN_POINT('Ctrl Pts',(15.4,-11.7,-9.74431020108925));
#15906=CARTESIAN_POINT('Ctrl Pts',(15.6142857142857,-13.813948872585,-9.26181516572732));
#15907=CARTESIAN_POINT('Ctrl Pts',(15.8285714285714,-15.92789774517,-8.77932013036537));
#15908=CARTESIAN_POINT('Ctrl Pts',(16.0428571428571,-17.6231531176579,-7.42739908344629));
#15909=CARTESIAN_POINT('Ctrl Pts',(16.2571428571428,-19.3184084901459,-6.07547803652718));
#15910=CARTESIAN_POINT('Ctrl Pts',(16.4714285714286,-20.259204245073,-4.12189552161682));
#15911=CARTESIAN_POINT('Ctrl Pts',(16.6857142857143,-21.2,-2.16831300670643));
#15912=CARTESIAN_POINT('Ctrl Pts',(16.9,-21.2,0.));
#15913=CARTESIAN_POINT('Ctrl Pts',(17.1142857142857,-21.2,2.16831300670642));
#15914=CARTESIAN_POINT('Ctrl Pts',(17.3285714285714,-20.259204245073,4.12189552161679));
#15915=CARTESIAN_POINT('Ctrl Pts',(17.5428571428572,-19.318408490146,6.07547803652717));
#15916=CARTESIAN_POINT('Ctrl Pts',(17.7571428571429,-17.623153117658,7.42739908344627));
#15917=CARTESIAN_POINT('Ctrl Pts',(17.9714285714286,-15.92789774517,8.77932013036537));
#15918=CARTESIAN_POINT('Ctrl Pts',(18.1857142857143,-13.813948872585,9.26181516572731));
#15919=CARTESIAN_POINT('Ctrl Pts',(18.4,-11.7,9.74431020108925));
#15920=CARTESIAN_POINT('Ctrl Pts',(18.6142857142857,-9.58605112741501,9.26181516572731));
#15921=CARTESIAN_POINT('Ctrl Pts',(18.8285714285714,-7.47210225483001,8.77932013036538));
#15922=CARTESIAN_POINT('Ctrl Pts',(19.0428571428571,-5.77684688234202,7.42739908344627));
#15923=CARTESIAN_POINT('Ctrl Pts',(19.2571428571429,-4.08159150985404,6.07547803652718));
#15924=CARTESIAN_POINT('Ctrl Pts',(19.4714285714286,-3.14079575492701,4.12189552161679));
#15925=CARTESIAN_POINT('Ctrl Pts',(19.6857142857143,-2.20000000000001,2.16831300670641));
#15926=CARTESIAN_POINT('Ctrl Pts',(19.9,-2.2,-1.38777878078145E-14));
#15927=CARTESIAN_POINT('Ctrl Pts',(20.1142857142857,-2.2,-2.16831300670642));
#15928=CARTESIAN_POINT('Ctrl Pts',(20.3285714285714,-3.14079575492703,-4.12189552161681));
#15929=CARTESIAN_POINT('Ctrl Pts',(20.5428571428571,-4.08159150985403,-6.07547803652718));
#15930=CARTESIAN_POINT('Ctrl Pts',(20.7571428571428,-5.77684688234203,-7.42739908344629));
#15931=CARTESIAN_POINT('Ctrl Pts',(20.9714285714286,-7.47210225483002,-8.77932013036538));
#15932=CARTESIAN_POINT('Ctrl Pts',(21.1857142857143,-9.58605112741501,-9.26181516572732));
#15933=CARTESIAN_POINT('Ctrl Pts',(21.4,-11.7,-9.74431020108924));
#15934=CARTESIAN_POINT('Ctrl Pts',(21.6142857142857,-13.813948872585,-9.26181516572731));
#15935=CARTESIAN_POINT('Ctrl Pts',(21.8285714285714,-15.92789774517,-8.77932013036537));
#15936=CARTESIAN_POINT('Ctrl Pts',(22.0428571428571,-17.6231531176579,-7.42739908344628));
#15937=CARTESIAN_POINT('Ctrl Pts',(22.2571428571429,-19.3184084901459,-6.07547803652717));
#15938=CARTESIAN_POINT('Ctrl Pts',(22.4714285714286,-20.259204245073,-4.12189552161681));
#15939=CARTESIAN_POINT('Ctrl Pts',(22.6857142857143,-21.2,-2.16831300670643));
#15940=CARTESIAN_POINT('Ctrl Pts',(22.9,-21.2,-1.04083408558608E-14));
#15941=CARTESIAN_POINT('Ctrl Pts',(23.1142857142857,-21.2,2.16831300670641));
#15942=CARTESIAN_POINT('Ctrl Pts',(23.3285714285714,-20.259204245073,4.1218955216168));
#15943=CARTESIAN_POINT('Ctrl Pts',(23.5428571428571,-19.3184084901459,6.07547803652717));
#15944=CARTESIAN_POINT('Ctrl Pts',(23.7571428571429,-17.623153117658,7.42739908344627));
#15945=CARTESIAN_POINT('Ctrl Pts',(23.9714285714286,-15.92789774517,8.77932013036537));
#15946=CARTESIAN_POINT('Ctrl Pts',(24.1857142857143,-13.813948872585,9.26181516572731));
#15947=CARTESIAN_POINT('Ctrl Pts',(24.4,-11.7,9.74431020108925));
#15948=CARTESIAN_POINT('Ctrl Pts',(24.6142857142857,-9.58605112741501,9.26181516572731));
#15949=CARTESIAN_POINT('Ctrl Pts',(24.8285714285714,-7.47210225483001,8.77932013036537));
#15950=CARTESIAN_POINT('Ctrl Pts',(25.0428571428571,-5.77684688234203,7.42739908344628));
#15951=CARTESIAN_POINT('Ctrl Pts',(25.2571428571429,-4.08159150985402,6.07547803652716));
#15952=CARTESIAN_POINT('Ctrl Pts',(25.4714285714286,-3.14079575492702,4.1218955216168));
#15953=CARTESIAN_POINT('Ctrl Pts',(25.6857142857143,-2.2,2.16831300670643));
#15954=CARTESIAN_POINT('Ctrl Pts',(25.9,-2.20000000000001,-1.38777878078145E-14));
#15955=CARTESIAN_POINT('Ctrl Pts',(0.970493990364278,1.5411253090549,-1.38777878078145E-14));
#15956=CARTESIAN_POINT('Ctrl Pts',(1.18477970464999,1.54112530905491,-3.02220044537403));
#15957=CARTESIAN_POINT('Ctrl Pts',(1.39906541893571,0.229841679453259,-5.74510895921686));
#15958=CARTESIAN_POINT('Ctrl Pts',(1.61335113322142,-1.08144195014838,-8.4680174730597));
#15959=CARTESIAN_POINT('Ctrl Pts',(1.82763684750713,-3.44429340467071,-10.3523286299233));
#15960=CARTESIAN_POINT('Ctrl Pts',(2.04192256179285,-5.80714485919301,-12.236639786787));
#15961=CARTESIAN_POINT('Ctrl Pts',(2.25620827607856,-8.75357242959651,-12.9091426524948));
#15962=CARTESIAN_POINT('Ctrl Pts',(2.47049399036428,-11.7,-13.5816455182026));
#15963=CARTESIAN_POINT('Ctrl Pts',(2.68477970464999,-14.6464275704035,-12.9091426524948));
#15964=CARTESIAN_POINT('Ctrl Pts',(2.89906541893571,-17.592855140807,-12.236639786787));
#15965=CARTESIAN_POINT('Ctrl Pts',(3.11335113322142,-19.9557065953293,-10.3523286299233));
#15966=CARTESIAN_POINT('Ctrl Pts',(3.32763684750713,-22.3185580498516,-8.4680174730597));
#15967=CARTESIAN_POINT('Ctrl Pts',(3.54192256179285,-23.6298416794532,-5.74510895921686));
#15968=CARTESIAN_POINT('Ctrl Pts',(3.75620827607856,-24.9411253090549,-3.02220044537403));
#15969=CARTESIAN_POINT('Ctrl Pts',(3.97049399036428,-24.9411253090549,3.46944695195361E-15));
#15970=CARTESIAN_POINT('Ctrl Pts',(4.18477970464999,-24.9411253090549,3.02220044537403));
#15971=CARTESIAN_POINT('Ctrl Pts',(4.39906541893571,-23.6298416794532,5.74510895921686));
#15972=CARTESIAN_POINT('Ctrl Pts',(4.61335113322142,-22.3185580498516,8.46801747305969));
#15973=CARTESIAN_POINT('Ctrl Pts',(4.82763684750714,-19.9557065953293,10.3523286299233));
#15974=CARTESIAN_POINT('Ctrl Pts',(5.04192256179285,-17.592855140807,12.2366397867869));
#15975=CARTESIAN_POINT('Ctrl Pts',(5.25620827607856,-14.6464275704035,12.9091426524948));
#15976=CARTESIAN_POINT('Ctrl Pts',(5.47049399036428,-11.7,13.5816455182026));
#15977=CARTESIAN_POINT('Ctrl Pts',(5.68477970464999,-8.75357242959651,12.9091426524948));
#15978=CARTESIAN_POINT('Ctrl Pts',(5.89906541893571,-5.80714485919302,12.236639786787));
#15979=CARTESIAN_POINT('Ctrl Pts',(6.11335113322142,-3.4442934046707,10.3523286299233));
#15980=CARTESIAN_POINT('Ctrl Pts',(6.32763684750713,-1.08144195014838,8.4680174730597));
#15981=CARTESIAN_POINT('Ctrl Pts',(6.54192256179285,0.229841679453252,5.74510895921686));
#15982=CARTESIAN_POINT('Ctrl Pts',(6.75620827607856,1.5411253090549,3.02220044537404));
#15983=CARTESIAN_POINT('Ctrl Pts',(6.97049399036428,1.5411253090549,-1.38777878078145E-14));
#15984=CARTESIAN_POINT('Ctrl Pts',(7.18477970464999,1.5411253090549,-3.02220044537404));
#15985=CARTESIAN_POINT('Ctrl Pts',(7.39906541893571,0.229841679453259,-5.74510895921689));
#15986=CARTESIAN_POINT('Ctrl Pts',(7.61335113322142,-1.08144195014838,-8.46801747305971));
#15987=CARTESIAN_POINT('Ctrl Pts',(7.82763684750713,-3.4442934046707,-10.3523286299233));
#15988=CARTESIAN_POINT('Ctrl Pts',(8.04192256179285,-5.80714485919302,-12.236639786787));
#15989=CARTESIAN_POINT('Ctrl Pts',(8.25620827607856,-8.75357242959651,-12.9091426524948));
#15990=CARTESIAN_POINT('Ctrl Pts',(8.47049399036428,-11.7,-13.5816455182026));
#15991=CARTESIAN_POINT('Ctrl Pts',(8.68477970464999,-14.6464275704035,-12.9091426524948));
#15992=CARTESIAN_POINT('Ctrl Pts',(8.89906541893571,-17.592855140807,-12.236639786787));
#15993=CARTESIAN_POINT('Ctrl Pts',(9.11335113322142,-19.9557065953293,-10.3523286299233));
#15994=CARTESIAN_POINT('Ctrl Pts',(9.32763684750714,-22.3185580498516,-8.4680174730597));
#15995=CARTESIAN_POINT('Ctrl Pts',(9.54192256179285,-23.6298416794532,-5.74510895921687));
#15996=CARTESIAN_POINT('Ctrl Pts',(9.75620827607856,-24.9411253090549,-3.02220044537404));
#15997=CARTESIAN_POINT('Ctrl Pts',(9.97049399036428,-24.9411253090549,-6.93889390390723E-15));
#15998=CARTESIAN_POINT('Ctrl Pts',(10.18477970465,-24.9411253090549,3.02220044537403));
#15999=CARTESIAN_POINT('Ctrl Pts',(10.3990654189357,-23.6298416794532,5.74510895921686));
#16000=CARTESIAN_POINT('Ctrl Pts',(10.6133511332214,-22.3185580498516,8.4680174730597));
#16001=CARTESIAN_POINT('Ctrl Pts',(10.8276368475071,-19.9557065953293,10.3523286299233));
#16002=CARTESIAN_POINT('Ctrl Pts',(11.0419225617928,-17.592855140807,12.236639786787));
#16003=CARTESIAN_POINT('Ctrl Pts',(11.2562082760786,-14.6464275704035,12.9091426524948));
#16004=CARTESIAN_POINT('Ctrl Pts',(11.4704939903643,-11.7,13.5816455182026));
#16005=CARTESIAN_POINT('Ctrl Pts',(11.68477970465,-8.75357242959651,12.9091426524948));
#16006=CARTESIAN_POINT('Ctrl Pts',(11.8990654189357,-5.80714485919301,12.236639786787));
#16007=CARTESIAN_POINT('Ctrl Pts',(12.1133511332214,-3.4442934046707,10.3523286299233));
#16008=CARTESIAN_POINT('Ctrl Pts',(12.3276368475071,-1.08144195014836,8.4680174730597));
#16009=CARTESIAN_POINT('Ctrl Pts',(12.5419225617929,0.229841679453266,5.74510895921686));
#16010=CARTESIAN_POINT('Ctrl Pts',(12.7562082760786,1.5411253090549,3.02220044537403));
#16011=CARTESIAN_POINT('Ctrl Pts',(12.9704939903643,1.5411253090549,-2.08166817117217E-14));
#16012=CARTESIAN_POINT('Ctrl Pts',(13.18477970465,1.5411253090549,-3.02220044537405));
#16013=CARTESIAN_POINT('Ctrl Pts',(13.3990654189357,0.229841679453252,-5.74510895921687));
#16014=CARTESIAN_POINT('Ctrl Pts',(13.6133511332214,-1.08144195014838,-8.46801747305971));
#16015=CARTESIAN_POINT('Ctrl Pts',(13.8276368475071,-3.44429340467069,-10.3523286299233));
#16016=CARTESIAN_POINT('Ctrl Pts',(14.0419225617929,-5.80714485919301,-12.236639786787));
#16017=CARTESIAN_POINT('Ctrl Pts',(14.2562082760786,-8.75357242959651,-12.9091426524948));
#16018=CARTESIAN_POINT('Ctrl Pts',(14.4704939903643,-11.7,-13.5816455182026));
#16019=CARTESIAN_POINT('Ctrl Pts',(14.68477970465,-14.6464275704035,-12.9091426524948));
#16020=CARTESIAN_POINT('Ctrl Pts',(14.8990654189357,-17.592855140807,-12.236639786787));
#16021=CARTESIAN_POINT('Ctrl Pts',(15.1133511332214,-19.9557065953293,-10.3523286299233));
#16022=CARTESIAN_POINT('Ctrl Pts',(15.3276368475071,-22.3185580498516,-8.46801747305969));
#16023=CARTESIAN_POINT('Ctrl Pts',(15.5419225617929,-23.6298416794532,-5.74510895921687));
#16024=CARTESIAN_POINT('Ctrl Pts',(15.7562082760786,-24.9411253090549,-3.02220044537403));
#16025=CARTESIAN_POINT('Ctrl Pts',(15.9704939903643,-24.9411253090549,-6.93889390390723E-15));
#16026=CARTESIAN_POINT('Ctrl Pts',(16.18477970465,-24.9411253090549,3.02220044537403));
#16027=CARTESIAN_POINT('Ctrl Pts',(16.3990654189357,-23.6298416794532,5.74510895921686));
#16028=CARTESIAN_POINT('Ctrl Pts',(16.6133511332214,-22.3185580498516,8.46801747305969));
#16029=CARTESIAN_POINT('Ctrl Pts',(16.8276368475071,-19.9557065953293,10.3523286299233));
#16030=CARTESIAN_POINT('Ctrl Pts',(17.0419225617928,-17.592855140807,12.236639786787));
#16031=CARTESIAN_POINT('Ctrl Pts',(17.2562082760786,-14.6464275704035,12.9091426524948));
#16032=CARTESIAN_POINT('Ctrl Pts',(17.4704939903643,-11.7,13.5816455182026));
#16033=CARTESIAN_POINT('Ctrl Pts',(17.68477970465,-8.75357242959651,12.9091426524948));
#16034=CARTESIAN_POINT('Ctrl Pts',(17.8990654189357,-5.80714485919301,12.236639786787));
#16035=CARTESIAN_POINT('Ctrl Pts',(18.1133511332214,-3.4442934046707,10.3523286299233));
#16036=CARTESIAN_POINT('Ctrl Pts',(18.3276368475071,-1.08144195014837,8.46801747305969));
#16037=CARTESIAN_POINT('Ctrl Pts',(18.5419225617928,0.229841679453252,5.74510895921686));
#16038=CARTESIAN_POINT('Ctrl Pts',(18.7562082760786,1.5411253090549,3.02220044537405));
#16039=CARTESIAN_POINT('Ctrl Pts',(18.9704939903643,1.5411253090549,-1.38777878078145E-14));
#16040=CARTESIAN_POINT('Ctrl Pts',(19.18477970465,1.5411253090549,-3.02220044537404));
#16041=CARTESIAN_POINT('Ctrl Pts',(19.3990654189357,0.229841679453259,-5.74510895921686));
#16042=CARTESIAN_POINT('Ctrl Pts',(19.6133511332214,-1.08144195014838,-8.4680174730597));
#16043=CARTESIAN_POINT('Ctrl Pts',(19.8276368475071,-3.4442934046707,-10.3523286299233));
#16044=CARTESIAN_POINT('Ctrl Pts',(20.0419225617929,-5.80714485919302,-12.236639786787));
#16045=CARTESIAN_POINT('Ctrl Pts',(20.2562082760786,-8.75357242959651,-12.9091426524948));
#16046=CARTESIAN_POINT('Ctrl Pts',(20.4704939903643,-11.7,-13.5816455182026));
#16047=CARTESIAN_POINT('Ctrl Pts',(20.68477970465,-14.6464275704035,-12.9091426524948));
#16048=CARTESIAN_POINT('Ctrl Pts',(20.8990654189357,-17.592855140807,-12.236639786787));
#16049=CARTESIAN_POINT('Ctrl Pts',(21.1133511332214,-19.9557065953293,-10.3523286299233));
#16050=CARTESIAN_POINT('Ctrl Pts',(21.3276368475071,-22.3185580498516,-8.4680174730597));
#16051=CARTESIAN_POINT('Ctrl Pts',(21.5419225617929,-23.6298416794532,-5.74510895921687));
#16052=CARTESIAN_POINT('Ctrl Pts',(21.7562082760786,-24.9411253090549,-3.02220044537404));
#16053=CARTESIAN_POINT('Ctrl Pts',(21.9704939903643,-24.9411253090549,-3.46944695195361E-15));
#16054=CARTESIAN_POINT('Ctrl Pts',(22.18477970465,-24.9411253090549,3.02220044537403));
#16055=CARTESIAN_POINT('Ctrl Pts',(22.3990654189357,-23.6298416794532,5.74510895921686));
#16056=CARTESIAN_POINT('Ctrl Pts',(22.6133511332214,-22.3185580498516,8.46801747305969));
#16057=CARTESIAN_POINT('Ctrl Pts',(22.8276368475071,-19.9557065953293,10.3523286299233));
#16058=CARTESIAN_POINT('Ctrl Pts',(23.0419225617928,-17.592855140807,12.236639786787));
#16059=CARTESIAN_POINT('Ctrl Pts',(23.2562082760786,-14.6464275704035,12.9091426524948));
#16060=CARTESIAN_POINT('Ctrl Pts',(23.4704939903643,-11.7,13.5816455182026));
#16061=CARTESIAN_POINT('Ctrl Pts',(23.68477970465,-8.75357242959651,12.9091426524948));
#16062=CARTESIAN_POINT('Ctrl Pts',(23.8990654189357,-5.80714485919302,12.236639786787));
#16063=CARTESIAN_POINT('Ctrl Pts',(24.1133511332214,-3.4442934046707,10.3523286299233));
#16064=CARTESIAN_POINT('Ctrl Pts',(24.3276368475071,-1.08144195014837,8.46801747305969));
#16065=CARTESIAN_POINT('Ctrl Pts',(24.5419225617928,0.229841679453252,5.74510895921686));
#16066=CARTESIAN_POINT('Ctrl Pts',(24.7562082760786,1.5411253090549,3.02220044537404));
#16067=CARTESIAN_POINT('Ctrl Pts',(24.9704939903643,1.5411253090549,0.));
#16068=CARTESIAN_POINT('',(1.43524699518214,-0.329437345472555,-3.46944695195361E-15));
#16069=CARTESIAN_POINT('Origin',(-24.,2.30000000000001,3.46944695195361E-15));
#16070=CARTESIAN_POINT('',(-23.0295060096357,1.5411253090549,0.));
#16071=CARTESIAN_POINT('',(-22.5647530048179,-0.329437345472555,-6.93889390390723E-15));
#16072=CARTESIAN_POINT('',(-24.9704939903643,1.5411253090549,0.));
#16073=CARTESIAN_POINT('Origin',(-24.,1.3,-6.93889390390723E-15));
#16074=CARTESIAN_POINT('',(-25.4352469951821,-0.329437345472555,-1.38777878078145E-14));
#16075=CARTESIAN_POINT('Ctrl Pts',(-0.97049399036428,1.5411253090549,-6.93889390390723E-15));
#16076=CARTESIAN_POINT('Ctrl Pts',(-1.18477970465,1.5411253090549,3.02220044537404));
#16077=CARTESIAN_POINT('Ctrl Pts',(-1.39906541893571,0.229841679453259,
5.74510895921686));
#16078=CARTESIAN_POINT('Ctrl Pts',(-1.61335113322143,-1.08144195014837,
8.46801747305969));
#16079=CARTESIAN_POINT('Ctrl Pts',(-1.82763684750714,-3.4442934046707,10.3523286299233));
#16080=CARTESIAN_POINT('Ctrl Pts',(-2.04192256179286,-5.80714485919302,
12.236639786787));
#16081=CARTESIAN_POINT('Ctrl Pts',(-2.25620827607857,-8.75357242959651,
12.9091426524948));
#16082=CARTESIAN_POINT('Ctrl Pts',(-2.47049399036428,-11.7,13.5816455182026));
#16083=CARTESIAN_POINT('Ctrl Pts',(-2.68477970464999,-14.6464275704035,
12.9091426524948));
#16084=CARTESIAN_POINT('Ctrl Pts',(-2.89906541893571,-17.592855140807,12.236639786787));
#16085=CARTESIAN_POINT('Ctrl Pts',(-3.11335113322142,-19.9557065953293,
10.3523286299233));
#16086=CARTESIAN_POINT('Ctrl Pts',(-3.32763684750714,-22.3185580498516,
8.46801747305969));
#16087=CARTESIAN_POINT('Ctrl Pts',(-3.54192256179285,-23.6298416794532,
5.74510895921685));
#16088=CARTESIAN_POINT('Ctrl Pts',(-3.75620827607857,-24.9411253090549,
3.02220044537403));
#16089=CARTESIAN_POINT('Ctrl Pts',(-3.97049399036429,-24.9411253090549,
-6.93889390390723E-15));
#16090=CARTESIAN_POINT('Ctrl Pts',(-4.18477970464999,-24.9411253090549,
-3.02220044537404));
#16091=CARTESIAN_POINT('Ctrl Pts',(-4.39906541893571,-23.6298416794532,
-5.74510895921685));
#16092=CARTESIAN_POINT('Ctrl Pts',(-4.61335113322143,-22.3185580498516,
-8.46801747305969));
#16093=CARTESIAN_POINT('Ctrl Pts',(-4.82763684750714,-19.9557065953293,
-10.3523286299233));
#16094=CARTESIAN_POINT('Ctrl Pts',(-5.04192256179286,-17.592855140807,-12.236639786787));
#16095=CARTESIAN_POINT('Ctrl Pts',(-5.25620827607857,-14.6464275704035,
-12.9091426524948));
#16096=CARTESIAN_POINT('Ctrl Pts',(-5.47049399036429,-11.7,-13.5816455182026));
#16097=CARTESIAN_POINT('Ctrl Pts',(-5.68477970464999,-8.75357242959651,
-12.9091426524948));
#16098=CARTESIAN_POINT('Ctrl Pts',(-5.89906541893571,-5.80714485919302,
-12.236639786787));
#16099=CARTESIAN_POINT('Ctrl Pts',(-6.11335113322142,-3.4442934046707,-10.3523286299233));
#16100=CARTESIAN_POINT('Ctrl Pts',(-6.32763684750714,-1.08144195014838,
-8.46801747305971));
#16101=CARTESIAN_POINT('Ctrl Pts',(-6.54192256179285,0.229841679453252,
-5.74510895921688));
#16102=CARTESIAN_POINT('Ctrl Pts',(-6.75620827607857,1.5411253090549,-3.02220044537405));
#16103=CARTESIAN_POINT('Ctrl Pts',(-6.97049399036428,1.54112530905488,-6.93889390390723E-15));
#16104=CARTESIAN_POINT('Ctrl Pts',(-7.18477970465,1.5411253090549,3.02220044537401));
#16105=CARTESIAN_POINT('Ctrl Pts',(-7.39906541893571,0.229841679453252,
5.74510895921687));
#16106=CARTESIAN_POINT('Ctrl Pts',(-7.61335113322142,-1.08144195014837,
8.4680174730597));
#16107=CARTESIAN_POINT('Ctrl Pts',(-7.82763684750714,-3.4442934046707,10.3523286299233));
#16108=CARTESIAN_POINT('Ctrl Pts',(-8.04192256179286,-5.80714485919302,
12.236639786787));
#16109=CARTESIAN_POINT('Ctrl Pts',(-8.25620827607856,-8.75357242959651,
12.9091426524948));
#16110=CARTESIAN_POINT('Ctrl Pts',(-8.47049399036428,-11.7,13.5816455182026));
#16111=CARTESIAN_POINT('Ctrl Pts',(-8.68477970464999,-14.6464275704035,
12.9091426524948));
#16112=CARTESIAN_POINT('Ctrl Pts',(-8.89906541893571,-17.592855140807,12.236639786787));
#16113=CARTESIAN_POINT('Ctrl Pts',(-9.11335113322142,-19.9557065953293,
10.3523286299233));
#16114=CARTESIAN_POINT('Ctrl Pts',(-9.32763684750714,-22.3185580498516,
8.4680174730597));
#16115=CARTESIAN_POINT('Ctrl Pts',(-9.54192256179285,-23.6298416794532,
5.74510895921686));
#16116=CARTESIAN_POINT('Ctrl Pts',(-9.75620827607857,-24.9411253090549,
3.02220044537403));
#16117=CARTESIAN_POINT('Ctrl Pts',(-9.97049399036428,-24.9411253090549,
-6.93889390390723E-15));
#16118=CARTESIAN_POINT('Ctrl Pts',(-10.18477970465,-24.9411253090549,-3.02220044537404));
#16119=CARTESIAN_POINT('Ctrl Pts',(-10.3990654189357,-23.6298416794532,
-5.74510895921686));
#16120=CARTESIAN_POINT('Ctrl Pts',(-10.6133511332214,-22.3185580498516,
-8.46801747305971));
#16121=CARTESIAN_POINT('Ctrl Pts',(-10.8276368475071,-19.9557065953293,
-10.3523286299233));
#16122=CARTESIAN_POINT('Ctrl Pts',(-11.0419225617928,-17.5928551408069,
-12.236639786787));
#16123=CARTESIAN_POINT('Ctrl Pts',(-11.2562082760786,-14.6464275704035,
-12.9091426524948));
#16124=CARTESIAN_POINT('Ctrl Pts',(-11.4704939903643,-11.7,-13.5816455182026));
#16125=CARTESIAN_POINT('Ctrl Pts',(-11.68477970465,-8.75357242959649,-12.9091426524948));
#16126=CARTESIAN_POINT('Ctrl Pts',(-11.8990654189357,-5.80714485919302,
-12.236639786787));
#16127=CARTESIAN_POINT('Ctrl Pts',(-12.1133511332214,-3.44429340467069,
-10.3523286299234));
#16128=CARTESIAN_POINT('Ctrl Pts',(-12.3276368475071,-1.08144195014838,
-8.46801747305969));
#16129=CARTESIAN_POINT('Ctrl Pts',(-12.5419225617929,0.229841679453252,
-5.74510895921687));
#16130=CARTESIAN_POINT('Ctrl Pts',(-12.7562082760786,1.54112530905491,-3.02220044537405));
#16131=CARTESIAN_POINT('Ctrl Pts',(-12.9704939903643,1.5411253090549,0.));
#16132=CARTESIAN_POINT('Ctrl Pts',(-13.18477970465,1.5411253090549,3.02220044537401));
#16133=CARTESIAN_POINT('Ctrl Pts',(-13.3990654189357,0.229841679453252,
5.74510895921686));
#16134=CARTESIAN_POINT('Ctrl Pts',(-13.6133511332214,-1.08144195014837,
8.46801747305969));
#16135=CARTESIAN_POINT('Ctrl Pts',(-13.8276368475071,-3.4442934046707,10.3523286299233));
#16136=CARTESIAN_POINT('Ctrl Pts',(-14.0419225617929,-5.80714485919302,
12.236639786787));
#16137=CARTESIAN_POINT('Ctrl Pts',(-14.2562082760786,-8.75357242959651,
12.9091426524948));
#16138=CARTESIAN_POINT('Ctrl Pts',(-14.4704939903643,-11.7,13.5816455182026));
#16139=CARTESIAN_POINT('Ctrl Pts',(-14.68477970465,-14.6464275704035,12.9091426524948));
#16140=CARTESIAN_POINT('Ctrl Pts',(-14.8990654189357,-17.5928551408069,
12.236639786787));
#16141=CARTESIAN_POINT('Ctrl Pts',(-15.1133511332214,-19.9557065953293,
10.3523286299233));
#16142=CARTESIAN_POINT('Ctrl Pts',(-15.3276368475071,-22.3185580498516,
8.46801747305968));
#16143=CARTESIAN_POINT('Ctrl Pts',(-15.5419225617929,-23.6298416794532,
5.74510895921686));
#16144=CARTESIAN_POINT('Ctrl Pts',(-15.7562082760786,-24.9411253090549,
3.02220044537403));
#16145=CARTESIAN_POINT('Ctrl Pts',(-15.9704939903643,-24.9411253090549,
0.));
#16146=CARTESIAN_POINT('Ctrl Pts',(-16.18477970465,-24.9411253090549,-3.02220044537402));
#16147=CARTESIAN_POINT('Ctrl Pts',(-16.3990654189357,-23.6298416794532,
-5.74510895921687));
#16148=CARTESIAN_POINT('Ctrl Pts',(-16.6133511332214,-22.3185580498516,
-8.4680174730597));
#16149=CARTESIAN_POINT('Ctrl Pts',(-16.8276368475071,-19.9557065953293,
-10.3523286299233));
#16150=CARTESIAN_POINT('Ctrl Pts',(-17.0419225617929,-17.5928551408069,
-12.236639786787));
#16151=CARTESIAN_POINT('Ctrl Pts',(-17.2562082760786,-14.6464275704035,
-12.9091426524948));
#16152=CARTESIAN_POINT('Ctrl Pts',(-17.4704939903643,-11.7,-13.5816455182026));
#16153=CARTESIAN_POINT('Ctrl Pts',(-17.68477970465,-8.75357242959651,-12.9091426524948));
#16154=CARTESIAN_POINT('Ctrl Pts',(-17.8990654189357,-5.80714485919301,
-12.236639786787));
#16155=CARTESIAN_POINT('Ctrl Pts',(-18.1133511332214,-3.4442934046707,-10.3523286299233));
#16156=CARTESIAN_POINT('Ctrl Pts',(-18.3276368475072,-1.08144195014838,
-8.46801747305968));
#16157=CARTESIAN_POINT('Ctrl Pts',(-18.5419225617929,0.229841679453252,
-5.74510895921686));
#16158=CARTESIAN_POINT('Ctrl Pts',(-18.7562082760786,1.5411253090549,-3.02220044537404));
#16159=CARTESIAN_POINT('Ctrl Pts',(-18.9704939903643,1.5411253090549,-3.46944695195361E-15));
#16160=CARTESIAN_POINT('Ctrl Pts',(-19.18477970465,1.5411253090549,3.02220044537403));
#16161=CARTESIAN_POINT('Ctrl Pts',(-19.3990654189357,0.229841679453252,
5.74510895921686));
#16162=CARTESIAN_POINT('Ctrl Pts',(-19.6133511332214,-1.08144195014837,
8.4680174730597));
#16163=CARTESIAN_POINT('Ctrl Pts',(-19.8276368475071,-3.4442934046707,10.3523286299233));
#16164=CARTESIAN_POINT('Ctrl Pts',(-20.0419225617929,-5.80714485919302,
12.236639786787));
#16165=CARTESIAN_POINT('Ctrl Pts',(-20.2562082760786,-8.75357242959651,
12.9091426524948));
#16166=CARTESIAN_POINT('Ctrl Pts',(-20.4704939903643,-11.7,13.5816455182026));
#16167=CARTESIAN_POINT('Ctrl Pts',(-20.68477970465,-14.6464275704035,12.9091426524948));
#16168=CARTESIAN_POINT('Ctrl Pts',(-20.8990654189357,-17.5928551408069,
12.236639786787));
#16169=CARTESIAN_POINT('Ctrl Pts',(-21.1133511332214,-19.9557065953293,
10.3523286299233));
#16170=CARTESIAN_POINT('Ctrl Pts',(-21.3276368475072,-22.3185580498516,
8.4680174730597));
#16171=CARTESIAN_POINT('Ctrl Pts',(-21.5419225617929,-23.6298416794532,
5.74510895921686));
#16172=CARTESIAN_POINT('Ctrl Pts',(-21.7562082760786,-24.9411253090549,
3.02220044537405));
#16173=CARTESIAN_POINT('Ctrl Pts',(-21.9704939903643,-24.9411253090549,
3.46944695195361E-15));
#16174=CARTESIAN_POINT('Ctrl Pts',(-22.18477970465,-24.9411253090549,-3.02220044537404));
#16175=CARTESIAN_POINT('Ctrl Pts',(-22.3990654189357,-23.6298416794532,
-5.74510895921686));
#16176=CARTESIAN_POINT('Ctrl Pts',(-22.6133511332214,-22.3185580498516,
-8.4680174730597));
#16177=CARTESIAN_POINT('Ctrl Pts',(-22.8276368475072,-19.9557065953293,
-10.3523286299233));
#16178=CARTESIAN_POINT('Ctrl Pts',(-23.0419225617929,-17.592855140807,-12.236639786787));
#16179=CARTESIAN_POINT('Ctrl Pts',(-23.2562082760786,-14.6464275704035,
-12.9091426524948));
#16180=CARTESIAN_POINT('Ctrl Pts',(-23.4704939903643,-11.7,-13.5816455182026));
#16181=CARTESIAN_POINT('Ctrl Pts',(-23.68477970465,-8.75357242959651,-12.9091426524948));
#16182=CARTESIAN_POINT('Ctrl Pts',(-23.8990654189357,-5.80714485919301,
-12.236639786787));
#16183=CARTESIAN_POINT('Ctrl Pts',(-24.1133511332214,-3.4442934046707,-10.3523286299233));
#16184=CARTESIAN_POINT('Ctrl Pts',(-24.3276368475071,-1.08144195014838,
-8.46801747305971));
#16185=CARTESIAN_POINT('Ctrl Pts',(-24.5419225617929,0.229841679453259,
-5.74510895921687));
#16186=CARTESIAN_POINT('Ctrl Pts',(-24.7562082760786,1.54112530905491,-3.02220044537405));
#16187=CARTESIAN_POINT('Ctrl Pts',(-24.9704939903643,1.5411253090549,0.));
#16188=CARTESIAN_POINT('Ctrl Pts',(-1.9,-2.2,0.));
#16189=CARTESIAN_POINT('Ctrl Pts',(-2.11428571428572,-2.19999999999999,
2.16831300670641));
#16190=CARTESIAN_POINT('Ctrl Pts',(-2.32857142857143,-3.14079575492701,
4.1218955216168));
#16191=CARTESIAN_POINT('Ctrl Pts',(-2.54285714285714,-4.08159150985402,
6.07547803652717));
#16192=CARTESIAN_POINT('Ctrl Pts',(-2.75714285714286,-5.77684688234203,
7.42739908344627));
#16193=CARTESIAN_POINT('Ctrl Pts',(-2.97142857142857,-7.47210225483002,
8.77932013036537));
#16194=CARTESIAN_POINT('Ctrl Pts',(-3.18571428571429,-9.58605112741499,
9.2618151657273));
#16195=CARTESIAN_POINT('Ctrl Pts',(-3.4,-11.7,9.74431020108924));
#16196=CARTESIAN_POINT('Ctrl Pts',(-3.61428571428572,-13.813948872585,9.26181516572731));
#16197=CARTESIAN_POINT('Ctrl Pts',(-3.82857142857143,-15.92789774517,8.77932013036537));
#16198=CARTESIAN_POINT('Ctrl Pts',(-4.04285714285715,-17.623153117658,7.42739908344628));
#16199=CARTESIAN_POINT('Ctrl Pts',(-4.25714285714286,-19.318408490146,6.07547803652718));
#16200=CARTESIAN_POINT('Ctrl Pts',(-4.47142857142857,-20.259204245073,4.1218955216168));
#16201=CARTESIAN_POINT('Ctrl Pts',(-4.68571428571429,-21.2,2.16831300670642));
#16202=CARTESIAN_POINT('Ctrl Pts',(-4.9,-21.2,-1.04083408558608E-14));
#16203=CARTESIAN_POINT('Ctrl Pts',(-5.11428571428572,-21.2,-2.16831300670643));
#16204=CARTESIAN_POINT('Ctrl Pts',(-5.32857142857143,-20.259204245073,-4.1218955216168));
#16205=CARTESIAN_POINT('Ctrl Pts',(-5.54285714285714,-19.318408490146,-6.07547803652718));
#16206=CARTESIAN_POINT('Ctrl Pts',(-5.75714285714286,-17.623153117658,-7.42739908344628));
#16207=CARTESIAN_POINT('Ctrl Pts',(-5.97142857142858,-15.92789774517,-8.7793201303654));
#16208=CARTESIAN_POINT('Ctrl Pts',(-6.18571428571429,-13.813948872585,-9.26181516572732));
#16209=CARTESIAN_POINT('Ctrl Pts',(-6.4,-11.7,-9.74431020108927));
#16210=CARTESIAN_POINT('Ctrl Pts',(-6.61428571428572,-9.58605112741499,
-9.26181516572733));
#16211=CARTESIAN_POINT('Ctrl Pts',(-6.82857142857144,-7.47210225483002,
-8.77932013036538));
#16212=CARTESIAN_POINT('Ctrl Pts',(-7.04285714285714,-5.77684688234203,
-7.42739908344628));
#16213=CARTESIAN_POINT('Ctrl Pts',(-7.25714285714286,-4.08159150985404,
-6.07547803652718));
#16214=CARTESIAN_POINT('Ctrl Pts',(-7.47142857142857,-3.14079575492701,
-4.12189552161681));
#16215=CARTESIAN_POINT('Ctrl Pts',(-7.68571428571429,-2.2,-2.16831300670643));
#16216=CARTESIAN_POINT('Ctrl Pts',(-7.9,-2.2,-3.46944695195361E-15));
#16217=CARTESIAN_POINT('Ctrl Pts',(-8.11428571428572,-2.20000000000001,
2.16831300670642));
#16218=CARTESIAN_POINT('Ctrl Pts',(-8.32857142857143,-3.14079575492702,
4.12189552161678));
#16219=CARTESIAN_POINT('Ctrl Pts',(-8.54285714285714,-4.08159150985404,
6.07547803652716));
#16220=CARTESIAN_POINT('Ctrl Pts',(-8.75714285714286,-5.77684688234202,
7.42739908344627));
#16221=CARTESIAN_POINT('Ctrl Pts',(-8.97142857142857,-7.47210225483001,
8.77932013036537));
#16222=CARTESIAN_POINT('Ctrl Pts',(-9.18571428571429,-9.58605112741501,
9.26181516572731));
#16223=CARTESIAN_POINT('Ctrl Pts',(-9.4,-11.7,9.74431020108925));
#16224=CARTESIAN_POINT('Ctrl Pts',(-9.61428571428571,-13.813948872585,9.26181516572731));
#16225=CARTESIAN_POINT('Ctrl Pts',(-9.82857142857143,-15.92789774517,8.77932013036538));
#16226=CARTESIAN_POINT('Ctrl Pts',(-10.0428571428572,-17.6231531176579,
7.42739908344626));
#16227=CARTESIAN_POINT('Ctrl Pts',(-10.2571428571429,-19.3184084901459,
6.07547803652716));
#16228=CARTESIAN_POINT('Ctrl Pts',(-10.4714285714286,-20.259204245073,4.12189552161679));
#16229=CARTESIAN_POINT('Ctrl Pts',(-10.6857142857143,-21.2,2.16831300670642));
#16230=CARTESIAN_POINT('Ctrl Pts',(-10.9,-21.2,-6.93889390390723E-15));
#16231=CARTESIAN_POINT('Ctrl Pts',(-11.1142857142857,-21.2,-2.16831300670643));
#16232=CARTESIAN_POINT('Ctrl Pts',(-11.3285714285714,-20.259204245073,-4.12189552161681));
#16233=CARTESIAN_POINT('Ctrl Pts',(-11.5428571428571,-19.3184084901459,
-6.07547803652717));
#16234=CARTESIAN_POINT('Ctrl Pts',(-11.7571428571429,-17.623153117658,-7.42739908344627));
#16235=CARTESIAN_POINT('Ctrl Pts',(-11.9714285714286,-15.92789774517,-8.77932013036536));
#16236=CARTESIAN_POINT('Ctrl Pts',(-12.1857142857143,-13.813948872585,-9.26181516572733));
#16237=CARTESIAN_POINT('Ctrl Pts',(-12.4,-11.7,-9.74431020108925));
#16238=CARTESIAN_POINT('Ctrl Pts',(-12.6142857142857,-9.58605112741501,
-9.26181516572733));
#16239=CARTESIAN_POINT('Ctrl Pts',(-12.8285714285714,-7.47210225483001,
-8.77932013036539));
#16240=CARTESIAN_POINT('Ctrl Pts',(-13.0428571428571,-5.77684688234202,
-7.4273990834463));
#16241=CARTESIAN_POINT('Ctrl Pts',(-13.2571428571429,-4.08159150985404,
-6.07547803652718));
#16242=CARTESIAN_POINT('Ctrl Pts',(-13.4714285714286,-3.14079575492702,
-4.12189552161681));
#16243=CARTESIAN_POINT('Ctrl Pts',(-13.6857142857143,-2.2,-2.16831300670643));
#16244=CARTESIAN_POINT('Ctrl Pts',(-13.9,-2.2,0.));
#16245=CARTESIAN_POINT('Ctrl Pts',(-14.1142857142857,-2.19999999999999,
2.16831300670641));
#16246=CARTESIAN_POINT('Ctrl Pts',(-14.3285714285714,-3.14079575492702,
4.1218955216168));
#16247=CARTESIAN_POINT('Ctrl Pts',(-14.5428571428571,-4.08159150985404,
6.07547803652717));
#16248=CARTESIAN_POINT('Ctrl Pts',(-14.7571428571429,-5.77684688234203,
7.42739908344626));
#16249=CARTESIAN_POINT('Ctrl Pts',(-14.9714285714286,-7.47210225483001,
8.77932013036538));
#16250=CARTESIAN_POINT('Ctrl Pts',(-15.1857142857143,-9.58605112741501,
9.26181516572731));
#16251=CARTESIAN_POINT('Ctrl Pts',(-15.4,-11.7,9.74431020108925));
#16252=CARTESIAN_POINT('Ctrl Pts',(-15.6142857142857,-13.813948872585,9.26181516572731));
#16253=CARTESIAN_POINT('Ctrl Pts',(-15.8285714285714,-15.92789774517,8.77932013036537));
#16254=CARTESIAN_POINT('Ctrl Pts',(-16.0428571428571,-17.6231531176579,
7.42739908344627));
#16255=CARTESIAN_POINT('Ctrl Pts',(-16.2571428571429,-19.3184084901459,
6.07547803652717));
#16256=CARTESIAN_POINT('Ctrl Pts',(-16.4714285714286,-20.259204245073,4.12189552161679));
#16257=CARTESIAN_POINT('Ctrl Pts',(-16.6857142857143,-21.2,2.16831300670642));
#16258=CARTESIAN_POINT('Ctrl Pts',(-16.9,-21.2,-6.93889390390723E-15));
#16259=CARTESIAN_POINT('Ctrl Pts',(-17.1142857142857,-21.2,-2.16831300670643));
#16260=CARTESIAN_POINT('Ctrl Pts',(-17.3285714285715,-20.259204245073,-4.1218955216168));
#16261=CARTESIAN_POINT('Ctrl Pts',(-17.5428571428572,-19.3184084901459,
-6.07547803652717));
#16262=CARTESIAN_POINT('Ctrl Pts',(-17.7571428571429,-17.623153117658,-7.42739908344627));
#16263=CARTESIAN_POINT('Ctrl Pts',(-17.9714285714286,-15.92789774517,-8.77932013036538));
#16264=CARTESIAN_POINT('Ctrl Pts',(-18.1857142857143,-13.813948872585,-9.26181516572732));
#16265=CARTESIAN_POINT('Ctrl Pts',(-18.4,-11.7,-9.74431020108925));
#16266=CARTESIAN_POINT('Ctrl Pts',(-18.6142857142857,-9.58605112741501,
-9.26181516572731));
#16267=CARTESIAN_POINT('Ctrl Pts',(-18.8285714285714,-7.47210225483001,
-8.77932013036538));
#16268=CARTESIAN_POINT('Ctrl Pts',(-19.0428571428572,-5.77684688234203,
-7.42739908344629));
#16269=CARTESIAN_POINT('Ctrl Pts',(-19.2571428571429,-4.08159150985404,
-6.07547803652718));
#16270=CARTESIAN_POINT('Ctrl Pts',(-19.4714285714286,-3.14079575492701,
-4.1218955216168));
#16271=CARTESIAN_POINT('Ctrl Pts',(-19.6857142857143,-2.2,-2.16831300670644));
#16272=CARTESIAN_POINT('Ctrl Pts',(-19.9,-2.2,-3.46944695195361E-15));
#16273=CARTESIAN_POINT('Ctrl Pts',(-20.1142857142857,-2.19999999999999,
2.16831300670643));
#16274=CARTESIAN_POINT('Ctrl Pts',(-20.3285714285714,-3.14079575492702,
4.1218955216168));
#16275=CARTESIAN_POINT('Ctrl Pts',(-20.5428571428571,-4.08159150985404,
6.07547803652716));
#16276=CARTESIAN_POINT('Ctrl Pts',(-20.7571428571429,-5.77684688234202,
7.42739908344627));
#16277=CARTESIAN_POINT('Ctrl Pts',(-20.9714285714286,-7.47210225483001,
8.77932013036537));
#16278=CARTESIAN_POINT('Ctrl Pts',(-21.1857142857143,-9.58605112741501,
9.2618151657273));
#16279=CARTESIAN_POINT('Ctrl Pts',(-21.4,-11.7,9.74431020108925));
#16280=CARTESIAN_POINT('Ctrl Pts',(-21.6142857142857,-13.813948872585,9.26181516572731));
#16281=CARTESIAN_POINT('Ctrl Pts',(-21.8285714285714,-15.92789774517,8.77932013036537));
#16282=CARTESIAN_POINT('Ctrl Pts',(-22.0428571428571,-17.6231531176579,
7.42739908344627));
#16283=CARTESIAN_POINT('Ctrl Pts',(-22.2571428571429,-19.3184084901459,
6.07547803652717));
#16284=CARTESIAN_POINT('Ctrl Pts',(-22.4714285714286,-20.259204245073,4.1218955216168));
#16285=CARTESIAN_POINT('Ctrl Pts',(-22.6857142857143,-21.2,2.16831300670641));
#16286=CARTESIAN_POINT('Ctrl Pts',(-22.9,-21.2,-6.93889390390723E-15));
#16287=CARTESIAN_POINT('Ctrl Pts',(-23.1142857142857,-21.2,-2.16831300670642));
#16288=CARTESIAN_POINT('Ctrl Pts',(-23.3285714285715,-20.259204245073,-4.1218955216168));
#16289=CARTESIAN_POINT('Ctrl Pts',(-23.5428571428572,-19.318408490146,-6.07547803652718));
#16290=CARTESIAN_POINT('Ctrl Pts',(-23.7571428571429,-17.623153117658,-7.42739908344627));
#16291=CARTESIAN_POINT('Ctrl Pts',(-23.9714285714286,-15.9278977451699,
-8.77932013036538));
#16292=CARTESIAN_POINT('Ctrl Pts',(-24.1857142857143,-13.813948872585,-9.26181516572731));
#16293=CARTESIAN_POINT('Ctrl Pts',(-24.4,-11.7,-9.74431020108925));
#16294=CARTESIAN_POINT('Ctrl Pts',(-24.6142857142857,-9.58605112741501,
-9.26181516572732));
#16295=CARTESIAN_POINT('Ctrl Pts',(-24.8285714285714,-7.47210225483001,
-8.77932013036537));
#16296=CARTESIAN_POINT('Ctrl Pts',(-25.0428571428572,-5.77684688234203,
-7.42739908344628));
#16297=CARTESIAN_POINT('Ctrl Pts',(-25.2571428571429,-4.08159150985402,
-6.07547803652718));
#16298=CARTESIAN_POINT('Ctrl Pts',(-25.4714285714286,-3.14079575492701,
-4.12189552161682));
#16299=CARTESIAN_POINT('Ctrl Pts',(-25.6857142857143,-2.20000000000001,
-2.16831300670643));
#16300=CARTESIAN_POINT('Ctrl Pts',(-25.9,-2.20000000000001,-1.38777878078145E-14));
#16301=CARTESIAN_POINT('Ctrl Pts',(-0.97049399036428,1.5411253090549,-6.93889390390723E-15));
#16302=CARTESIAN_POINT('Ctrl Pts',(-1.18477970465,1.5411253090549,3.02220044537404));
#16303=CARTESIAN_POINT('Ctrl Pts',(-1.39906541893571,0.229841679453259,
5.74510895921686));
#16304=CARTESIAN_POINT('Ctrl Pts',(-1.61335113322143,-1.08144195014837,
8.46801747305969));
#16305=CARTESIAN_POINT('Ctrl Pts',(-1.82763684750714,-3.4442934046707,10.3523286299233));
#16306=CARTESIAN_POINT('Ctrl Pts',(-2.04192256179285,-5.80714485919302,
12.236639786787));
#16307=CARTESIAN_POINT('Ctrl Pts',(-2.25620827607857,-8.75357242959651,
12.9091426524948));
#16308=CARTESIAN_POINT('Ctrl Pts',(-2.47049399036428,-11.7,13.5816455182026));
#16309=CARTESIAN_POINT('Ctrl Pts',(-2.68477970464999,-14.6464275704035,
12.9091426524948));
#16310=CARTESIAN_POINT('Ctrl Pts',(-2.89906541893571,-17.592855140807,12.236639786787));
#16311=CARTESIAN_POINT('Ctrl Pts',(-3.11335113322142,-19.9557065953293,
10.3523286299233));
#16312=CARTESIAN_POINT('Ctrl Pts',(-3.32763684750714,-22.3185580498516,
8.46801747305969));
#16313=CARTESIAN_POINT('Ctrl Pts',(-3.54192256179285,-23.6298416794532,
5.74510895921685));
#16314=CARTESIAN_POINT('Ctrl Pts',(-3.75620827607857,-24.9411253090549,
3.02220044537403));
#16315=CARTESIAN_POINT('Ctrl Pts',(-3.97049399036428,-24.9411253090549,
-6.93889390390723E-15));
#16316=CARTESIAN_POINT('Ctrl Pts',(-4.18477970464999,-24.9411253090549,
-3.02220044537404));
#16317=CARTESIAN_POINT('Ctrl Pts',(-4.39906541893571,-23.6298416794532,
-5.74510895921685));
#16318=CARTESIAN_POINT('Ctrl Pts',(-4.61335113322142,-22.3185580498516,
-8.46801747305969));
#16319=CARTESIAN_POINT('Ctrl Pts',(-4.82763684750714,-19.9557065953293,
-10.3523286299233));
#16320=CARTESIAN_POINT('Ctrl Pts',(-5.04192256179286,-17.592855140807,-12.236639786787));
#16321=CARTESIAN_POINT('Ctrl Pts',(-5.25620827607857,-14.6464275704035,
-12.9091426524948));
#16322=CARTESIAN_POINT('Ctrl Pts',(-5.47049399036429,-11.7,-13.5816455182026));
#16323=CARTESIAN_POINT('Ctrl Pts',(-5.68477970464999,-8.75357242959651,
-12.9091426524948));
#16324=CARTESIAN_POINT('Ctrl Pts',(-5.89906541893571,-5.80714485919302,
-12.236639786787));
#16325=CARTESIAN_POINT('Ctrl Pts',(-6.11335113322142,-3.4442934046707,-10.3523286299233));
#16326=CARTESIAN_POINT('Ctrl Pts',(-6.32763684750714,-1.08144195014838,
-8.46801747305971));
#16327=CARTESIAN_POINT('Ctrl Pts',(-6.54192256179285,0.229841679453252,
-5.74510895921688));
#16328=CARTESIAN_POINT('Ctrl Pts',(-6.75620827607857,1.5411253090549,-3.02220044537405));
#16329=CARTESIAN_POINT('Ctrl Pts',(-6.97049399036428,1.54112530905488,-6.93889390390723E-15));
#16330=CARTESIAN_POINT('Ctrl Pts',(-7.18477970465,1.5411253090549,3.02220044537401));
#16331=CARTESIAN_POINT('Ctrl Pts',(-7.39906541893571,0.229841679453252,
5.74510895921687));
#16332=CARTESIAN_POINT('Ctrl Pts',(-7.61335113322143,-1.08144195014837,
8.4680174730597));
#16333=CARTESIAN_POINT('Ctrl Pts',(-7.82763684750714,-3.4442934046707,10.3523286299233));
#16334=CARTESIAN_POINT('Ctrl Pts',(-8.04192256179286,-5.80714485919302,
12.236639786787));
#16335=CARTESIAN_POINT('Ctrl Pts',(-8.25620827607856,-8.75357242959651,
12.9091426524948));
#16336=CARTESIAN_POINT('Ctrl Pts',(-8.47049399036428,-11.7,13.5816455182026));
#16337=CARTESIAN_POINT('Ctrl Pts',(-8.68477970464999,-14.6464275704035,
12.9091426524948));
#16338=CARTESIAN_POINT('Ctrl Pts',(-8.89906541893571,-17.592855140807,12.236639786787));
#16339=CARTESIAN_POINT('Ctrl Pts',(-9.11335113322142,-19.9557065953293,
10.3523286299233));
#16340=CARTESIAN_POINT('Ctrl Pts',(-9.32763684750714,-22.3185580498516,
8.4680174730597));
#16341=CARTESIAN_POINT('Ctrl Pts',(-9.54192256179285,-23.6298416794532,
5.74510895921686));
#16342=CARTESIAN_POINT('Ctrl Pts',(-9.75620827607857,-24.9411253090549,
3.02220044537403));
#16343=CARTESIAN_POINT('Ctrl Pts',(-9.97049399036428,-24.9411253090549,
-6.93889390390723E-15));
#16344=CARTESIAN_POINT('Ctrl Pts',(-10.18477970465,-24.9411253090549,-3.02220044537404));
#16345=CARTESIAN_POINT('Ctrl Pts',(-10.3990654189357,-23.6298416794532,
-5.74510895921686));
#16346=CARTESIAN_POINT('Ctrl Pts',(-10.6133511332214,-22.3185580498516,
-8.46801747305971));
#16347=CARTESIAN_POINT('Ctrl Pts',(-10.8276368475071,-19.9557065953293,
-10.3523286299233));
#16348=CARTESIAN_POINT('Ctrl Pts',(-11.0419225617928,-17.5928551408069,
-12.236639786787));
#16349=CARTESIAN_POINT('Ctrl Pts',(-11.2562082760786,-14.6464275704035,
-12.9091426524948));
#16350=CARTESIAN_POINT('Ctrl Pts',(-11.4704939903643,-11.7,-13.5816455182026));
#16351=CARTESIAN_POINT('Ctrl Pts',(-11.68477970465,-8.75357242959649,-12.9091426524948));
#16352=CARTESIAN_POINT('Ctrl Pts',(-11.8990654189357,-5.80714485919302,
-12.236639786787));
#16353=CARTESIAN_POINT('Ctrl Pts',(-12.1133511332214,-3.44429340467069,
-10.3523286299234));
#16354=CARTESIAN_POINT('Ctrl Pts',(-12.3276368475071,-1.08144195014838,
-8.46801747305969));
#16355=CARTESIAN_POINT('Ctrl Pts',(-12.5419225617929,0.229841679453252,
-5.74510895921687));
#16356=CARTESIAN_POINT('Ctrl Pts',(-12.7562082760786,1.54112530905491,-3.02220044537405));
#16357=CARTESIAN_POINT('Ctrl Pts',(-12.9704939903643,1.5411253090549,0.));
#16358=CARTESIAN_POINT('Ctrl Pts',(-13.18477970465,1.5411253090549,3.02220044537401));
#16359=CARTESIAN_POINT('Ctrl Pts',(-13.3990654189357,0.229841679453252,
5.74510895921686));
#16360=CARTESIAN_POINT('Ctrl Pts',(-13.6133511332214,-1.08144195014837,
8.46801747305969));
#16361=CARTESIAN_POINT('Ctrl Pts',(-13.8276368475071,-3.4442934046707,10.3523286299233));
#16362=CARTESIAN_POINT('Ctrl Pts',(-14.0419225617929,-5.80714485919302,
12.236639786787));
#16363=CARTESIAN_POINT('Ctrl Pts',(-14.2562082760786,-8.75357242959651,
12.9091426524948));
#16364=CARTESIAN_POINT('Ctrl Pts',(-14.4704939903643,-11.7,13.5816455182026));
#16365=CARTESIAN_POINT('Ctrl Pts',(-14.68477970465,-14.6464275704035,12.9091426524948));
#16366=CARTESIAN_POINT('Ctrl Pts',(-14.8990654189357,-17.5928551408069,
12.236639786787));
#16367=CARTESIAN_POINT('Ctrl Pts',(-15.1133511332214,-19.9557065953293,
10.3523286299233));
#16368=CARTESIAN_POINT('Ctrl Pts',(-15.3276368475071,-22.3185580498516,
8.46801747305968));
#16369=CARTESIAN_POINT('Ctrl Pts',(-15.5419225617929,-23.6298416794532,
5.74510895921686));
#16370=CARTESIAN_POINT('Ctrl Pts',(-15.7562082760786,-24.9411253090549,
3.02220044537403));
#16371=CARTESIAN_POINT('Ctrl Pts',(-15.9704939903643,-24.9411253090549,
0.));
#16372=CARTESIAN_POINT('Ctrl Pts',(-16.18477970465,-24.9411253090549,-3.02220044537402));
#16373=CARTESIAN_POINT('Ctrl Pts',(-16.3990654189357,-23.6298416794532,
-5.74510895921687));
#16374=CARTESIAN_POINT('Ctrl Pts',(-16.6133511332214,-22.3185580498516,
-8.4680174730597));
#16375=CARTESIAN_POINT('Ctrl Pts',(-16.8276368475071,-19.9557065953293,
-10.3523286299233));
#16376=CARTESIAN_POINT('Ctrl Pts',(-17.0419225617929,-17.5928551408069,
-12.236639786787));
#16377=CARTESIAN_POINT('Ctrl Pts',(-17.2562082760786,-14.6464275704035,
-12.9091426524948));
#16378=CARTESIAN_POINT('Ctrl Pts',(-17.4704939903643,-11.7,-13.5816455182026));
#16379=CARTESIAN_POINT('Ctrl Pts',(-17.68477970465,-8.75357242959651,-12.9091426524948));
#16380=CARTESIAN_POINT('Ctrl Pts',(-17.8990654189357,-5.80714485919301,
-12.236639786787));
#16381=CARTESIAN_POINT('Ctrl Pts',(-18.1133511332214,-3.4442934046707,-10.3523286299233));
#16382=CARTESIAN_POINT('Ctrl Pts',(-18.3276368475072,-1.08144195014838,
-8.46801747305968));
#16383=CARTESIAN_POINT('Ctrl Pts',(-18.5419225617929,0.229841679453252,
-5.74510895921686));
#16384=CARTESIAN_POINT('Ctrl Pts',(-18.7562082760786,1.5411253090549,-3.02220044537404));
#16385=CARTESIAN_POINT('Ctrl Pts',(-18.9704939903643,1.5411253090549,-3.46944695195361E-15));
#16386=CARTESIAN_POINT('Ctrl Pts',(-19.18477970465,1.5411253090549,3.02220044537403));
#16387=CARTESIAN_POINT('Ctrl Pts',(-19.3990654189357,0.229841679453252,
5.74510895921686));
#16388=CARTESIAN_POINT('Ctrl Pts',(-19.6133511332214,-1.08144195014837,
8.4680174730597));
#16389=CARTESIAN_POINT('Ctrl Pts',(-19.8276368475071,-3.4442934046707,10.3523286299233));
#16390=CARTESIAN_POINT('Ctrl Pts',(-20.0419225617929,-5.80714485919302,
12.236639786787));
#16391=CARTESIAN_POINT('Ctrl Pts',(-20.2562082760786,-8.75357242959651,
12.9091426524948));
#16392=CARTESIAN_POINT('Ctrl Pts',(-20.4704939903643,-11.7,13.5816455182026));
#16393=CARTESIAN_POINT('Ctrl Pts',(-20.68477970465,-14.6464275704035,12.9091426524948));
#16394=CARTESIAN_POINT('Ctrl Pts',(-20.8990654189357,-17.5928551408069,
12.236639786787));
#16395=CARTESIAN_POINT('Ctrl Pts',(-21.1133511332214,-19.9557065953293,
10.3523286299233));
#16396=CARTESIAN_POINT('Ctrl Pts',(-21.3276368475072,-22.3185580498516,
8.4680174730597));
#16397=CARTESIAN_POINT('Ctrl Pts',(-21.5419225617929,-23.6298416794532,
5.74510895921686));
#16398=CARTESIAN_POINT('Ctrl Pts',(-21.7562082760786,-24.9411253090549,
3.02220044537405));
#16399=CARTESIAN_POINT('Ctrl Pts',(-21.9704939903643,-24.9411253090549,
3.46944695195361E-15));
#16400=CARTESIAN_POINT('Ctrl Pts',(-22.18477970465,-24.9411253090549,-3.02220044537404));
#16401=CARTESIAN_POINT('Ctrl Pts',(-22.3990654189357,-23.6298416794532,
-5.74510895921686));
#16402=CARTESIAN_POINT('Ctrl Pts',(-22.6133511332214,-22.3185580498516,
-8.4680174730597));
#16403=CARTESIAN_POINT('Ctrl Pts',(-22.8276368475072,-19.9557065953293,
-10.3523286299233));
#16404=CARTESIAN_POINT('Ctrl Pts',(-23.0419225617929,-17.592855140807,-12.236639786787));
#16405=CARTESIAN_POINT('Ctrl Pts',(-23.2562082760786,-14.6464275704035,
-12.9091426524948));
#16406=CARTESIAN_POINT('Ctrl Pts',(-23.4704939903643,-11.7,-13.5816455182026));
#16407=CARTESIAN_POINT('Ctrl Pts',(-23.68477970465,-8.75357242959651,-12.9091426524948));
#16408=CARTESIAN_POINT('Ctrl Pts',(-23.8990654189357,-5.80714485919301,
-12.236639786787));
#16409=CARTESIAN_POINT('Ctrl Pts',(-24.1133511332214,-3.4442934046707,-10.3523286299233));
#16410=CARTESIAN_POINT('Ctrl Pts',(-24.3276368475071,-1.08144195014838,
-8.46801747305971));
#16411=CARTESIAN_POINT('Ctrl Pts',(-24.5419225617929,0.229841679453259,
-5.74510895921687));
#16412=CARTESIAN_POINT('Ctrl Pts',(-24.7562082760786,1.54112530905491,-3.02220044537405));
#16413=CARTESIAN_POINT('Ctrl Pts',(-24.9704939903643,1.5411253090549,0.));
#16414=CARTESIAN_POINT('Ctrl Pts',(0.970493990364278,1.5411253090549,-1.38777878078145E-14));
#16415=CARTESIAN_POINT('Ctrl Pts',(0.75620827607856,1.5411253090549,3.02220044537401));
#16416=CARTESIAN_POINT('Ctrl Pts',(0.541922561792848,0.229841679453252,
5.74510895921686));
#16417=CARTESIAN_POINT('Ctrl Pts',(0.327636847507131,-1.08144195014837,
8.4680174730597));
#16418=CARTESIAN_POINT('Ctrl Pts',(0.113351133221419,-3.4442934046707,10.3523286299233));
#16419=CARTESIAN_POINT('Ctrl Pts',(-0.100934581064293,-5.80714485919301,
12.236639786787));
#16420=CARTESIAN_POINT('Ctrl Pts',(-0.315220295350009,-8.7535724295965,
12.9091426524948));
#16421=CARTESIAN_POINT('Ctrl Pts',(-0.529506009635726,-11.7,13.5816455182026));
#16422=CARTESIAN_POINT('Ctrl Pts',(-0.743791723921436,-14.6464275704035,
12.9091426524948));
#16423=CARTESIAN_POINT('Ctrl Pts',(-0.958077438207154,-17.592855140807,
12.236639786787));
#16424=CARTESIAN_POINT('Ctrl Pts',(-1.17236315249287,-19.9557065953293,
10.3523286299233));
#16425=CARTESIAN_POINT('Ctrl Pts',(-1.38664886677858,-22.3185580498516,
8.46801747305969));
#16426=CARTESIAN_POINT('Ctrl Pts',(-1.60093458106429,-23.6298416794532,
5.74510895921685));
#16427=CARTESIAN_POINT('Ctrl Pts',(-1.81522029535001,-24.9411253090549,
3.02220044537403));
#16428=CARTESIAN_POINT('Ctrl Pts',(-2.02950600963573,-24.9411253090549,
-6.93889390390723E-15));
#16429=CARTESIAN_POINT('Ctrl Pts',(-2.24379172392144,-24.9411253090549,
-3.02220044537404));
#16430=CARTESIAN_POINT('Ctrl Pts',(-2.45807743820715,-23.6298416794532,
-5.74510895921686));
#16431=CARTESIAN_POINT('Ctrl Pts',(-2.67236315249287,-22.3185580498516,
-8.4680174730597));
#16432=CARTESIAN_POINT('Ctrl Pts',(-2.88664886677858,-19.9557065953293,
-10.3523286299233));
#16433=CARTESIAN_POINT('Ctrl Pts',(-3.1009345810643,-17.592855140807,-12.236639786787));
#16434=CARTESIAN_POINT('Ctrl Pts',(-3.31522029535001,-14.6464275704035,
-12.9091426524948));
#16435=CARTESIAN_POINT('Ctrl Pts',(-3.52950600963573,-11.7,-13.5816455182026));
#16436=CARTESIAN_POINT('Ctrl Pts',(-3.74379172392144,-8.75357242959649,
-12.9091426524948));
#16437=CARTESIAN_POINT('Ctrl Pts',(-3.95807743820716,-5.80714485919301,
-12.236639786787));
#16438=CARTESIAN_POINT('Ctrl Pts',(-4.17236315249286,-3.44429340467069,
-10.3523286299233));
#16439=CARTESIAN_POINT('Ctrl Pts',(-4.38664886677858,-1.08144195014838,
-8.4680174730597));
#16440=CARTESIAN_POINT('Ctrl Pts',(-4.60093458106429,0.229841679453252,
-5.74510895921687));
#16441=CARTESIAN_POINT('Ctrl Pts',(-4.81522029535001,1.5411253090549,-3.02220044537403));
#16442=CARTESIAN_POINT('Ctrl Pts',(-5.02950600963572,1.5411253090549,0.));
#16443=CARTESIAN_POINT('Ctrl Pts',(-5.24379172392144,1.5411253090549,3.02220044537403));
#16444=CARTESIAN_POINT('Ctrl Pts',(-5.45807743820715,0.229841679453252,
5.74510895921686));
#16445=CARTESIAN_POINT('Ctrl Pts',(-5.67236315249287,-1.08144195014838,
8.4680174730597));
#16446=CARTESIAN_POINT('Ctrl Pts',(-5.88664886677858,-3.4442934046707,10.3523286299233));
#16447=CARTESIAN_POINT('Ctrl Pts',(-6.10093458106429,-5.80714485919302,
12.236639786787));
#16448=CARTESIAN_POINT('Ctrl Pts',(-6.31522029535001,-8.75357242959651,
12.9091426524948));
#16449=CARTESIAN_POINT('Ctrl Pts',(-6.52950600963572,-11.7,13.5816455182026));
#16450=CARTESIAN_POINT('Ctrl Pts',(-6.74379172392143,-14.6464275704035,
12.9091426524948));
#16451=CARTESIAN_POINT('Ctrl Pts',(-6.95807743820715,-17.592855140807,12.2366397867869));
#16452=CARTESIAN_POINT('Ctrl Pts',(-7.17236315249286,-19.9557065953293,
10.3523286299233));
#16453=CARTESIAN_POINT('Ctrl Pts',(-7.38664886677858,-22.3185580498516,
8.46801747305969));
#16454=CARTESIAN_POINT('Ctrl Pts',(-7.6009345810643,-23.6298416794532,5.74510895921687));
#16455=CARTESIAN_POINT('Ctrl Pts',(-7.81522029535001,-24.9411253090549,
3.02220044537403));
#16456=CARTESIAN_POINT('Ctrl Pts',(-8.02950600963572,-24.9411253090549,
-1.38777878078145E-14));
#16457=CARTESIAN_POINT('Ctrl Pts',(-8.24379172392144,-24.9411253090549,
-3.02220044537403));
#16458=CARTESIAN_POINT('Ctrl Pts',(-8.45807743820715,-23.6298416794532,
-5.74510895921687));
#16459=CARTESIAN_POINT('Ctrl Pts',(-8.67236315249287,-22.3185580498516,
-8.46801747305971));
#16460=CARTESIAN_POINT('Ctrl Pts',(-8.88664886677859,-19.9557065953293,
-10.3523286299233));
#16461=CARTESIAN_POINT('Ctrl Pts',(-9.10093458106429,-17.592855140807,-12.236639786787));
#16462=CARTESIAN_POINT('Ctrl Pts',(-9.31522029535001,-14.6464275704035,
-12.9091426524948));
#16463=CARTESIAN_POINT('Ctrl Pts',(-9.52950600963572,-11.7,-13.5816455182026));
#16464=CARTESIAN_POINT('Ctrl Pts',(-9.74379172392145,-8.75357242959651,
-12.9091426524948));
#16465=CARTESIAN_POINT('Ctrl Pts',(-9.95807743820715,-5.80714485919301,
-12.236639786787));
#16466=CARTESIAN_POINT('Ctrl Pts',(-10.1723631524929,-3.4442934046707,-10.3523286299233));
#16467=CARTESIAN_POINT('Ctrl Pts',(-10.3866488667786,-1.08144195014838,
-8.4680174730597));
#16468=CARTESIAN_POINT('Ctrl Pts',(-10.6009345810643,0.229841679453252,
-5.74510895921687));
#16469=CARTESIAN_POINT('Ctrl Pts',(-10.81522029535,1.5411253090549,-3.02220044537404));
#16470=CARTESIAN_POINT('Ctrl Pts',(-11.0295060096357,1.5411253090549,3.46944695195361E-15));
#16471=CARTESIAN_POINT('Ctrl Pts',(-11.2437917239214,1.5411253090549,3.02220044537404));
#16472=CARTESIAN_POINT('Ctrl Pts',(-11.4580774382071,0.229841679453252,
5.74510895921686));
#16473=CARTESIAN_POINT('Ctrl Pts',(-11.6723631524929,-1.08144195014838,
8.4680174730597));
#16474=CARTESIAN_POINT('Ctrl Pts',(-11.8866488667786,-3.4442934046707,10.3523286299233));
#16475=CARTESIAN_POINT('Ctrl Pts',(-12.1009345810643,-5.80714485919302,
12.236639786787));
#16476=CARTESIAN_POINT('Ctrl Pts',(-12.31522029535,-8.75357242959651,12.9091426524948));
#16477=CARTESIAN_POINT('Ctrl Pts',(-12.5295060096357,-11.7,13.5816455182026));
#16478=CARTESIAN_POINT('Ctrl Pts',(-12.7437917239214,-14.6464275704035,
12.9091426524948));
#16479=CARTESIAN_POINT('Ctrl Pts',(-12.9580774382071,-17.5928551408069,
12.236639786787));
#16480=CARTESIAN_POINT('Ctrl Pts',(-13.1723631524929,-19.9557065953293,
10.3523286299233));
#16481=CARTESIAN_POINT('Ctrl Pts',(-13.3866488667786,-22.3185580498516,
8.46801747305969));
#16482=CARTESIAN_POINT('Ctrl Pts',(-13.6009345810643,-23.6298416794532,
5.74510895921686));
#16483=CARTESIAN_POINT('Ctrl Pts',(-13.81522029535,-24.9411253090549,3.02220044537403));
#16484=CARTESIAN_POINT('Ctrl Pts',(-14.0295060096357,-24.9411253090549,
-6.93889390390723E-15));
#16485=CARTESIAN_POINT('Ctrl Pts',(-14.2437917239214,-24.9411253090549,
-3.02220044537403));
#16486=CARTESIAN_POINT('Ctrl Pts',(-14.4580774382072,-23.6298416794532,
-5.74510895921687));
#16487=CARTESIAN_POINT('Ctrl Pts',(-14.6723631524929,-22.3185580498516,
-8.4680174730597));
#16488=CARTESIAN_POINT('Ctrl Pts',(-14.8866488667786,-19.9557065953293,
-10.3523286299233));
#16489=CARTESIAN_POINT('Ctrl Pts',(-15.1009345810643,-17.5928551408069,
-12.236639786787));
#16490=CARTESIAN_POINT('Ctrl Pts',(-15.31522029535,-14.6464275704035,-12.9091426524948));
#16491=CARTESIAN_POINT('Ctrl Pts',(-15.5295060096357,-11.7,-13.5816455182026));
#16492=CARTESIAN_POINT('Ctrl Pts',(-15.7437917239214,-8.75357242959651,
-12.9091426524948));
#16493=CARTESIAN_POINT('Ctrl Pts',(-15.9580774382072,-5.80714485919302,
-12.236639786787));
#16494=CARTESIAN_POINT('Ctrl Pts',(-16.1723631524929,-3.4442934046707,-10.3523286299233));
#16495=CARTESIAN_POINT('Ctrl Pts',(-16.3866488667786,-1.08144195014838,
-8.4680174730597));
#16496=CARTESIAN_POINT('Ctrl Pts',(-16.6009345810643,0.229841679453259,
-5.74510895921687));
#16497=CARTESIAN_POINT('Ctrl Pts',(-16.81522029535,1.5411253090549,-3.02220044537405));
#16498=CARTESIAN_POINT('Ctrl Pts',(-17.0295060096357,1.5411253090549,0.));
#16499=CARTESIAN_POINT('Ctrl Pts',(-17.2437917239215,1.5411253090549,3.02220044537402));
#16500=CARTESIAN_POINT('Ctrl Pts',(-17.4580774382072,0.229841679453259,
5.74510895921687));
#16501=CARTESIAN_POINT('Ctrl Pts',(-17.6723631524929,-1.08144195014838,
8.4680174730597));
#16502=CARTESIAN_POINT('Ctrl Pts',(-17.8866488667786,-3.4442934046707,10.3523286299233));
#16503=CARTESIAN_POINT('Ctrl Pts',(-18.1009345810643,-5.80714485919302,
12.236639786787));
#16504=CARTESIAN_POINT('Ctrl Pts',(-18.31522029535,-8.75357242959651,12.9091426524948));
#16505=CARTESIAN_POINT('Ctrl Pts',(-18.5295060096357,-11.7,13.5816455182026));
#16506=CARTESIAN_POINT('Ctrl Pts',(-18.7437917239214,-14.6464275704035,
12.9091426524948));
#16507=CARTESIAN_POINT('Ctrl Pts',(-18.9580774382072,-17.592855140807,12.236639786787));
#16508=CARTESIAN_POINT('Ctrl Pts',(-19.1723631524929,-19.9557065953293,
10.3523286299233));
#16509=CARTESIAN_POINT('Ctrl Pts',(-19.3866488667786,-22.3185580498516,
8.46801747305969));
#16510=CARTESIAN_POINT('Ctrl Pts',(-19.6009345810643,-23.6298416794532,
5.74510895921686));
#16511=CARTESIAN_POINT('Ctrl Pts',(-19.81522029535,-24.9411253090549,3.02220044537404));
#16512=CARTESIAN_POINT('Ctrl Pts',(-20.0295060096357,-24.9411253090549,
-3.46944695195361E-15));
#16513=CARTESIAN_POINT('Ctrl Pts',(-20.2437917239214,-24.9411253090549,
-3.02220044537404));
#16514=CARTESIAN_POINT('Ctrl Pts',(-20.4580774382072,-23.6298416794532,
-5.74510895921686));
#16515=CARTESIAN_POINT('Ctrl Pts',(-20.6723631524929,-22.3185580498516,
-8.4680174730597));
#16516=CARTESIAN_POINT('Ctrl Pts',(-20.8866488667786,-19.9557065953293,
-10.3523286299233));
#16517=CARTESIAN_POINT('Ctrl Pts',(-21.1009345810643,-17.5928551408069,
-12.236639786787));
#16518=CARTESIAN_POINT('Ctrl Pts',(-21.31522029535,-14.6464275704035,-12.9091426524948));
#16519=CARTESIAN_POINT('Ctrl Pts',(-21.5295060096357,-11.7,-13.5816455182026));
#16520=CARTESIAN_POINT('Ctrl Pts',(-21.7437917239214,-8.7535724295965,-12.9091426524948));
#16521=CARTESIAN_POINT('Ctrl Pts',(-21.9580774382072,-5.80714485919302,
-12.236639786787));
#16522=CARTESIAN_POINT('Ctrl Pts',(-22.1723631524929,-3.4442934046707,-10.3523286299234));
#16523=CARTESIAN_POINT('Ctrl Pts',(-22.3866488667786,-1.08144195014838,
-8.4680174730597));
#16524=CARTESIAN_POINT('Ctrl Pts',(-22.6009345810643,0.229841679453252,
-5.74510895921687));
#16525=CARTESIAN_POINT('Ctrl Pts',(-22.81522029535,1.5411253090549,-3.02220044537406));
#16526=CARTESIAN_POINT('Ctrl Pts',(-23.0295060096357,1.5411253090549,0.));
#16527=CARTESIAN_POINT('Ctrl Pts',(0.654743522119005,2.81197461594778,-1.40439689870177E-14));
#16528=CARTESIAN_POINT('Ctrl Pts',(0.440457807833292,2.81197461594777,3.31226350660556));
#16529=CARTESIAN_POINT('Ctrl Pts',(0.226172093547578,1.37483734075912,6.29650980834649));
#16530=CARTESIAN_POINT('Ctrl Pts',(0.0118863792618643,-0.0622999344295592,
9.28075611008742));
#16531=CARTESIAN_POINT('Ctrl Pts',(-0.20239933502385,-2.65193182212373,
11.3459186275248));
#16532=CARTESIAN_POINT('Ctrl Pts',(-0.416685049309565,-5.24156370981795,
13.4110811449623));
#16533=CARTESIAN_POINT('Ctrl Pts',(-0.630970763595279,-8.47078185490895,
14.1481291139616));
#16534=CARTESIAN_POINT('Ctrl Pts',(-0.84525647788099,-11.7,14.8851770829608));
#16535=CARTESIAN_POINT('Ctrl Pts',(-1.05954219216671,-14.929218145091,14.1481291139616));
#16536=CARTESIAN_POINT('Ctrl Pts',(-1.27382790645242,-18.158436290182,13.4110811449623));
#16537=CARTESIAN_POINT('Ctrl Pts',(-1.48811362073814,-20.7480681778762,
11.3459186275248));
#16538=CARTESIAN_POINT('Ctrl Pts',(-1.70239933502385,-23.3377000655704,
9.2807561100874));
#16539=CARTESIAN_POINT('Ctrl Pts',(-1.91668504930957,-24.7748373407591,
6.29650980834649));
#16540=CARTESIAN_POINT('Ctrl Pts',(-2.13097076359528,-26.2119746159477,
3.31226350660556));
#16541=CARTESIAN_POINT('Ctrl Pts',(-2.345256477881,-26.2119746159478,-1.75549612337721E-14));
#16542=CARTESIAN_POINT('Ctrl Pts',(-2.55954219216671,-26.2119746159478,
-3.31226350660559));
#16543=CARTESIAN_POINT('Ctrl Pts',(-2.77382790645242,-24.7748373407591,
-6.29650980834651));
#16544=CARTESIAN_POINT('Ctrl Pts',(-2.98811362073814,-23.3377000655704,
-9.28075611008743));
#16545=CARTESIAN_POINT('Ctrl Pts',(-3.20239933502385,-20.7480681778762,
-11.3459186275249));
#16546=CARTESIAN_POINT('Ctrl Pts',(-3.41668504930957,-18.158436290182,-13.4110811449623));
#16547=CARTESIAN_POINT('Ctrl Pts',(-3.63097076359528,-14.929218145091,-14.1481291139616));
#16548=CARTESIAN_POINT('Ctrl Pts',(-3.845256477881,-11.7,-14.8851770829609));
#16549=CARTESIAN_POINT('Ctrl Pts',(-4.05954219216671,-8.47078185490897,
-14.1481291139616));
#16550=CARTESIAN_POINT('Ctrl Pts',(-4.27382790645242,-5.24156370981795,
-13.4110811449623));
#16551=CARTESIAN_POINT('Ctrl Pts',(-4.48811362073814,-2.65193182212374,
-11.3459186275249));
#16552=CARTESIAN_POINT('Ctrl Pts',(-4.70239933502385,-0.0622999344295592,
-9.28075611008746));
#16553=CARTESIAN_POINT('Ctrl Pts',(-4.91668504930956,1.37483734075911,-6.29650980834651));
#16554=CARTESIAN_POINT('Ctrl Pts',(-5.13097076359528,2.81197461594777,-3.31226350660559));
#16555=CARTESIAN_POINT('Ctrl Pts',(-5.34525647788099,2.81197461594778,-7.02198449350884E-15));
#16556=CARTESIAN_POINT('Ctrl Pts',(-5.55954219216671,2.81197461594777,3.31226350660558));
#16557=CARTESIAN_POINT('Ctrl Pts',(-5.77382790645242,1.37483734075912,6.29650980834649));
#16558=CARTESIAN_POINT('Ctrl Pts',(-5.98811362073814,-0.0622999344295592,
9.28075611008741));
#16559=CARTESIAN_POINT('Ctrl Pts',(-6.20239933502385,-2.65193182212374,
11.3459186275248));
#16560=CARTESIAN_POINT('Ctrl Pts',(-6.41668504930957,-5.24156370981794,
13.4110811449623));
#16561=CARTESIAN_POINT('Ctrl Pts',(-6.63097076359528,-8.47078185490896,
14.1481291139616));
#16562=CARTESIAN_POINT('Ctrl Pts',(-6.84525647788099,-11.7,14.8851770829608));
#16563=CARTESIAN_POINT('Ctrl Pts',(-7.05954219216671,-14.929218145091,14.1481291139616));
#16564=CARTESIAN_POINT('Ctrl Pts',(-7.27382790645243,-18.158436290182,13.4110811449623));
#16565=CARTESIAN_POINT('Ctrl Pts',(-7.48811362073814,-20.7480681778762,
11.3459186275248));
#16566=CARTESIAN_POINT('Ctrl Pts',(-7.70239933502385,-23.3377000655704,
9.28075611008742));
#16567=CARTESIAN_POINT('Ctrl Pts',(-7.91668504930957,-24.7748373407591,
6.2965098083465));
#16568=CARTESIAN_POINT('Ctrl Pts',(-8.13097076359528,-26.2119746159478,
3.31226350660557));
#16569=CARTESIAN_POINT('Ctrl Pts',(-8.345256477881,-26.2119746159478,-1.75549612337721E-14));
#16570=CARTESIAN_POINT('Ctrl Pts',(-8.55954219216671,-26.2119746159478,
-3.3122635066056));
#16571=CARTESIAN_POINT('Ctrl Pts',(-8.77382790645243,-24.7748373407591,
-6.29650980834652));
#16572=CARTESIAN_POINT('Ctrl Pts',(-8.98811362073814,-23.3377000655704,
-9.28075611008744));
#16573=CARTESIAN_POINT('Ctrl Pts',(-9.20239933502386,-20.7480681778762,
-11.3459186275249));
#16574=CARTESIAN_POINT('Ctrl Pts',(-9.41668504930956,-18.158436290182,-13.4110811449623));
#16575=CARTESIAN_POINT('Ctrl Pts',(-9.63097076359528,-14.929218145091,-14.1481291139616));
#16576=CARTESIAN_POINT('Ctrl Pts',(-9.84525647788099,-11.7,-14.8851770829609));
#16577=CARTESIAN_POINT('Ctrl Pts',(-10.0595421921667,-8.47078185490896,
-14.1481291139616));
#16578=CARTESIAN_POINT('Ctrl Pts',(-10.2738279064524,-5.24156370981796,
-13.4110811449623));
#16579=CARTESIAN_POINT('Ctrl Pts',(-10.4881136207381,-2.65193182212374,
-11.3459186275249));
#16580=CARTESIAN_POINT('Ctrl Pts',(-10.7023993350239,-0.0622999344295592,
-9.28075611008745));
#16581=CARTESIAN_POINT('Ctrl Pts',(-10.9166850493096,1.37483734075912,-6.29650980834652));
#16582=CARTESIAN_POINT('Ctrl Pts',(-11.1309707635953,2.81197461594777,-3.31226350660559));
#16583=CARTESIAN_POINT('Ctrl Pts',(-11.345256477881,2.81197461594778,-2.10659534805265E-14));
#16584=CARTESIAN_POINT('Ctrl Pts',(-11.5595421921667,2.81197461594777,3.31226350660557));
#16585=CARTESIAN_POINT('Ctrl Pts',(-11.7738279064524,1.37483734075912,6.2965098083465));
#16586=CARTESIAN_POINT('Ctrl Pts',(-11.9881136207381,-0.0622999344295592,
9.2807561100874));
#16587=CARTESIAN_POINT('Ctrl Pts',(-12.2023993350239,-2.65193182212374,
11.3459186275248));
#16588=CARTESIAN_POINT('Ctrl Pts',(-12.4166850493096,-5.24156370981794,
13.4110811449623));
#16589=CARTESIAN_POINT('Ctrl Pts',(-12.6309707635953,-8.47078185490896,
14.1481291139616));
#16590=CARTESIAN_POINT('Ctrl Pts',(-12.845256477881,-11.7,14.8851770829609));
#16591=CARTESIAN_POINT('Ctrl Pts',(-13.0595421921667,-14.929218145091,14.1481291139616));
#16592=CARTESIAN_POINT('Ctrl Pts',(-13.2738279064524,-18.158436290182,13.4110811449623));
#16593=CARTESIAN_POINT('Ctrl Pts',(-13.4881136207381,-20.7480681778762,
11.3459186275248));
#16594=CARTESIAN_POINT('Ctrl Pts',(-13.7023993350239,-23.3377000655704,
9.28075611008741));
#16595=CARTESIAN_POINT('Ctrl Pts',(-13.9166850493096,-24.7748373407591,
6.2965098083465));
#16596=CARTESIAN_POINT('Ctrl Pts',(-14.1309707635953,-26.2119746159478,
3.31226350660557));
#16597=CARTESIAN_POINT('Ctrl Pts',(-14.345256477881,-26.2119746159478,-7.02198449350884E-15));
#16598=CARTESIAN_POINT('Ctrl Pts',(-14.5595421921667,-26.2119746159478,
-3.31226350660558));
#16599=CARTESIAN_POINT('Ctrl Pts',(-14.7738279064524,-24.7748373407591,
-6.29650980834651));
#16600=CARTESIAN_POINT('Ctrl Pts',(-14.9881136207381,-23.3377000655704,
-9.28075611008744));
#16601=CARTESIAN_POINT('Ctrl Pts',(-15.2023993350239,-20.7480681778762,
-11.3459186275248));
#16602=CARTESIAN_POINT('Ctrl Pts',(-15.4166850493096,-18.158436290182,-13.4110811449623));
#16603=CARTESIAN_POINT('Ctrl Pts',(-15.6309707635953,-14.929218145091,-14.1481291139616));
#16604=CARTESIAN_POINT('Ctrl Pts',(-15.845256477881,-11.7,-14.8851770829609));
#16605=CARTESIAN_POINT('Ctrl Pts',(-16.0595421921667,-8.47078185490896,
-14.1481291139616));
#16606=CARTESIAN_POINT('Ctrl Pts',(-16.2738279064524,-5.24156370981796,
-13.4110811449623));
#16607=CARTESIAN_POINT('Ctrl Pts',(-16.4881136207381,-2.65193182212374,
-11.3459186275249));
#16608=CARTESIAN_POINT('Ctrl Pts',(-16.7023993350239,-0.0622999344295592,
-9.28075611008745));
#16609=CARTESIAN_POINT('Ctrl Pts',(-16.9166850493096,1.37483734075912,-6.29650980834652));
#16610=CARTESIAN_POINT('Ctrl Pts',(-17.1309707635953,2.81197461594777,-3.3122635066056));
#16611=CARTESIAN_POINT('Ctrl Pts',(-17.345256477881,2.81197461594778,-1.75549612337721E-14));
#16612=CARTESIAN_POINT('Ctrl Pts',(-17.5595421921667,2.81197461594777,3.31226350660556));
#16613=CARTESIAN_POINT('Ctrl Pts',(-17.7738279064524,1.37483734075912,6.29650980834649));
#16614=CARTESIAN_POINT('Ctrl Pts',(-17.9881136207381,-0.0622999344295592,
9.28075611008742));
#16615=CARTESIAN_POINT('Ctrl Pts',(-18.2023993350239,-2.65193182212374,
11.3459186275248));
#16616=CARTESIAN_POINT('Ctrl Pts',(-18.4166850493096,-5.24156370981795,
13.4110811449623));
#16617=CARTESIAN_POINT('Ctrl Pts',(-18.6309707635953,-8.47078185490896,
14.1481291139616));
#16618=CARTESIAN_POINT('Ctrl Pts',(-18.845256477881,-11.7,14.8851770829608));
#16619=CARTESIAN_POINT('Ctrl Pts',(-19.0595421921667,-14.929218145091,14.1481291139616));
#16620=CARTESIAN_POINT('Ctrl Pts',(-19.2738279064524,-18.158436290182,13.4110811449623));
#16621=CARTESIAN_POINT('Ctrl Pts',(-19.4881136207381,-20.7480681778762,
11.3459186275248));
#16622=CARTESIAN_POINT('Ctrl Pts',(-19.7023993350239,-23.3377000655704,
9.28075611008741));
#16623=CARTESIAN_POINT('Ctrl Pts',(-19.9166850493096,-24.7748373407591,
6.29650980834649));
#16624=CARTESIAN_POINT('Ctrl Pts',(-20.1309707635953,-26.2119746159478,
3.31226350660556));
#16625=CARTESIAN_POINT('Ctrl Pts',(-20.345256477881,-26.2119746159478,-1.75549612337721E-14));
#16626=CARTESIAN_POINT('Ctrl Pts',(-20.5595421921667,-26.2119746159478,
-3.31226350660559));
#16627=CARTESIAN_POINT('Ctrl Pts',(-20.7738279064524,-24.7748373407591,
-6.29650980834651));
#16628=CARTESIAN_POINT('Ctrl Pts',(-20.9881136207381,-23.3377000655704,
-9.28075611008743));
#16629=CARTESIAN_POINT('Ctrl Pts',(-21.2023993350239,-20.7480681778762,
-11.3459186275249));
#16630=CARTESIAN_POINT('Ctrl Pts',(-21.4166850493096,-18.158436290182,-13.4110811449623));
#16631=CARTESIAN_POINT('Ctrl Pts',(-21.6309707635953,-14.929218145091,-14.1481291139616));
#16632=CARTESIAN_POINT('Ctrl Pts',(-21.845256477881,-11.7,-14.8851770829609));
#16633=CARTESIAN_POINT('Ctrl Pts',(-22.0595421921667,-8.47078185490896,
-14.1481291139616));
#16634=CARTESIAN_POINT('Ctrl Pts',(-22.2738279064524,-5.24156370981795,
-13.4110811449623));
#16635=CARTESIAN_POINT('Ctrl Pts',(-22.4881136207381,-2.65193182212374,
-11.3459186275249));
#16636=CARTESIAN_POINT('Ctrl Pts',(-22.7023993350238,-0.0622999344295592,
-9.28075611008743));
#16637=CARTESIAN_POINT('Ctrl Pts',(-22.9166850493096,1.37483734075912,-6.29650980834652));
#16638=CARTESIAN_POINT('Ctrl Pts',(-23.1309707635953,2.81197461594777,-3.31226350660561));
#16639=CARTESIAN_POINT('Ctrl Pts',(-23.345256477881,2.81197461594778,-1.40439689870177E-14));
#16640=CARTESIAN_POINT('Ctrl Pts',(-0.65474352211901,2.81197461594778,-2.10659534805265E-14));
#16641=CARTESIAN_POINT('Ctrl Pts',(-0.869029236404722,2.81197461594777,
3.31226350660557));
#16642=CARTESIAN_POINT('Ctrl Pts',(-1.08331495069044,1.37483734075912,6.2965098083465));
#16643=CARTESIAN_POINT('Ctrl Pts',(-1.29760066497615,-0.0622999344295592,
9.28075611008742));
#16644=CARTESIAN_POINT('Ctrl Pts',(-1.51188637926187,-2.65193182212374,
11.3459186275248));
#16645=CARTESIAN_POINT('Ctrl Pts',(-1.72617209354758,-5.24156370981795,
13.4110811449623));
#16646=CARTESIAN_POINT('Ctrl Pts',(-1.94045780783329,-8.47078185490896,
14.1481291139616));
#16647=CARTESIAN_POINT('Ctrl Pts',(-2.15474352211901,-11.7,14.8851770829608));
#16648=CARTESIAN_POINT('Ctrl Pts',(-2.36902923640472,-14.929218145091,14.1481291139616));
#16649=CARTESIAN_POINT('Ctrl Pts',(-2.58331495069044,-18.158436290182,13.4110811449623));
#16650=CARTESIAN_POINT('Ctrl Pts',(-2.79760066497615,-20.7480681778762,
11.3459186275249));
#16651=CARTESIAN_POINT('Ctrl Pts',(-3.01188637926187,-23.3377000655704,
9.28075611008742));
#16652=CARTESIAN_POINT('Ctrl Pts',(-3.22617209354758,-24.7748373407591,
6.2965098083465));
#16653=CARTESIAN_POINT('Ctrl Pts',(-3.4404578078333,-26.2119746159477,3.31226350660556));
#16654=CARTESIAN_POINT('Ctrl Pts',(-3.65474352211901,-26.2119746159478,
-1.75549612337721E-14));
#16655=CARTESIAN_POINT('Ctrl Pts',(-3.86902923640472,-26.2119746159477,
-3.3122635066056));
#16656=CARTESIAN_POINT('Ctrl Pts',(-4.08331495069044,-24.7748373407591,
-6.29650980834652));
#16657=CARTESIAN_POINT('Ctrl Pts',(-4.29760066497615,-23.3377000655704,
-9.28075611008743));
#16658=CARTESIAN_POINT('Ctrl Pts',(-4.51188637926187,-20.7480681778762,
-11.3459186275249));
#16659=CARTESIAN_POINT('Ctrl Pts',(-4.72617209354758,-18.158436290182,-13.4110811449623));
#16660=CARTESIAN_POINT('Ctrl Pts',(-4.94045780783329,-14.929218145091,-14.1481291139616));
#16661=CARTESIAN_POINT('Ctrl Pts',(-5.15474352211901,-11.7,-14.8851770829609));
#16662=CARTESIAN_POINT('Ctrl Pts',(-5.36902923640472,-8.47078185490896,
-14.1481291139616));
#16663=CARTESIAN_POINT('Ctrl Pts',(-5.58331495069044,-5.24156370981795,
-13.4110811449623));
#16664=CARTESIAN_POINT('Ctrl Pts',(-5.79760066497615,-2.65193182212374,
-11.3459186275249));
#16665=CARTESIAN_POINT('Ctrl Pts',(-6.01188637926186,-0.0622999344295592,
-9.28075611008746));
#16666=CARTESIAN_POINT('Ctrl Pts',(-6.22617209354758,1.37483734075912,-6.29650980834653));
#16667=CARTESIAN_POINT('Ctrl Pts',(-6.44045780783329,2.81197461594777,-3.3122635066056));
#16668=CARTESIAN_POINT('Ctrl Pts',(-6.65474352211901,2.81197461594778,-1.40439689870177E-14));
#16669=CARTESIAN_POINT('Ctrl Pts',(-6.86902923640472,2.81197461594777,3.31226350660556));
#16670=CARTESIAN_POINT('Ctrl Pts',(-7.08331495069044,1.37483734075912,6.29650980834649));
#16671=CARTESIAN_POINT('Ctrl Pts',(-7.29760066497615,-0.0622999344295592,
9.28075611008741));
#16672=CARTESIAN_POINT('Ctrl Pts',(-7.51188637926187,-2.65193182212374,
11.3459186275248));
#16673=CARTESIAN_POINT('Ctrl Pts',(-7.72617209354758,-5.24156370981794,
13.4110811449623));
#16674=CARTESIAN_POINT('Ctrl Pts',(-7.9404578078333,-8.47078185490896,14.1481291139616));
#16675=CARTESIAN_POINT('Ctrl Pts',(-8.15474352211901,-11.7,14.8851770829609));
#16676=CARTESIAN_POINT('Ctrl Pts',(-8.36902923640472,-14.929218145091,14.1481291139616));
#16677=CARTESIAN_POINT('Ctrl Pts',(-8.58331495069044,-18.158436290182,13.4110811449623));
#16678=CARTESIAN_POINT('Ctrl Pts',(-8.79760066497615,-20.7480681778762,
11.3459186275248));
#16679=CARTESIAN_POINT('Ctrl Pts',(-9.01188637926186,-23.3377000655704,
9.28075611008741));
#16680=CARTESIAN_POINT('Ctrl Pts',(-9.22617209354758,-24.7748373407591,
6.2965098083465));
#16681=CARTESIAN_POINT('Ctrl Pts',(-9.44045780783329,-26.2119746159478,
3.31226350660557));
#16682=CARTESIAN_POINT('Ctrl Pts',(-9.65474352211901,-26.2119746159478,
-1.05329767402633E-14));
#16683=CARTESIAN_POINT('Ctrl Pts',(-9.86902923640472,-26.2119746159478,
-3.31226350660559));
#16684=CARTESIAN_POINT('Ctrl Pts',(-10.0833149506904,-24.7748373407591,
-6.29650980834652));
#16685=CARTESIAN_POINT('Ctrl Pts',(-10.2976006649762,-23.3377000655704,
-9.28075611008745));
#16686=CARTESIAN_POINT('Ctrl Pts',(-10.5118863792619,-20.7480681778762,
-11.3459186275249));
#16687=CARTESIAN_POINT('Ctrl Pts',(-10.7261720935476,-18.158436290182,-13.4110811449623));
#16688=CARTESIAN_POINT('Ctrl Pts',(-10.9404578078333,-14.929218145091,-14.1481291139616));
#16689=CARTESIAN_POINT('Ctrl Pts',(-11.154743522119,-11.7,-14.8851770829609));
#16690=CARTESIAN_POINT('Ctrl Pts',(-11.3690292364047,-8.47078185490896,
-14.1481291139616));
#16691=CARTESIAN_POINT('Ctrl Pts',(-11.5833149506904,-5.24156370981795,
-13.4110811449623));
#16692=CARTESIAN_POINT('Ctrl Pts',(-11.7976006649762,-2.65193182212373,
-11.3459186275249));
#16693=CARTESIAN_POINT('Ctrl Pts',(-12.0118863792619,-0.0622999344295592,
-9.28075611008745));
#16694=CARTESIAN_POINT('Ctrl Pts',(-12.2261720935476,1.37483734075911,-6.29650980834651));
#16695=CARTESIAN_POINT('Ctrl Pts',(-12.4404578078333,2.81197461594777,-3.3122635066056));
#16696=CARTESIAN_POINT('Ctrl Pts',(-12.654743522119,2.81197461594778,-2.10659534805265E-14));
#16697=CARTESIAN_POINT('Ctrl Pts',(-12.8690292364047,2.81197461594777,3.31226350660555));
#16698=CARTESIAN_POINT('Ctrl Pts',(-13.0833149506904,1.37483734075912,6.2965098083465));
#16699=CARTESIAN_POINT('Ctrl Pts',(-13.2976006649762,-0.0622999344295736,
9.28075611008741));
#16700=CARTESIAN_POINT('Ctrl Pts',(-13.5118863792619,-2.65193182212374,
11.3459186275248));
#16701=CARTESIAN_POINT('Ctrl Pts',(-13.7261720935476,-5.24156370981795,
13.4110811449623));
#16702=CARTESIAN_POINT('Ctrl Pts',(-13.9404578078333,-8.47078185490895,
14.1481291139616));
#16703=CARTESIAN_POINT('Ctrl Pts',(-14.154743522119,-11.7,14.8851770829609));
#16704=CARTESIAN_POINT('Ctrl Pts',(-14.3690292364047,-14.929218145091,14.1481291139616));
#16705=CARTESIAN_POINT('Ctrl Pts',(-14.5833149506904,-18.158436290182,13.4110811449623));
#16706=CARTESIAN_POINT('Ctrl Pts',(-14.7976006649762,-20.7480681778762,
11.3459186275248));
#16707=CARTESIAN_POINT('Ctrl Pts',(-15.0118863792619,-23.3377000655704,
9.28075611008742));
#16708=CARTESIAN_POINT('Ctrl Pts',(-15.2261720935476,-24.7748373407591,
6.29650980834649));
#16709=CARTESIAN_POINT('Ctrl Pts',(-15.4404578078333,-26.2119746159478,
3.31226350660556));
#16710=CARTESIAN_POINT('Ctrl Pts',(-15.654743522119,-26.2119746159477,-7.02198449350884E-15));
#16711=CARTESIAN_POINT('Ctrl Pts',(-15.8690292364047,-26.2119746159478,
-3.31226350660559));
#16712=CARTESIAN_POINT('Ctrl Pts',(-16.0833149506904,-24.7748373407591,
-6.2965098083465));
#16713=CARTESIAN_POINT('Ctrl Pts',(-16.2976006649761,-23.3377000655704,
-9.28075611008744));
#16714=CARTESIAN_POINT('Ctrl Pts',(-16.5118863792619,-20.7480681778762,
-11.3459186275249));
#16715=CARTESIAN_POINT('Ctrl Pts',(-16.7261720935476,-18.158436290182,-13.4110811449623));
#16716=CARTESIAN_POINT('Ctrl Pts',(-16.9404578078333,-14.929218145091,-14.1481291139616));
#16717=CARTESIAN_POINT('Ctrl Pts',(-17.154743522119,-11.7,-14.8851770829609));
#16718=CARTESIAN_POINT('Ctrl Pts',(-17.3690292364047,-8.47078185490896,
-14.1481291139616));
#16719=CARTESIAN_POINT('Ctrl Pts',(-17.5833149506904,-5.24156370981795,
-13.4110811449623));
#16720=CARTESIAN_POINT('Ctrl Pts',(-17.7976006649762,-2.65193182212373,
-11.3459186275249));
#16721=CARTESIAN_POINT('Ctrl Pts',(-18.0118863792619,-0.0622999344295592,
-9.28075611008744));
#16722=CARTESIAN_POINT('Ctrl Pts',(-18.2261720935476,1.37483734075912,-6.29650980834652));
#16723=CARTESIAN_POINT('Ctrl Pts',(-18.4404578078333,2.81197461594777,-3.31226350660559));
#16724=CARTESIAN_POINT('Ctrl Pts',(-18.654743522119,2.81197461594776,-1.05329767402633E-14));
#16725=CARTESIAN_POINT('Ctrl Pts',(-18.8690292364047,2.81197461594777,3.31226350660557));
#16726=CARTESIAN_POINT('Ctrl Pts',(-19.0833149506904,1.37483734075912,6.29650980834649));
#16727=CARTESIAN_POINT('Ctrl Pts',(-19.2976006649762,-0.0622999344295592,
9.28075611008741));
#16728=CARTESIAN_POINT('Ctrl Pts',(-19.5118863792619,-2.65193182212374,
11.3459186275248));
#16729=CARTESIAN_POINT('Ctrl Pts',(-19.7261720935476,-5.24156370981794,
13.4110811449623));
#16730=CARTESIAN_POINT('Ctrl Pts',(-19.9404578078333,-8.47078185490896,
14.1481291139616));
#16731=CARTESIAN_POINT('Ctrl Pts',(-20.154743522119,-11.7,14.8851770829608));
#16732=CARTESIAN_POINT('Ctrl Pts',(-20.3690292364048,-14.929218145091,14.1481291139616));
#16733=CARTESIAN_POINT('Ctrl Pts',(-20.5833149506904,-18.158436290182,13.4110811449623));
#16734=CARTESIAN_POINT('Ctrl Pts',(-20.7976006649762,-20.7480681778762,
11.3459186275248));
#16735=CARTESIAN_POINT('Ctrl Pts',(-21.0118863792619,-23.3377000655704,
9.28075611008741));
#16736=CARTESIAN_POINT('Ctrl Pts',(-21.2261720935476,-24.7748373407591,
6.2965098083465));
#16737=CARTESIAN_POINT('Ctrl Pts',(-21.4404578078333,-26.2119746159477,
3.31226350660557));
#16738=CARTESIAN_POINT('Ctrl Pts',(-21.654743522119,-26.2119746159478,-1.75549612337721E-14));
#16739=CARTESIAN_POINT('Ctrl Pts',(-21.8690292364047,-26.2119746159478,
-3.31226350660559));
#16740=CARTESIAN_POINT('Ctrl Pts',(-22.0833149506904,-24.7748373407591,
-6.29650980834651));
#16741=CARTESIAN_POINT('Ctrl Pts',(-22.2976006649762,-23.3377000655704,
-9.28075611008745));
#16742=CARTESIAN_POINT('Ctrl Pts',(-22.5118863792619,-20.7480681778762,
-11.3459186275249));
#16743=CARTESIAN_POINT('Ctrl Pts',(-22.7261720935476,-18.158436290182,-13.4110811449623));
#16744=CARTESIAN_POINT('Ctrl Pts',(-22.9404578078333,-14.929218145091,-14.1481291139616));
#16745=CARTESIAN_POINT('Ctrl Pts',(-23.154743522119,-11.7,-14.8851770829609));
#16746=CARTESIAN_POINT('Ctrl Pts',(-23.3690292364047,-8.47078185490896,
-14.1481291139616));
#16747=CARTESIAN_POINT('Ctrl Pts',(-23.5833149506904,-5.24156370981795,
-13.4110811449623));
#16748=CARTESIAN_POINT('Ctrl Pts',(-23.7976006649762,-2.65193182212375,
-11.3459186275249));
#16749=CARTESIAN_POINT('Ctrl Pts',(-24.0118863792619,-0.0622999344295592,
-9.28075611008744));
#16750=CARTESIAN_POINT('Ctrl Pts',(-24.2261720935476,1.37483734075912,-6.29650980834651));
#16751=CARTESIAN_POINT('Ctrl Pts',(-24.4404578078333,2.81197461594777,-3.3122635066056));
#16752=CARTESIAN_POINT('Ctrl Pts',(-24.654743522119,2.81197461594778,-1.40439689870177E-14));
#16753=CARTESIAN_POINT('Ctrl Pts',(-0.97049399036428,1.5411253090549,-6.93889390390723E-15));
#16754=CARTESIAN_POINT('Ctrl Pts',(-1.18477970465,1.5411253090549,3.02220044537404));
#16755=CARTESIAN_POINT('Ctrl Pts',(-1.39906541893571,0.229841679453259,
5.74510895921686));
#16756=CARTESIAN_POINT('Ctrl Pts',(-1.61335113322143,-1.08144195014837,
8.46801747305969));
#16757=CARTESIAN_POINT('Ctrl Pts',(-1.82763684750714,-3.4442934046707,10.3523286299233));
#16758=CARTESIAN_POINT('Ctrl Pts',(-2.04192256179286,-5.80714485919302,
12.236639786787));
#16759=CARTESIAN_POINT('Ctrl Pts',(-2.25620827607857,-8.75357242959651,
12.9091426524948));
#16760=CARTESIAN_POINT('Ctrl Pts',(-2.47049399036428,-11.7,13.5816455182026));
#16761=CARTESIAN_POINT('Ctrl Pts',(-2.68477970464999,-14.6464275704035,
12.9091426524948));
#16762=CARTESIAN_POINT('Ctrl Pts',(-2.89906541893571,-17.592855140807,12.236639786787));
#16763=CARTESIAN_POINT('Ctrl Pts',(-3.11335113322142,-19.9557065953293,
10.3523286299233));
#16764=CARTESIAN_POINT('Ctrl Pts',(-3.32763684750714,-22.3185580498516,
8.46801747305969));
#16765=CARTESIAN_POINT('Ctrl Pts',(-3.54192256179285,-23.6298416794532,
5.74510895921685));
#16766=CARTESIAN_POINT('Ctrl Pts',(-3.75620827607857,-24.9411253090549,
3.02220044537403));
#16767=CARTESIAN_POINT('Ctrl Pts',(-3.97049399036428,-24.9411253090549,
-6.93889390390723E-15));
#16768=CARTESIAN_POINT('Ctrl Pts',(-4.18477970464999,-24.9411253090549,
-3.02220044537404));
#16769=CARTESIAN_POINT('Ctrl Pts',(-4.39906541893571,-23.6298416794532,
-5.74510895921685));
#16770=CARTESIAN_POINT('Ctrl Pts',(-4.61335113322142,-22.3185580498516,
-8.46801747305969));
#16771=CARTESIAN_POINT('Ctrl Pts',(-4.82763684750714,-19.9557065953293,
-10.3523286299233));
#16772=CARTESIAN_POINT('Ctrl Pts',(-5.04192256179286,-17.592855140807,-12.236639786787));
#16773=CARTESIAN_POINT('Ctrl Pts',(-5.25620827607857,-14.6464275704035,
-12.9091426524948));
#16774=CARTESIAN_POINT('Ctrl Pts',(-5.47049399036429,-11.7,-13.5816455182026));
#16775=CARTESIAN_POINT('Ctrl Pts',(-5.68477970464999,-8.75357242959651,
-12.9091426524948));
#16776=CARTESIAN_POINT('Ctrl Pts',(-5.89906541893571,-5.80714485919302,
-12.236639786787));
#16777=CARTESIAN_POINT('Ctrl Pts',(-6.11335113322142,-3.4442934046707,-10.3523286299233));
#16778=CARTESIAN_POINT('Ctrl Pts',(-6.32763684750714,-1.08144195014838,
-8.46801747305971));
#16779=CARTESIAN_POINT('Ctrl Pts',(-6.54192256179285,0.229841679453252,
-5.74510895921688));
#16780=CARTESIAN_POINT('Ctrl Pts',(-6.75620827607857,1.5411253090549,-3.02220044537405));
#16781=CARTESIAN_POINT('Ctrl Pts',(-6.97049399036428,1.54112530905488,-6.93889390390723E-15));
#16782=CARTESIAN_POINT('Ctrl Pts',(-7.18477970465,1.5411253090549,3.02220044537401));
#16783=CARTESIAN_POINT('Ctrl Pts',(-7.39906541893571,0.229841679453252,
5.74510895921687));
#16784=CARTESIAN_POINT('Ctrl Pts',(-7.61335113322142,-1.08144195014837,
8.4680174730597));
#16785=CARTESIAN_POINT('Ctrl Pts',(-7.82763684750714,-3.4442934046707,10.3523286299233));
#16786=CARTESIAN_POINT('Ctrl Pts',(-8.04192256179286,-5.80714485919302,
12.236639786787));
#16787=CARTESIAN_POINT('Ctrl Pts',(-8.25620827607856,-8.75357242959651,
12.9091426524948));
#16788=CARTESIAN_POINT('Ctrl Pts',(-8.47049399036428,-11.7,13.5816455182026));
#16789=CARTESIAN_POINT('Ctrl Pts',(-8.68477970464999,-14.6464275704035,
12.9091426524948));
#16790=CARTESIAN_POINT('Ctrl Pts',(-8.89906541893571,-17.592855140807,12.236639786787));
#16791=CARTESIAN_POINT('Ctrl Pts',(-9.11335113322142,-19.9557065953293,
10.3523286299233));
#16792=CARTESIAN_POINT('Ctrl Pts',(-9.32763684750714,-22.3185580498516,
8.4680174730597));
#16793=CARTESIAN_POINT('Ctrl Pts',(-9.54192256179285,-23.6298416794532,
5.74510895921686));
#16794=CARTESIAN_POINT('Ctrl Pts',(-9.75620827607857,-24.9411253090549,
3.02220044537403));
#16795=CARTESIAN_POINT('Ctrl Pts',(-9.97049399036428,-24.9411253090549,
-6.93889390390723E-15));
#16796=CARTESIAN_POINT('Ctrl Pts',(-10.18477970465,-24.9411253090549,-3.02220044537404));
#16797=CARTESIAN_POINT('Ctrl Pts',(-10.3990654189357,-23.6298416794532,
-5.74510895921686));
#16798=CARTESIAN_POINT('Ctrl Pts',(-10.6133511332214,-22.3185580498516,
-8.46801747305971));
#16799=CARTESIAN_POINT('Ctrl Pts',(-10.8276368475071,-19.9557065953293,
-10.3523286299233));
#16800=CARTESIAN_POINT('Ctrl Pts',(-11.0419225617928,-17.5928551408069,
-12.236639786787));
#16801=CARTESIAN_POINT('Ctrl Pts',(-11.2562082760786,-14.6464275704035,
-12.9091426524948));
#16802=CARTESIAN_POINT('Ctrl Pts',(-11.4704939903643,-11.7,-13.5816455182026));
#16803=CARTESIAN_POINT('Ctrl Pts',(-11.68477970465,-8.75357242959649,-12.9091426524948));
#16804=CARTESIAN_POINT('Ctrl Pts',(-11.8990654189357,-5.80714485919302,
-12.236639786787));
#16805=CARTESIAN_POINT('Ctrl Pts',(-12.1133511332214,-3.44429340467069,
-10.3523286299234));
#16806=CARTESIAN_POINT('Ctrl Pts',(-12.3276368475071,-1.08144195014838,
-8.46801747305969));
#16807=CARTESIAN_POINT('Ctrl Pts',(-12.5419225617929,0.229841679453252,
-5.74510895921687));
#16808=CARTESIAN_POINT('Ctrl Pts',(-12.7562082760786,1.54112530905491,-3.02220044537405));
#16809=CARTESIAN_POINT('Ctrl Pts',(-12.9704939903643,1.5411253090549,0.));
#16810=CARTESIAN_POINT('Ctrl Pts',(-13.18477970465,1.5411253090549,3.02220044537401));
#16811=CARTESIAN_POINT('Ctrl Pts',(-13.3990654189357,0.229841679453252,
5.74510895921686));
#16812=CARTESIAN_POINT('Ctrl Pts',(-13.6133511332214,-1.08144195014837,
8.46801747305969));
#16813=CARTESIAN_POINT('Ctrl Pts',(-13.8276368475071,-3.4442934046707,10.3523286299233));
#16814=CARTESIAN_POINT('Ctrl Pts',(-14.0419225617929,-5.80714485919302,
12.236639786787));
#16815=CARTESIAN_POINT('Ctrl Pts',(-14.2562082760786,-8.75357242959651,
12.9091426524948));
#16816=CARTESIAN_POINT('Ctrl Pts',(-14.4704939903643,-11.7,13.5816455182026));
#16817=CARTESIAN_POINT('Ctrl Pts',(-14.68477970465,-14.6464275704035,12.9091426524948));
#16818=CARTESIAN_POINT('Ctrl Pts',(-14.8990654189357,-17.5928551408069,
12.236639786787));
#16819=CARTESIAN_POINT('Ctrl Pts',(-15.1133511332214,-19.9557065953293,
10.3523286299233));
#16820=CARTESIAN_POINT('Ctrl Pts',(-15.3276368475071,-22.3185580498516,
8.46801747305968));
#16821=CARTESIAN_POINT('Ctrl Pts',(-15.5419225617929,-23.6298416794532,
5.74510895921686));
#16822=CARTESIAN_POINT('Ctrl Pts',(-15.7562082760786,-24.9411253090549,
3.02220044537403));
#16823=CARTESIAN_POINT('Ctrl Pts',(-15.9704939903643,-24.9411253090549,
0.));
#16824=CARTESIAN_POINT('Ctrl Pts',(-16.18477970465,-24.9411253090549,-3.02220044537402));
#16825=CARTESIAN_POINT('Ctrl Pts',(-16.3990654189357,-23.6298416794532,
-5.74510895921687));
#16826=CARTESIAN_POINT('Ctrl Pts',(-16.6133511332214,-22.3185580498516,
-8.4680174730597));
#16827=CARTESIAN_POINT('Ctrl Pts',(-16.8276368475071,-19.9557065953293,
-10.3523286299233));
#16828=CARTESIAN_POINT('Ctrl Pts',(-17.0419225617929,-17.5928551408069,
-12.236639786787));
#16829=CARTESIAN_POINT('Ctrl Pts',(-17.2562082760786,-14.6464275704035,
-12.9091426524948));
#16830=CARTESIAN_POINT('Ctrl Pts',(-17.4704939903643,-11.7,-13.5816455182026));
#16831=CARTESIAN_POINT('Ctrl Pts',(-17.68477970465,-8.75357242959651,-12.9091426524948));
#16832=CARTESIAN_POINT('Ctrl Pts',(-17.8990654189357,-5.80714485919301,
-12.236639786787));
#16833=CARTESIAN_POINT('Ctrl Pts',(-18.1133511332214,-3.4442934046707,-10.3523286299233));
#16834=CARTESIAN_POINT('Ctrl Pts',(-18.3276368475072,-1.08144195014838,
-8.46801747305968));
#16835=CARTESIAN_POINT('Ctrl Pts',(-18.5419225617929,0.229841679453252,
-5.74510895921686));
#16836=CARTESIAN_POINT('Ctrl Pts',(-18.7562082760786,1.5411253090549,-3.02220044537404));
#16837=CARTESIAN_POINT('Ctrl Pts',(-18.9704939903643,1.5411253090549,-3.46944695195361E-15));
#16838=CARTESIAN_POINT('Ctrl Pts',(-19.18477970465,1.5411253090549,3.02220044537403));
#16839=CARTESIAN_POINT('Ctrl Pts',(-19.3990654189357,0.229841679453252,
5.74510895921686));
#16840=CARTESIAN_POINT('Ctrl Pts',(-19.6133511332214,-1.08144195014837,
8.4680174730597));
#16841=CARTESIAN_POINT('Ctrl Pts',(-19.8276368475071,-3.4442934046707,10.3523286299233));
#16842=CARTESIAN_POINT('Ctrl Pts',(-20.0419225617929,-5.80714485919302,
12.236639786787));
#16843=CARTESIAN_POINT('Ctrl Pts',(-20.2562082760786,-8.75357242959651,
12.9091426524948));
#16844=CARTESIAN_POINT('Ctrl Pts',(-20.4704939903643,-11.7,13.5816455182026));
#16845=CARTESIAN_POINT('Ctrl Pts',(-20.68477970465,-14.6464275704035,12.9091426524948));
#16846=CARTESIAN_POINT('Ctrl Pts',(-20.8990654189357,-17.5928551408069,
12.236639786787));
#16847=CARTESIAN_POINT('Ctrl Pts',(-21.1133511332214,-19.9557065953293,
10.3523286299233));
#16848=CARTESIAN_POINT('Ctrl Pts',(-21.3276368475072,-22.3185580498516,
8.4680174730597));
#16849=CARTESIAN_POINT('Ctrl Pts',(-21.5419225617929,-23.6298416794532,
5.74510895921686));
#16850=CARTESIAN_POINT('Ctrl Pts',(-21.7562082760786,-24.9411253090549,
3.02220044537405));
#16851=CARTESIAN_POINT('Ctrl Pts',(-21.9704939903643,-24.9411253090549,
3.46944695195361E-15));
#16852=CARTESIAN_POINT('Ctrl Pts',(-22.18477970465,-24.9411253090549,-3.02220044537404));
#16853=CARTESIAN_POINT('Ctrl Pts',(-22.3990654189357,-23.6298416794532,
-5.74510895921686));
#16854=CARTESIAN_POINT('Ctrl Pts',(-22.6133511332214,-22.3185580498516,
-8.4680174730597));
#16855=CARTESIAN_POINT('Ctrl Pts',(-22.8276368475072,-19.9557065953293,
-10.3523286299233));
#16856=CARTESIAN_POINT('Ctrl Pts',(-23.0419225617929,-17.592855140807,-12.236639786787));
#16857=CARTESIAN_POINT('Ctrl Pts',(-23.2562082760786,-14.6464275704035,
-12.9091426524948));
#16858=CARTESIAN_POINT('Ctrl Pts',(-23.4704939903643,-11.7,-13.5816455182026));
#16859=CARTESIAN_POINT('Ctrl Pts',(-23.68477970465,-8.75357242959651,-12.9091426524948));
#16860=CARTESIAN_POINT('Ctrl Pts',(-23.8990654189357,-5.80714485919301,
-12.236639786787));
#16861=CARTESIAN_POINT('Ctrl Pts',(-24.1133511332214,-3.4442934046707,-10.3523286299233));
#16862=CARTESIAN_POINT('Ctrl Pts',(-24.3276368475071,-1.08144195014838,
-8.46801747305971));
#16863=CARTESIAN_POINT('Ctrl Pts',(-24.5419225617929,0.229841679453259,
-5.74510895921687));
#16864=CARTESIAN_POINT('Ctrl Pts',(-24.7562082760786,1.54112530905491,-3.02220044537405));
#16865=CARTESIAN_POINT('Ctrl Pts',(-24.9704939903643,1.5411253090549,0.));
#16866=CARTESIAN_POINT('Ctrl Pts',(0.970493990364278,1.5411253090549,-1.38777878078145E-14));
#16867=CARTESIAN_POINT('Ctrl Pts',(0.75620827607856,1.5411253090549,3.02220044537401));
#16868=CARTESIAN_POINT('Ctrl Pts',(0.541922561792848,0.229841679453252,
5.74510895921686));
#16869=CARTESIAN_POINT('Ctrl Pts',(0.327636847507131,-1.08144195014837,
8.4680174730597));
#16870=CARTESIAN_POINT('Ctrl Pts',(0.113351133221419,-3.4442934046707,10.3523286299233));
#16871=CARTESIAN_POINT('Ctrl Pts',(-0.100934581064293,-5.80714485919301,
12.236639786787));
#16872=CARTESIAN_POINT('Ctrl Pts',(-0.315220295350009,-8.7535724295965,
12.9091426524948));
#16873=CARTESIAN_POINT('Ctrl Pts',(-0.529506009635726,-11.7,13.5816455182026));
#16874=CARTESIAN_POINT('Ctrl Pts',(-0.743791723921436,-14.6464275704035,
12.9091426524948));
#16875=CARTESIAN_POINT('Ctrl Pts',(-0.958077438207154,-17.592855140807,
12.236639786787));
#16876=CARTESIAN_POINT('Ctrl Pts',(-1.17236315249287,-19.9557065953293,
10.3523286299233));
#16877=CARTESIAN_POINT('Ctrl Pts',(-1.38664886677858,-22.3185580498516,
8.46801747305969));
#16878=CARTESIAN_POINT('Ctrl Pts',(-1.60093458106429,-23.6298416794532,
5.74510895921685));
#16879=CARTESIAN_POINT('Ctrl Pts',(-1.81522029535001,-24.9411253090549,
3.02220044537403));
#16880=CARTESIAN_POINT('Ctrl Pts',(-2.02950600963573,-24.9411253090549,
-6.93889390390723E-15));
#16881=CARTESIAN_POINT('Ctrl Pts',(-2.24379172392144,-24.9411253090549,
-3.02220044537404));
#16882=CARTESIAN_POINT('Ctrl Pts',(-2.45807743820715,-23.6298416794532,
-5.74510895921686));
#16883=CARTESIAN_POINT('Ctrl Pts',(-2.67236315249287,-22.3185580498516,
-8.4680174730597));
#16884=CARTESIAN_POINT('Ctrl Pts',(-2.88664886677858,-19.9557065953293,
-10.3523286299233));
#16885=CARTESIAN_POINT('Ctrl Pts',(-3.1009345810643,-17.592855140807,-12.236639786787));
#16886=CARTESIAN_POINT('Ctrl Pts',(-3.31522029535001,-14.6464275704035,
-12.9091426524948));
#16887=CARTESIAN_POINT('Ctrl Pts',(-3.52950600963573,-11.7,-13.5816455182026));
#16888=CARTESIAN_POINT('Ctrl Pts',(-3.74379172392144,-8.75357242959649,
-12.9091426524948));
#16889=CARTESIAN_POINT('Ctrl Pts',(-3.95807743820716,-5.80714485919301,
-12.236639786787));
#16890=CARTESIAN_POINT('Ctrl Pts',(-4.17236315249286,-3.44429340467069,
-10.3523286299233));
#16891=CARTESIAN_POINT('Ctrl Pts',(-4.38664886677858,-1.08144195014838,
-8.4680174730597));
#16892=CARTESIAN_POINT('Ctrl Pts',(-4.60093458106429,0.229841679453252,
-5.74510895921687));
#16893=CARTESIAN_POINT('Ctrl Pts',(-4.81522029535001,1.5411253090549,-3.02220044537403));
#16894=CARTESIAN_POINT('Ctrl Pts',(-5.02950600963572,1.5411253090549,0.));
#16895=CARTESIAN_POINT('Ctrl Pts',(-5.24379172392144,1.5411253090549,3.02220044537403));
#16896=CARTESIAN_POINT('Ctrl Pts',(-5.45807743820715,0.229841679453252,
5.74510895921686));
#16897=CARTESIAN_POINT('Ctrl Pts',(-5.67236315249287,-1.08144195014838,
8.4680174730597));
#16898=CARTESIAN_POINT('Ctrl Pts',(-5.88664886677858,-3.4442934046707,10.3523286299233));
#16899=CARTESIAN_POINT('Ctrl Pts',(-6.10093458106429,-5.80714485919302,
12.236639786787));
#16900=CARTESIAN_POINT('Ctrl Pts',(-6.31522029535001,-8.75357242959651,
12.9091426524948));
#16901=CARTESIAN_POINT('Ctrl Pts',(-6.52950600963572,-11.7,13.5816455182026));
#16902=CARTESIAN_POINT('Ctrl Pts',(-6.74379172392143,-14.6464275704035,
12.9091426524948));
#16903=CARTESIAN_POINT('Ctrl Pts',(-6.95807743820715,-17.592855140807,12.2366397867869));
#16904=CARTESIAN_POINT('Ctrl Pts',(-7.17236315249286,-19.9557065953293,
10.3523286299233));
#16905=CARTESIAN_POINT('Ctrl Pts',(-7.38664886677858,-22.3185580498516,
8.46801747305969));
#16906=CARTESIAN_POINT('Ctrl Pts',(-7.6009345810643,-23.6298416794532,5.74510895921687));
#16907=CARTESIAN_POINT('Ctrl Pts',(-7.81522029535001,-24.9411253090549,
3.02220044537403));
#16908=CARTESIAN_POINT('Ctrl Pts',(-8.02950600963572,-24.9411253090549,
-1.38777878078145E-14));
#16909=CARTESIAN_POINT('Ctrl Pts',(-8.24379172392144,-24.9411253090549,
-3.02220044537403));
#16910=CARTESIAN_POINT('Ctrl Pts',(-8.45807743820715,-23.6298416794532,
-5.74510895921687));
#16911=CARTESIAN_POINT('Ctrl Pts',(-8.67236315249287,-22.3185580498516,
-8.46801747305971));
#16912=CARTESIAN_POINT('Ctrl Pts',(-8.88664886677859,-19.9557065953293,
-10.3523286299233));
#16913=CARTESIAN_POINT('Ctrl Pts',(-9.10093458106429,-17.592855140807,-12.236639786787));
#16914=CARTESIAN_POINT('Ctrl Pts',(-9.31522029535001,-14.6464275704035,
-12.9091426524948));
#16915=CARTESIAN_POINT('Ctrl Pts',(-9.52950600963572,-11.7,-13.5816455182026));
#16916=CARTESIAN_POINT('Ctrl Pts',(-9.74379172392145,-8.75357242959651,
-12.9091426524948));
#16917=CARTESIAN_POINT('Ctrl Pts',(-9.95807743820715,-5.80714485919301,
-12.236639786787));
#16918=CARTESIAN_POINT('Ctrl Pts',(-10.1723631524929,-3.4442934046707,-10.3523286299233));
#16919=CARTESIAN_POINT('Ctrl Pts',(-10.3866488667786,-1.08144195014838,
-8.4680174730597));
#16920=CARTESIAN_POINT('Ctrl Pts',(-10.6009345810643,0.229841679453252,
-5.74510895921687));
#16921=CARTESIAN_POINT('Ctrl Pts',(-10.81522029535,1.5411253090549,-3.02220044537404));
#16922=CARTESIAN_POINT('Ctrl Pts',(-11.0295060096357,1.5411253090549,3.46944695195361E-15));
#16923=CARTESIAN_POINT('Ctrl Pts',(-11.2437917239215,1.5411253090549,3.02220044537404));
#16924=CARTESIAN_POINT('Ctrl Pts',(-11.4580774382071,0.229841679453252,
5.74510895921686));
#16925=CARTESIAN_POINT('Ctrl Pts',(-11.6723631524929,-1.08144195014838,
8.4680174730597));
#16926=CARTESIAN_POINT('Ctrl Pts',(-11.8866488667786,-3.4442934046707,10.3523286299233));
#16927=CARTESIAN_POINT('Ctrl Pts',(-12.1009345810643,-5.80714485919302,
12.236639786787));
#16928=CARTESIAN_POINT('Ctrl Pts',(-12.31522029535,-8.75357242959651,12.9091426524948));
#16929=CARTESIAN_POINT('Ctrl Pts',(-12.5295060096357,-11.7,13.5816455182026));
#16930=CARTESIAN_POINT('Ctrl Pts',(-12.7437917239214,-14.6464275704035,
12.9091426524948));
#16931=CARTESIAN_POINT('Ctrl Pts',(-12.9580774382072,-17.5928551408069,
12.236639786787));
#16932=CARTESIAN_POINT('Ctrl Pts',(-13.1723631524929,-19.9557065953293,
10.3523286299233));
#16933=CARTESIAN_POINT('Ctrl Pts',(-13.3866488667786,-22.3185580498516,
8.46801747305969));
#16934=CARTESIAN_POINT('Ctrl Pts',(-13.6009345810643,-23.6298416794532,
5.74510895921686));
#16935=CARTESIAN_POINT('Ctrl Pts',(-13.81522029535,-24.9411253090549,3.02220044537403));
#16936=CARTESIAN_POINT('Ctrl Pts',(-14.0295060096357,-24.9411253090549,
-6.93889390390723E-15));
#16937=CARTESIAN_POINT('Ctrl Pts',(-14.2437917239214,-24.9411253090549,
-3.02220044537403));
#16938=CARTESIAN_POINT('Ctrl Pts',(-14.4580774382072,-23.6298416794532,
-5.74510895921687));
#16939=CARTESIAN_POINT('Ctrl Pts',(-14.6723631524929,-22.3185580498516,
-8.4680174730597));
#16940=CARTESIAN_POINT('Ctrl Pts',(-14.8866488667786,-19.9557065953293,
-10.3523286299233));
#16941=CARTESIAN_POINT('Ctrl Pts',(-15.1009345810643,-17.5928551408069,
-12.236639786787));
#16942=CARTESIAN_POINT('Ctrl Pts',(-15.31522029535,-14.6464275704035,-12.9091426524948));
#16943=CARTESIAN_POINT('Ctrl Pts',(-15.5295060096357,-11.7,-13.5816455182026));
#16944=CARTESIAN_POINT('Ctrl Pts',(-15.7437917239214,-8.75357242959651,
-12.9091426524948));
#16945=CARTESIAN_POINT('Ctrl Pts',(-15.9580774382072,-5.80714485919302,
-12.236639786787));
#16946=CARTESIAN_POINT('Ctrl Pts',(-16.1723631524929,-3.4442934046707,-10.3523286299233));
#16947=CARTESIAN_POINT('Ctrl Pts',(-16.3866488667786,-1.08144195014838,
-8.4680174730597));
#16948=CARTESIAN_POINT('Ctrl Pts',(-16.6009345810643,0.229841679453259,
-5.74510895921687));
#16949=CARTESIAN_POINT('Ctrl Pts',(-16.81522029535,1.5411253090549,-3.02220044537405));
#16950=CARTESIAN_POINT('Ctrl Pts',(-17.0295060096357,1.5411253090549,0.));
#16951=CARTESIAN_POINT('Ctrl Pts',(-17.2437917239214,1.5411253090549,3.02220044537402));
#16952=CARTESIAN_POINT('Ctrl Pts',(-17.4580774382072,0.229841679453259,
5.74510895921687));
#16953=CARTESIAN_POINT('Ctrl Pts',(-17.6723631524929,-1.08144195014838,
8.4680174730597));
#16954=CARTESIAN_POINT('Ctrl Pts',(-17.8866488667786,-3.4442934046707,10.3523286299233));
#16955=CARTESIAN_POINT('Ctrl Pts',(-18.1009345810643,-5.80714485919302,
12.236639786787));
#16956=CARTESIAN_POINT('Ctrl Pts',(-18.31522029535,-8.75357242959651,12.9091426524948));
#16957=CARTESIAN_POINT('Ctrl Pts',(-18.5295060096357,-11.7,13.5816455182026));
#16958=CARTESIAN_POINT('Ctrl Pts',(-18.7437917239214,-14.6464275704035,
12.9091426524948));
#16959=CARTESIAN_POINT('Ctrl Pts',(-18.9580774382072,-17.592855140807,12.236639786787));
#16960=CARTESIAN_POINT('Ctrl Pts',(-19.1723631524929,-19.9557065953293,
10.3523286299233));
#16961=CARTESIAN_POINT('Ctrl Pts',(-19.3866488667786,-22.3185580498516,
8.46801747305969));
#16962=CARTESIAN_POINT('Ctrl Pts',(-19.6009345810643,-23.6298416794532,
5.74510895921686));
#16963=CARTESIAN_POINT('Ctrl Pts',(-19.81522029535,-24.9411253090549,3.02220044537404));
#16964=CARTESIAN_POINT('Ctrl Pts',(-20.0295060096357,-24.9411253090549,
-3.46944695195361E-15));
#16965=CARTESIAN_POINT('Ctrl Pts',(-20.2437917239214,-24.9411253090549,
-3.02220044537404));
#16966=CARTESIAN_POINT('Ctrl Pts',(-20.4580774382072,-23.6298416794532,
-5.74510895921686));
#16967=CARTESIAN_POINT('Ctrl Pts',(-20.6723631524929,-22.3185580498516,
-8.4680174730597));
#16968=CARTESIAN_POINT('Ctrl Pts',(-20.8866488667786,-19.9557065953293,
-10.3523286299233));
#16969=CARTESIAN_POINT('Ctrl Pts',(-21.1009345810643,-17.5928551408069,
-12.236639786787));
#16970=CARTESIAN_POINT('Ctrl Pts',(-21.31522029535,-14.6464275704035,-12.9091426524948));
#16971=CARTESIAN_POINT('Ctrl Pts',(-21.5295060096357,-11.7,-13.5816455182026));
#16972=CARTESIAN_POINT('Ctrl Pts',(-21.7437917239214,-8.7535724295965,-12.9091426524948));
#16973=CARTESIAN_POINT('Ctrl Pts',(-21.9580774382072,-5.80714485919302,
-12.236639786787));
#16974=CARTESIAN_POINT('Ctrl Pts',(-22.1723631524929,-3.4442934046707,-10.3523286299234));
#16975=CARTESIAN_POINT('Ctrl Pts',(-22.3866488667786,-1.08144195014838,
-8.4680174730597));
#16976=CARTESIAN_POINT('Ctrl Pts',(-22.6009345810643,0.229841679453252,
-5.74510895921687));
#16977=CARTESIAN_POINT('Ctrl Pts',(-22.81522029535,1.5411253090549,-3.02220044537406));
#16978=CARTESIAN_POINT('Ctrl Pts',(-23.0295060096357,1.5411253090549,0.));
#16979=CARTESIAN_POINT('Ctrl Pts',(1.9,-2.19999999999999,0.));
#16980=CARTESIAN_POINT('Ctrl Pts',(1.68571428571428,-2.20000000000001,2.16831300670642));
#16981=CARTESIAN_POINT('Ctrl Pts',(1.47142857142857,-3.14079575492701,4.12189552161678));
#16982=CARTESIAN_POINT('Ctrl Pts',(1.25714285714285,-4.08159150985404,6.07547803652718));
#16983=CARTESIAN_POINT('Ctrl Pts',(1.04285714285714,-5.77684688234202,7.42739908344627));
#16984=CARTESIAN_POINT('Ctrl Pts',(0.828571428571428,-7.47210225483002,
8.77932013036537));
#16985=CARTESIAN_POINT('Ctrl Pts',(0.61428571428571,-9.58605112741501,9.26181516572732));
#16986=CARTESIAN_POINT('Ctrl Pts',(0.399999999999996,-11.7,9.74431020108925));
#16987=CARTESIAN_POINT('Ctrl Pts',(0.185714285714286,-13.813948872585,9.26181516572731));
#16988=CARTESIAN_POINT('Ctrl Pts',(-0.028571428571431,-15.92789774517,8.77932013036537));
#16989=CARTESIAN_POINT('Ctrl Pts',(-0.242857142857143,-17.6231531176579,
7.42739908344628));
#16990=CARTESIAN_POINT('Ctrl Pts',(-0.457142857142861,-19.3184084901459,
6.07547803652717));
#16991=CARTESIAN_POINT('Ctrl Pts',(-0.671428571428574,-20.259204245073,
4.1218955216168));
#16992=CARTESIAN_POINT('Ctrl Pts',(-0.885714285714288,-21.2,2.16831300670641));
#16993=CARTESIAN_POINT('Ctrl Pts',(-1.1,-21.2,0.));
#16994=CARTESIAN_POINT('Ctrl Pts',(-1.31428571428572,-21.2,-2.16831300670643));
#16995=CARTESIAN_POINT('Ctrl Pts',(-1.52857142857143,-20.259204245073,-4.12189552161681));
#16996=CARTESIAN_POINT('Ctrl Pts',(-1.74285714285715,-19.3184084901459,
-6.07547803652718));
#16997=CARTESIAN_POINT('Ctrl Pts',(-1.95714285714286,-17.6231531176579,
-7.42739908344627));
#16998=CARTESIAN_POINT('Ctrl Pts',(-2.17142857142858,-15.92789774517,-8.77932013036537));
#16999=CARTESIAN_POINT('Ctrl Pts',(-2.38571428571429,-13.813948872585,-9.26181516572734));
#17000=CARTESIAN_POINT('Ctrl Pts',(-2.6,-11.7,-9.74431020108928));
#17001=CARTESIAN_POINT('Ctrl Pts',(-2.81428571428572,-9.58605112741501,
-9.26181516572733));
#17002=CARTESIAN_POINT('Ctrl Pts',(-3.02857142857143,-7.47210225483002,
-8.77932013036539));
#17003=CARTESIAN_POINT('Ctrl Pts',(-3.24285714285714,-5.77684688234203,
-7.42739908344628));
#17004=CARTESIAN_POINT('Ctrl Pts',(-3.45714285714286,-4.08159150985404,
-6.07547803652718));
#17005=CARTESIAN_POINT('Ctrl Pts',(-3.67142857142857,-3.14079575492701,
-4.12189552161681));
#17006=CARTESIAN_POINT('Ctrl Pts',(-3.88571428571429,-2.2,-2.16831300670643));
#17007=CARTESIAN_POINT('Ctrl Pts',(-4.1,-2.2,0.));
#17008=CARTESIAN_POINT('Ctrl Pts',(-4.31428571428572,-2.2,2.16831300670642));
#17009=CARTESIAN_POINT('Ctrl Pts',(-4.52857142857143,-3.14079575492702,
4.1218955216168));
#17010=CARTESIAN_POINT('Ctrl Pts',(-4.74285714285714,-4.08159150985404,
6.07547803652717));
#17011=CARTESIAN_POINT('Ctrl Pts',(-4.95714285714286,-5.77684688234202,
7.42739908344626));
#17012=CARTESIAN_POINT('Ctrl Pts',(-5.17142857142857,-7.47210225483002,
8.77932013036537));
#17013=CARTESIAN_POINT('Ctrl Pts',(-5.38571428571428,-9.58605112741501,
9.26181516572731));
#17014=CARTESIAN_POINT('Ctrl Pts',(-5.6,-11.7,9.74431020108925));
#17015=CARTESIAN_POINT('Ctrl Pts',(-5.81428571428572,-13.813948872585,9.26181516572731));
#17016=CARTESIAN_POINT('Ctrl Pts',(-6.02857142857143,-15.9278977451699,
8.77932013036537));
#17017=CARTESIAN_POINT('Ctrl Pts',(-6.24285714285714,-17.623153117658,7.42739908344628));
#17018=CARTESIAN_POINT('Ctrl Pts',(-6.45714285714286,-19.318408490146,6.07547803652718));
#17019=CARTESIAN_POINT('Ctrl Pts',(-6.67142857142857,-20.259204245073,4.12189552161679));
#17020=CARTESIAN_POINT('Ctrl Pts',(-6.88571428571429,-21.2,2.16831300670641));
#17021=CARTESIAN_POINT('Ctrl Pts',(-7.1,-21.2,-1.04083408558608E-14));
#17022=CARTESIAN_POINT('Ctrl Pts',(-7.31428571428571,-21.2,-2.16831300670643));
#17023=CARTESIAN_POINT('Ctrl Pts',(-7.52857142857143,-20.259204245073,-4.1218955216168));
#17024=CARTESIAN_POINT('Ctrl Pts',(-7.74285714285714,-19.3184084901459,
-6.07547803652717));
#17025=CARTESIAN_POINT('Ctrl Pts',(-7.95714285714286,-17.6231531176579,
-7.42739908344627));
#17026=CARTESIAN_POINT('Ctrl Pts',(-8.17142857142857,-15.92789774517,-8.77932013036537));
#17027=CARTESIAN_POINT('Ctrl Pts',(-8.38571428571429,-13.813948872585,-9.26181516572732));
#17028=CARTESIAN_POINT('Ctrl Pts',(-8.6,-11.7,-9.74431020108926));
#17029=CARTESIAN_POINT('Ctrl Pts',(-8.81428571428571,-9.586051127415,-9.26181516572733));
#17030=CARTESIAN_POINT('Ctrl Pts',(-9.02857142857144,-7.47210225483002,
-8.77932013036538));
#17031=CARTESIAN_POINT('Ctrl Pts',(-9.24285714285714,-5.77684688234203,
-7.42739908344628));
#17032=CARTESIAN_POINT('Ctrl Pts',(-9.45714285714286,-4.08159150985404,
-6.07547803652718));
#17033=CARTESIAN_POINT('Ctrl Pts',(-9.67142857142858,-3.14079575492702,
-4.12189552161681));
#17034=CARTESIAN_POINT('Ctrl Pts',(-9.88571428571429,-2.19999999999999,
-2.16831300670644));
#17035=CARTESIAN_POINT('Ctrl Pts',(-10.1,-2.19999999999999,0.));
#17036=CARTESIAN_POINT('Ctrl Pts',(-10.3142857142857,-2.19999999999999,
2.16831300670642));
#17037=CARTESIAN_POINT('Ctrl Pts',(-10.5285714285714,-3.14079575492701,
4.1218955216168));
#17038=CARTESIAN_POINT('Ctrl Pts',(-10.7428571428571,-4.08159150985404,
6.07547803652716));
#17039=CARTESIAN_POINT('Ctrl Pts',(-10.9571428571429,-5.77684688234203,
7.42739908344628));
#17040=CARTESIAN_POINT('Ctrl Pts',(-11.1714285714286,-7.47210225483001,
8.77932013036537));
#17041=CARTESIAN_POINT('Ctrl Pts',(-11.3857142857143,-9.58605112741501,
9.26181516572731));
#17042=CARTESIAN_POINT('Ctrl Pts',(-11.6,-11.7,9.74431020108925));
#17043=CARTESIAN_POINT('Ctrl Pts',(-11.8142857142857,-13.813948872585,9.26181516572731));
#17044=CARTESIAN_POINT('Ctrl Pts',(-12.0285714285714,-15.92789774517,8.77932013036537));
#17045=CARTESIAN_POINT('Ctrl Pts',(-12.2428571428572,-17.6231531176579,
7.42739908344627));
#17046=CARTESIAN_POINT('Ctrl Pts',(-12.4571428571429,-19.3184084901459,
6.07547803652716));
#17047=CARTESIAN_POINT('Ctrl Pts',(-12.6714285714286,-20.259204245073,4.12189552161679));
#17048=CARTESIAN_POINT('Ctrl Pts',(-12.8857142857143,-21.2,2.16831300670642));
#17049=CARTESIAN_POINT('Ctrl Pts',(-13.1,-21.2,-6.93889390390723E-15));
#17050=CARTESIAN_POINT('Ctrl Pts',(-13.3142857142857,-21.2,-2.16831300670643));
#17051=CARTESIAN_POINT('Ctrl Pts',(-13.5285714285714,-20.259204245073,-4.1218955216168));
#17052=CARTESIAN_POINT('Ctrl Pts',(-13.7428571428571,-19.318408490146,-6.07547803652717));
#17053=CARTESIAN_POINT('Ctrl Pts',(-13.9571428571429,-17.623153117658,-7.42739908344627));
#17054=CARTESIAN_POINT('Ctrl Pts',(-14.1714285714286,-15.92789774517,-8.77932013036538));
#17055=CARTESIAN_POINT('Ctrl Pts',(-14.3857142857143,-13.813948872585,-9.26181516572733));
#17056=CARTESIAN_POINT('Ctrl Pts',(-14.6,-11.7,-9.74431020108926));
#17057=CARTESIAN_POINT('Ctrl Pts',(-14.8142857142857,-9.58605112741501,
-9.26181516572732));
#17058=CARTESIAN_POINT('Ctrl Pts',(-15.0285714285714,-7.47210225483002,
-8.77932013036538));
#17059=CARTESIAN_POINT('Ctrl Pts',(-15.2428571428571,-5.77684688234203,
-7.42739908344628));
#17060=CARTESIAN_POINT('Ctrl Pts',(-15.4571428571429,-4.08159150985402,
-6.07547803652717));
#17061=CARTESIAN_POINT('Ctrl Pts',(-15.6714285714286,-3.14079575492701,
-4.12189552161682));
#17062=CARTESIAN_POINT('Ctrl Pts',(-15.8857142857143,-2.19999999999999,
-2.16831300670642));
#17063=CARTESIAN_POINT('Ctrl Pts',(-16.1,-2.20000000000001,-1.38777878078145E-14));
#17064=CARTESIAN_POINT('Ctrl Pts',(-16.3142857142857,-2.19999999999998,
2.16831300670643));
#17065=CARTESIAN_POINT('Ctrl Pts',(-16.5285714285714,-3.14079575492701,
4.12189552161679));
#17066=CARTESIAN_POINT('Ctrl Pts',(-16.7428571428571,-4.08159150985404,
6.07547803652718));
#17067=CARTESIAN_POINT('Ctrl Pts',(-16.9571428571429,-5.77684688234202,
7.42739908344626));
#17068=CARTESIAN_POINT('Ctrl Pts',(-17.1714285714286,-7.47210225483001,
8.77932013036537));
#17069=CARTESIAN_POINT('Ctrl Pts',(-17.3857142857143,-9.58605112741501,
9.26181516572732));
#17070=CARTESIAN_POINT('Ctrl Pts',(-17.6,-11.7,9.74431020108925));
#17071=CARTESIAN_POINT('Ctrl Pts',(-17.8142857142857,-13.813948872585,9.26181516572732));
#17072=CARTESIAN_POINT('Ctrl Pts',(-18.0285714285714,-15.92789774517,8.77932013036538));
#17073=CARTESIAN_POINT('Ctrl Pts',(-18.2428571428571,-17.623153117658,7.42739908344627));
#17074=CARTESIAN_POINT('Ctrl Pts',(-18.4571428571429,-19.318408490146,6.07547803652718));
#17075=CARTESIAN_POINT('Ctrl Pts',(-18.6714285714286,-20.259204245073,4.12189552161679));
#17076=CARTESIAN_POINT('Ctrl Pts',(-18.8857142857143,-21.2,2.16831300670641));
#17077=CARTESIAN_POINT('Ctrl Pts',(-19.1,-21.2,-1.38777878078145E-14));
#17078=CARTESIAN_POINT('Ctrl Pts',(-19.3142857142857,-21.2,-2.16831300670643));
#17079=CARTESIAN_POINT('Ctrl Pts',(-19.5285714285714,-20.259204245073,-4.12189552161681));
#17080=CARTESIAN_POINT('Ctrl Pts',(-19.7428571428572,-19.3184084901459,
-6.07547803652717));
#17081=CARTESIAN_POINT('Ctrl Pts',(-19.9571428571429,-17.623153117658,-7.42739908344628));
#17082=CARTESIAN_POINT('Ctrl Pts',(-20.1714285714286,-15.92789774517,-8.77932013036539));
#17083=CARTESIAN_POINT('Ctrl Pts',(-20.3857142857143,-13.813948872585,-9.26181516572732));
#17084=CARTESIAN_POINT('Ctrl Pts',(-20.6,-11.7,-9.74431020108926));
#17085=CARTESIAN_POINT('Ctrl Pts',(-20.8142857142857,-9.58605112741501,
-9.26181516572732));
#17086=CARTESIAN_POINT('Ctrl Pts',(-21.0285714285714,-7.47210225483001,
-8.77932013036538));
#17087=CARTESIAN_POINT('Ctrl Pts',(-21.2428571428572,-5.77684688234203,
-7.42739908344628));
#17088=CARTESIAN_POINT('Ctrl Pts',(-21.4571428571429,-4.08159150985402,
-6.07547803652718));
#17089=CARTESIAN_POINT('Ctrl Pts',(-21.6714285714286,-3.14079575492701,
-4.1218955216168));
#17090=CARTESIAN_POINT('Ctrl Pts',(-21.8857142857143,-2.20000000000001,
-2.16831300670643));
#17091=CARTESIAN_POINT('Ctrl Pts',(-22.1,-2.20000000000001,-2.08166817117217E-14));
#17092=CARTESIAN_POINT('Ctrl Pts',(0.970493990364278,1.5411253090549,-1.38777878078145E-14));
#17093=CARTESIAN_POINT('Ctrl Pts',(0.75620827607856,1.5411253090549,3.02220044537401));
#17094=CARTESIAN_POINT('Ctrl Pts',(0.541922561792848,0.229841679453252,
5.74510895921686));
#17095=CARTESIAN_POINT('Ctrl Pts',(0.327636847507131,-1.08144195014837,
8.4680174730597));
#17096=CARTESIAN_POINT('Ctrl Pts',(0.113351133221419,-3.4442934046707,10.3523286299233));
#17097=CARTESIAN_POINT('Ctrl Pts',(-0.100934581064293,-5.80714485919301,
12.236639786787));
#17098=CARTESIAN_POINT('Ctrl Pts',(-0.315220295350009,-8.7535724295965,
12.9091426524948));
#17099=CARTESIAN_POINT('Ctrl Pts',(-0.529506009635726,-11.7,13.5816455182026));
#17100=CARTESIAN_POINT('Ctrl Pts',(-0.743791723921436,-14.6464275704035,
12.9091426524948));
#17101=CARTESIAN_POINT('Ctrl Pts',(-0.958077438207154,-17.592855140807,
12.236639786787));
#17102=CARTESIAN_POINT('Ctrl Pts',(-1.17236315249287,-19.9557065953293,
10.3523286299233));
#17103=CARTESIAN_POINT('Ctrl Pts',(-1.38664886677858,-22.3185580498516,
8.46801747305969));
#17104=CARTESIAN_POINT('Ctrl Pts',(-1.60093458106429,-23.6298416794532,
5.74510895921685));
#17105=CARTESIAN_POINT('Ctrl Pts',(-1.81522029535001,-24.9411253090549,
3.02220044537403));
#17106=CARTESIAN_POINT('Ctrl Pts',(-2.02950600963573,-24.9411253090549,
-6.93889390390723E-15));
#17107=CARTESIAN_POINT('Ctrl Pts',(-2.24379172392144,-24.9411253090549,
-3.02220044537404));
#17108=CARTESIAN_POINT('Ctrl Pts',(-2.45807743820715,-23.6298416794532,
-5.74510895921686));
#17109=CARTESIAN_POINT('Ctrl Pts',(-2.67236315249287,-22.3185580498516,
-8.4680174730597));
#17110=CARTESIAN_POINT('Ctrl Pts',(-2.88664886677858,-19.9557065953293,
-10.3523286299233));
#17111=CARTESIAN_POINT('Ctrl Pts',(-3.1009345810643,-17.592855140807,-12.236639786787));
#17112=CARTESIAN_POINT('Ctrl Pts',(-3.31522029535001,-14.6464275704035,
-12.9091426524948));
#17113=CARTESIAN_POINT('Ctrl Pts',(-3.52950600963573,-11.7,-13.5816455182026));
#17114=CARTESIAN_POINT('Ctrl Pts',(-3.74379172392144,-8.75357242959649,
-12.9091426524948));
#17115=CARTESIAN_POINT('Ctrl Pts',(-3.95807743820716,-5.80714485919301,
-12.236639786787));
#17116=CARTESIAN_POINT('Ctrl Pts',(-4.17236315249286,-3.44429340467069,
-10.3523286299233));
#17117=CARTESIAN_POINT('Ctrl Pts',(-4.38664886677858,-1.08144195014838,
-8.4680174730597));
#17118=CARTESIAN_POINT('Ctrl Pts',(-4.60093458106429,0.229841679453252,
-5.74510895921687));
#17119=CARTESIAN_POINT('Ctrl Pts',(-4.81522029535001,1.5411253090549,-3.02220044537403));
#17120=CARTESIAN_POINT('Ctrl Pts',(-5.02950600963572,1.5411253090549,0.));
#17121=CARTESIAN_POINT('Ctrl Pts',(-5.24379172392144,1.5411253090549,3.02220044537403));
#17122=CARTESIAN_POINT('Ctrl Pts',(-5.45807743820715,0.229841679453252,
5.74510895921686));
#17123=CARTESIAN_POINT('Ctrl Pts',(-5.67236315249287,-1.08144195014838,
8.4680174730597));
#17124=CARTESIAN_POINT('Ctrl Pts',(-5.88664886677858,-3.4442934046707,10.3523286299233));
#17125=CARTESIAN_POINT('Ctrl Pts',(-6.10093458106429,-5.80714485919302,
12.236639786787));
#17126=CARTESIAN_POINT('Ctrl Pts',(-6.31522029535001,-8.75357242959651,
12.9091426524948));
#17127=CARTESIAN_POINT('Ctrl Pts',(-6.52950600963572,-11.7,13.5816455182026));
#17128=CARTESIAN_POINT('Ctrl Pts',(-6.74379172392143,-14.6464275704035,
12.9091426524948));
#17129=CARTESIAN_POINT('Ctrl Pts',(-6.95807743820715,-17.592855140807,12.2366397867869));
#17130=CARTESIAN_POINT('Ctrl Pts',(-7.17236315249286,-19.9557065953293,
10.3523286299233));
#17131=CARTESIAN_POINT('Ctrl Pts',(-7.38664886677858,-22.3185580498516,
8.46801747305969));
#17132=CARTESIAN_POINT('Ctrl Pts',(-7.6009345810643,-23.6298416794532,5.74510895921687));
#17133=CARTESIAN_POINT('Ctrl Pts',(-7.81522029535001,-24.9411253090549,
3.02220044537403));
#17134=CARTESIAN_POINT('Ctrl Pts',(-8.02950600963572,-24.9411253090549,
-1.38777878078145E-14));
#17135=CARTESIAN_POINT('Ctrl Pts',(-8.24379172392144,-24.9411253090549,
-3.02220044537403));
#17136=CARTESIAN_POINT('Ctrl Pts',(-8.45807743820715,-23.6298416794532,
-5.74510895921687));
#17137=CARTESIAN_POINT('Ctrl Pts',(-8.67236315249287,-22.3185580498516,
-8.46801747305971));
#17138=CARTESIAN_POINT('Ctrl Pts',(-8.88664886677859,-19.9557065953293,
-10.3523286299233));
#17139=CARTESIAN_POINT('Ctrl Pts',(-9.10093458106429,-17.592855140807,-12.236639786787));
#17140=CARTESIAN_POINT('Ctrl Pts',(-9.31522029535001,-14.6464275704035,
-12.9091426524948));
#17141=CARTESIAN_POINT('Ctrl Pts',(-9.52950600963572,-11.7,-13.5816455182026));
#17142=CARTESIAN_POINT('Ctrl Pts',(-9.74379172392145,-8.75357242959651,
-12.9091426524948));
#17143=CARTESIAN_POINT('Ctrl Pts',(-9.95807743820715,-5.80714485919301,
-12.236639786787));
#17144=CARTESIAN_POINT('Ctrl Pts',(-10.1723631524929,-3.4442934046707,-10.3523286299233));
#17145=CARTESIAN_POINT('Ctrl Pts',(-10.3866488667786,-1.08144195014838,
-8.4680174730597));
#17146=CARTESIAN_POINT('Ctrl Pts',(-10.6009345810643,0.229841679453252,
-5.74510895921687));
#17147=CARTESIAN_POINT('Ctrl Pts',(-10.81522029535,1.5411253090549,-3.02220044537404));
#17148=CARTESIAN_POINT('Ctrl Pts',(-11.0295060096357,1.5411253090549,3.46944695195361E-15));
#17149=CARTESIAN_POINT('Ctrl Pts',(-11.2437917239214,1.5411253090549,3.02220044537404));
#17150=CARTESIAN_POINT('Ctrl Pts',(-11.4580774382071,0.229841679453252,
5.74510895921686));
#17151=CARTESIAN_POINT('Ctrl Pts',(-11.6723631524929,-1.08144195014838,
8.4680174730597));
#17152=CARTESIAN_POINT('Ctrl Pts',(-11.8866488667786,-3.4442934046707,10.3523286299233));
#17153=CARTESIAN_POINT('Ctrl Pts',(-12.1009345810643,-5.80714485919302,
12.236639786787));
#17154=CARTESIAN_POINT('Ctrl Pts',(-12.31522029535,-8.75357242959651,12.9091426524948));
#17155=CARTESIAN_POINT('Ctrl Pts',(-12.5295060096357,-11.7,13.5816455182026));
#17156=CARTESIAN_POINT('Ctrl Pts',(-12.7437917239214,-14.6464275704035,
12.9091426524948));
#17157=CARTESIAN_POINT('Ctrl Pts',(-12.9580774382071,-17.5928551408069,
12.236639786787));
#17158=CARTESIAN_POINT('Ctrl Pts',(-13.1723631524929,-19.9557065953293,
10.3523286299233));
#17159=CARTESIAN_POINT('Ctrl Pts',(-13.3866488667786,-22.3185580498516,
8.46801747305969));
#17160=CARTESIAN_POINT('Ctrl Pts',(-13.6009345810643,-23.6298416794532,
5.74510895921686));
#17161=CARTESIAN_POINT('Ctrl Pts',(-13.81522029535,-24.9411253090549,3.02220044537403));
#17162=CARTESIAN_POINT('Ctrl Pts',(-14.0295060096357,-24.9411253090549,
-6.93889390390723E-15));
#17163=CARTESIAN_POINT('Ctrl Pts',(-14.2437917239214,-24.9411253090549,
-3.02220044537403));
#17164=CARTESIAN_POINT('Ctrl Pts',(-14.4580774382072,-23.6298416794532,
-5.74510895921687));
#17165=CARTESIAN_POINT('Ctrl Pts',(-14.6723631524929,-22.3185580498516,
-8.4680174730597));
#17166=CARTESIAN_POINT('Ctrl Pts',(-14.8866488667786,-19.9557065953293,
-10.3523286299233));
#17167=CARTESIAN_POINT('Ctrl Pts',(-15.1009345810643,-17.5928551408069,
-12.236639786787));
#17168=CARTESIAN_POINT('Ctrl Pts',(-15.31522029535,-14.6464275704035,-12.9091426524948));
#17169=CARTESIAN_POINT('Ctrl Pts',(-15.5295060096357,-11.7,-13.5816455182026));
#17170=CARTESIAN_POINT('Ctrl Pts',(-15.7437917239214,-8.75357242959651,
-12.9091426524948));
#17171=CARTESIAN_POINT('Ctrl Pts',(-15.9580774382072,-5.80714485919302,
-12.236639786787));
#17172=CARTESIAN_POINT('Ctrl Pts',(-16.1723631524929,-3.4442934046707,-10.3523286299233));
#17173=CARTESIAN_POINT('Ctrl Pts',(-16.3866488667786,-1.08144195014838,
-8.4680174730597));
#17174=CARTESIAN_POINT('Ctrl Pts',(-16.6009345810643,0.229841679453259,
-5.74510895921687));
#17175=CARTESIAN_POINT('Ctrl Pts',(-16.81522029535,1.5411253090549,-3.02220044537405));
#17176=CARTESIAN_POINT('Ctrl Pts',(-17.0295060096357,1.5411253090549,0.));
#17177=CARTESIAN_POINT('Ctrl Pts',(-17.2437917239215,1.5411253090549,3.02220044537402));
#17178=CARTESIAN_POINT('Ctrl Pts',(-17.4580774382072,0.229841679453259,
5.74510895921687));
#17179=CARTESIAN_POINT('Ctrl Pts',(-17.6723631524929,-1.08144195014838,
8.4680174730597));
#17180=CARTESIAN_POINT('Ctrl Pts',(-17.8866488667786,-3.4442934046707,10.3523286299233));
#17181=CARTESIAN_POINT('Ctrl Pts',(-18.1009345810643,-5.80714485919302,
12.236639786787));
#17182=CARTESIAN_POINT('Ctrl Pts',(-18.31522029535,-8.75357242959651,12.9091426524948));
#17183=CARTESIAN_POINT('Ctrl Pts',(-18.5295060096357,-11.7,13.5816455182026));
#17184=CARTESIAN_POINT('Ctrl Pts',(-18.7437917239214,-14.6464275704035,
12.9091426524948));
#17185=CARTESIAN_POINT('Ctrl Pts',(-18.9580774382072,-17.592855140807,12.236639786787));
#17186=CARTESIAN_POINT('Ctrl Pts',(-19.1723631524929,-19.9557065953293,
10.3523286299233));
#17187=CARTESIAN_POINT('Ctrl Pts',(-19.3866488667786,-22.3185580498516,
8.46801747305969));
#17188=CARTESIAN_POINT('Ctrl Pts',(-19.6009345810643,-23.6298416794532,
5.74510895921686));
#17189=CARTESIAN_POINT('Ctrl Pts',(-19.81522029535,-24.9411253090549,3.02220044537404));
#17190=CARTESIAN_POINT('Ctrl Pts',(-20.0295060096357,-24.9411253090549,
-3.46944695195361E-15));
#17191=CARTESIAN_POINT('Ctrl Pts',(-20.2437917239214,-24.9411253090549,
-3.02220044537404));
#17192=CARTESIAN_POINT('Ctrl Pts',(-20.4580774382072,-23.6298416794532,
-5.74510895921686));
#17193=CARTESIAN_POINT('Ctrl Pts',(-20.6723631524929,-22.3185580498516,
-8.4680174730597));
#17194=CARTESIAN_POINT('Ctrl Pts',(-20.8866488667786,-19.9557065953293,
-10.3523286299233));
#17195=CARTESIAN_POINT('Ctrl Pts',(-21.1009345810643,-17.5928551408069,
-12.236639786787));
#17196=CARTESIAN_POINT('Ctrl Pts',(-21.31522029535,-14.6464275704035,-12.9091426524948));
#17197=CARTESIAN_POINT('Ctrl Pts',(-21.5295060096357,-11.7,-13.5816455182026));
#17198=CARTESIAN_POINT('Ctrl Pts',(-21.7437917239214,-8.7535724295965,-12.9091426524948));
#17199=CARTESIAN_POINT('Ctrl Pts',(-21.9580774382072,-5.80714485919302,
-12.236639786787));
#17200=CARTESIAN_POINT('Ctrl Pts',(-22.1723631524929,-3.4442934046707,-10.3523286299234));
#17201=CARTESIAN_POINT('Ctrl Pts',(-22.3866488667786,-1.08144195014838,
-8.4680174730597));
#17202=CARTESIAN_POINT('Ctrl Pts',(-22.6009345810643,0.229841679453252,
-5.74510895921687));
#17203=CARTESIAN_POINT('Ctrl Pts',(-22.81522029535,1.5411253090549,-3.02220044537406));
#17204=CARTESIAN_POINT('Ctrl Pts',(-23.0295060096357,1.5411253090549,0.));
#17205=CARTESIAN_POINT('Origin',(128.,-11.7,-3.46944695195361E-15));
#17206=CARTESIAN_POINT('',(128.,-5.19999999999998,-1.62500000000002));
#17207=CARTESIAN_POINT('',(128.,-5.19999999999998,-1.62500000000002));
#17208=CARTESIAN_POINT('',(128.,-5.19999999999998,1.62499999999999));
#17209=CARTESIAN_POINT('',(128.,-5.19999999999998,1.62499999999999));
#17210=CARTESIAN_POINT('',(128.,-5.19999999999998,1.62499999999999));
#17211=CARTESIAN_POINT('Origin',(108.,-5.19999999999998,-1.625));
#17212=CARTESIAN_POINT('',(108.,-5.19999999999998,-1.625));
#17213=CARTESIAN_POINT('',(108.,-5.19999999999998,-1.625));
#17214=CARTESIAN_POINT('',(108.,-5.19999999999998,-1.625));
#17215=CARTESIAN_POINT('Origin',(108.,-5.19999999999998,1.62499999999999));
#17216=CARTESIAN_POINT('',(108.,-5.19999999999998,1.62499999999999));
#17217=CARTESIAN_POINT('',(108.,-5.19999999999998,1.62499999999999));
#17218=CARTESIAN_POINT('',(108.,-5.19999999999998,1.62499999999999));
#17219=CARTESIAN_POINT('Origin',(108.,-5.19999999999998,1.62499999999999));
#17220=CARTESIAN_POINT('',(108.,-5.19999999999998,1.62499999999999));
#17221=CARTESIAN_POINT('Origin',(108.,0.,6.93889390390723E-15));
#17222=CARTESIAN_POINT('Origin',(-58.,-11.7,0.));
#17223=CARTESIAN_POINT('',(0.,0.,0.));
#17224=CARTESIAN_POINT('Origin',(0.,0.,0.));
#17225=CARTESIAN_POINT('',(0.499999999999973,9.12361865364679E-16,-7.45));
#17226=CARTESIAN_POINT('',(0.499999999999979,-9.12361865364683E-16,7.45000000000001));
#17227=CARTESIAN_POINT('Origin',(0.499999999999973,-6.93889390390723E-15,
5.20417042793042E-15));
#17228=CARTESIAN_POINT('Origin',(0.499999999999973,-6.93889390390723E-15,
5.20417042793042E-15));
#17229=CARTESIAN_POINT('',(-2.67390226427335E-16,-8.51129525407326E-16,
6.95000000000004));
#17230=CARTESIAN_POINT('',(-4.11193746846455E-30,-8.51129525407326E-16,
6.95000000000004));
#17231=CARTESIAN_POINT('Origin',(0.,0.,0.));
#17232=CARTESIAN_POINT('Origin',(78.,-8.67361737988404E-15,6.93889390390723E-15));
#17233=CARTESIAN_POINT('',(52.7,-9.59210247924465E-15,-7.49999999999999));
#17234=CARTESIAN_POINT('Origin',(52.7,-8.67361737988404E-15,6.93889390390723E-15));
#17235=CARTESIAN_POINT('',(78.,-9.59210247924465E-15,-7.49999999999999));
#17236=CARTESIAN_POINT('',(78.,-9.59210247924465E-15,-7.49999999999999));
#17237=CARTESIAN_POINT('Origin',(78.,-8.67361737988404E-15,6.93889390390723E-15));
#17238=CARTESIAN_POINT('Origin',(52.7,-8.67361737988404E-15,6.93889390390723E-15));
#17239=CARTESIAN_POINT('',(52.7,14.1421356237309,5.00000000000001));
#17240=CARTESIAN_POINT('',(52.7,14.1421356237309,-4.99999999999999));
#17241=CARTESIAN_POINT('Origin',(52.7,-8.67361737988404E-15,6.93889390390723E-15));
#17242=CARTESIAN_POINT('',(30.,14.1421356237309,5.00000000000001));
#17243=CARTESIAN_POINT('',(52.7,14.1421356237309,5.00000000000001));
#17244=CARTESIAN_POINT('',(30.,14.142135623731,-4.99999999999999));
#17245=CARTESIAN_POINT('Origin',(30.,-6.93889390390723E-15,6.93889390390723E-15));
#17246=CARTESIAN_POINT('',(52.7,14.1421356237309,-4.99999999999999));
#17247=CARTESIAN_POINT('Origin',(0.,0.,0.));
#17248=CARTESIAN_POINT('',(30.,-9.12361865364874E-16,-7.45));
#17249=CARTESIAN_POINT('',(4.4077603079224E-30,-9.12361865364874E-16,-7.45));
#17250=CARTESIAN_POINT('Origin',(30.,-6.93889390390723E-15,6.93889390390723E-15));
#17251=CARTESIAN_POINT('Origin',(118.,0.,0.));
#17252=CARTESIAN_POINT('',(78.,-7.65404249467176E-16,-6.25));
#17253=CARTESIAN_POINT('Origin',(78.,-8.67361737988404E-15,6.93889390390723E-15));
#17254=CARTESIAN_POINT('',(118.,-7.65404249467176E-16,-6.25));
#17255=CARTESIAN_POINT('',(118.,-7.65404249467176E-16,-6.25));
#17256=CARTESIAN_POINT('',(118.,6.03505385228666,1.625));
#17257=CARTESIAN_POINT('Origin',(118.,0.,0.));
#17258=CARTESIAN_POINT('',(88.,6.03505385228665,1.625));
#17259=CARTESIAN_POINT('',(118.,6.03505385228666,1.625));
#17260=CARTESIAN_POINT('',(88.,6.03505385228665,-1.625));
#17261=CARTESIAN_POINT('Origin',(88.,-6.93889390390723E-15,3.46944695195361E-15));
#17262=CARTESIAN_POINT('',(118.,6.03505385228666,-1.625));
#17263=CARTESIAN_POINT('',(118.,6.03505385228666,-1.625));
#17264=CARTESIAN_POINT('Origin',(118.,0.,0.));
#17265=CARTESIAN_POINT('Origin',(118.,0.,0.));
#17266=CARTESIAN_POINT('',(118.,5.5,1.625));
#17267=CARTESIAN_POINT('',(118.,5.5,-1.62499999999999));
#17268=CARTESIAN_POINT('',(118.,5.5,0.));
#17269=CARTESIAN_POINT('',(118.,-3.46944695195361E-15,1.625));
#17270=CARTESIAN_POINT('',(118.,-1.73472347597681E-15,-1.625));
#17271=CARTESIAN_POINT('Origin',(0.,0.,0.));
#17272=CARTESIAN_POINT('Origin',(52.7,-5.20417042793042E-15,5.00000000000001));
#17273=CARTESIAN_POINT('',(30.,11.,5.00000000000001));
#17274=CARTESIAN_POINT('',(30.,-6.93889390390723E-15,5.00000000000001));
#17275=CARTESIAN_POINT('',(52.7,11.,5.00000000000001));
#17276=CARTESIAN_POINT('',(52.7,-5.20417042793042E-15,5.00000000000001));
#17277=CARTESIAN_POINT('',(52.7,11.,5.00000000000001));
#17278=CARTESIAN_POINT('Origin',(52.7,-5.20417042793042E-15,-4.99999999999999));
#17279=CARTESIAN_POINT('',(30.,11.,-4.99999999999999));
#17280=CARTESIAN_POINT('',(30.,-5.20417042793042E-15,-4.99999999999999));
#17281=CARTESIAN_POINT('',(52.7,11.,-4.99999999999999));
#17282=CARTESIAN_POINT('',(52.7,11.,-4.99999999999999));
#17283=CARTESIAN_POINT('',(52.7,-5.20417042793042E-15,-4.99999999999999));
#17284=CARTESIAN_POINT('Origin',(52.7,11.,5.20417042793042E-15));
#17285=CARTESIAN_POINT('',(30.,11.,6.93889390390723E-15));
#17286=CARTESIAN_POINT('',(52.7,11.,5.20417042793042E-15));
#17287=CARTESIAN_POINT('Origin',(52.7,-8.67361737988404E-15,6.93889390390723E-15));
#17288=CARTESIAN_POINT('Origin',(30.,-6.93889390390723E-15,6.93889390390723E-15));
#17289=CARTESIAN_POINT('Origin',(78.,-8.67361737988404E-15,6.93889390390723E-15));
#17290=CARTESIAN_POINT('Origin',(88.,-6.93889390390723E-15,3.46944695195361E-15));
#17291=CARTESIAN_POINT('',(88.,5.49999999999999,1.625));
#17292=CARTESIAN_POINT('',(88.,-5.20417042793042E-15,1.625));
#17293=CARTESIAN_POINT('',(88.,5.5,-1.62499999999999));
#17294=CARTESIAN_POINT('',(88.,5.5,0.));
#17295=CARTESIAN_POINT('',(88.,-6.93889390390723E-15,-1.62499999999999));
#17296=CARTESIAN_POINT('Origin',(88.,-5.20417042793042E-15,1.625));
#17297=CARTESIAN_POINT('',(88.,5.49999999999999,1.625));
#17298=CARTESIAN_POINT('Origin',(88.,-6.93889390390723E-15,-1.62499999999999));
#17299=CARTESIAN_POINT('',(88.,5.5,-1.62499999999999));
#17300=CARTESIAN_POINT('Origin',(88.,5.5,0.));
#17301=CARTESIAN_POINT('',(0.,0.,0.));
#17302=CARTESIAN_POINT('Origin',(0.,0.,-6.93889390390723E-15));
#17303=CARTESIAN_POINT('',(-3.54343684303821,-43.3554385900939,6.16441400296896));
#17304=CARTESIAN_POINT('',(-3.84642767658917,-41.3213624427943,0.));
#17305=CARTESIAN_POINT('Ctrl Pts',(-3.54343684303822,-43.3554385900939,
6.16441400296899));
#17306=CARTESIAN_POINT('Ctrl Pts',(-3.55141066631791,-42.7078411106921,
5.27531660683076));
#17307=CARTESIAN_POINT('Ctrl Pts',(-3.57572362730238,-42.2030493088126,
4.29109868658263));
#17308=CARTESIAN_POINT('Ctrl Pts',(-3.6760022876941,-41.5111240838458,2.19783870908455));
#17309=CARTESIAN_POINT('Ctrl Pts',(-3.75038336645554,-41.3303027940034,
1.10199792653041));
#17310=CARTESIAN_POINT('Ctrl Pts',(-3.84642767658919,-41.3213624427943,
1.38777878078145E-15));
#17311=CARTESIAN_POINT('',(-3.54327233497679,-43.3554520350116,-6.16441400296897));
#17312=CARTESIAN_POINT('Ctrl Pts',(-3.54327233497681,-43.3554520350116,
-6.16441400296899));
#17313=CARTESIAN_POINT('Ctrl Pts',(-3.55068393228085,-42.7074736895779,
-5.27472971793057));
#17314=CARTESIAN_POINT('Ctrl Pts',(-3.57665600754489,-42.2023811348684,
-4.28982003626222));
#17315=CARTESIAN_POINT('Ctrl Pts',(-3.67659250957593,-41.5108986473516,
-2.19678068827402));
#17316=CARTESIAN_POINT('Ctrl Pts',(-3.74909596947971,-41.3304226322436,
-1.10143125928569));
#17317=CARTESIAN_POINT('Ctrl Pts',(-3.84642767658919,-41.3213624427943,
-1.38777878078145E-15));
#17318=CARTESIAN_POINT('',(-1.48664137583835,-43.4745891000668,-6.16441400296897));
#17319=CARTESIAN_POINT('Origin',(-5.20417042793042E-15,1.73472347597681E-15,
-6.16441400296897));
#17320=CARTESIAN_POINT('',(-2.07336642434586,-41.448174286335,0.));
#17321=CARTESIAN_POINT('Ctrl Pts',(-2.07336642434585,-41.4481742863349,
9.0205620750794E-16));
#17322=CARTESIAN_POINT('Ctrl Pts',(-2.06122214993793,-41.4487817806634,
-0.137010845842713));
#17323=CARTESIAN_POINT('Ctrl Pts',(-2.04906663309419,-41.4520669390525,
-0.273849719833661));
#17324=CARTESIAN_POINT('Ctrl Pts',(-2.02470703660086,-41.4639867448445,
-0.547496131359158));
#17325=CARTESIAN_POINT('Ctrl Pts',(-2.01251001184278,-41.4726232572572,
-0.684223919449433));
#17326=CARTESIAN_POINT('Ctrl Pts',(-1.97587807515071,-41.5065536416689,
-1.09397285879738));
#17327=CARTESIAN_POINT('Ctrl Pts',(-1.95143443912056,-41.5398552486479,
-1.36621764182242));
#17328=CARTESIAN_POINT('Ctrl Pts',(-1.87808530350882,-41.6716267136228,
-2.17875768609682));
#17329=CARTESIAN_POINT('Ctrl Pts',(-1.82935412691929,-41.8017662331319,
-2.71300426676783));
#17330=CARTESIAN_POINT('Ctrl Pts',(-1.73185220830973,-42.144880341048,-3.75889728641896));
#17331=CARTESIAN_POINT('Ctrl Pts',(-1.68324609183627,-42.3577123750293,
-4.26878718252178));
#17332=CARTESIAN_POINT('Ctrl Pts',(-1.58505547146646,-42.8607776274967,
-5.24984087225669));
#17333=CARTESIAN_POINT('Ctrl Pts',(-1.53586728286777,-43.1500457179623,
-5.71948809643066));
#17334=CARTESIAN_POINT('Ctrl Pts',(-1.48664137583835,-43.4745891000668,
-6.16441400296899));
#17335=CARTESIAN_POINT('',(-1.48703027021499,-43.4745757998335,6.16441400296896));
#17336=CARTESIAN_POINT('Ctrl Pts',(-2.07336642434584,-41.4481742863349,
-2.77555756156289E-16));
#17337=CARTESIAN_POINT('Ctrl Pts',(-1.97732270203172,-41.4529786916566,
1.09861960926666));
#17338=CARTESIAN_POINT('Ctrl Pts',(-1.87861834962005,-41.630211988073,2.18971594132761));
#17339=CARTESIAN_POINT('Ctrl Pts',(-1.68194342719021,-42.3167003895122,
4.28292314717353));
#17340=CARTESIAN_POINT('Ctrl Pts',(-1.58640053900951,-42.8234325995621,
5.27177304443354));
#17341=CARTESIAN_POINT('Ctrl Pts',(-1.48703027021497,-43.4745757998335,
6.16441400296898));
#17342=CARTESIAN_POINT('Origin',(-1.73472347597681E-15,-1.73472347597681E-15,
6.16441400296896));
#17343=CARTESIAN_POINT('Origin',(0.,0.,-6.93889390390723E-15));
#17344=CARTESIAN_POINT('',(-9.67749199640668,-42.4098590973784,6.16441400296896));
#17345=CARTESIAN_POINT('',(-9.68791960221031,-40.3533668208876,0.));
#17346=CARTESIAN_POINT('Ctrl Pts',(-9.67749199640668,-42.4098590973784,
6.164414002969));
#17347=CARTESIAN_POINT('Ctrl Pts',(-9.59322192711545,-41.767718433188,5.27531660683078));
#17348=CARTESIAN_POINT('Ctrl Pts',(-9.54544805356732,-41.2646045888915,
4.29109868658267));
#17349=CARTESIAN_POINT('Ctrl Pts',(-9.54623479529778,-40.5654510237051,
2.19783870908455));
#17350=CARTESIAN_POINT('Ctrl Pts',(-9.59412522930581,-40.375884702676,1.1019979265304));
#17351=CARTESIAN_POINT('Ctrl Pts',(-9.68791960221032,-40.3533668208876,
1.11022302462516E-15));
#17352=CARTESIAN_POINT('',(-9.67733107621878,-42.4098958173827,-6.16441400296897));
#17353=CARTESIAN_POINT('Ctrl Pts',(-9.67733107621879,-42.4098958173827,
-6.164414002969));
#17354=CARTESIAN_POINT('Ctrl Pts',(-9.59245030071221,-41.7674581769263,
-5.2747297179302));
#17355=CARTESIAN_POINT('Ctrl Pts',(-9.5462758524577,-41.2638105244509,-4.28982003626219));
#17356=CARTESIAN_POINT('Ctrl Pts',(-9.54678692660889,-40.5651438845136,
-2.19678068831833));
#17357=CARTESIAN_POINT('Ctrl Pts',(-9.59286799090522,-40.3761865368352,
-1.10143125952358));
#17358=CARTESIAN_POINT('Ctrl Pts',(-9.68791960221033,-40.3533668208876,
-2.22044604925031E-15));
#17359=CARTESIAN_POINT('',(-7.65858862696402,-42.8205093412368,-6.16441400296901));
#17360=CARTESIAN_POINT('Origin',(-5.20417042793042E-15,1.73472347597681E-15,
-6.16441400296897));
#17361=CARTESIAN_POINT('',(-7.95095276397625,-40.7312208280702,0.));
#17362=CARTESIAN_POINT('Ctrl Pts',(-7.95095276397622,-40.7312208280702,
2.46330733588707E-15));
#17363=CARTESIAN_POINT('Ctrl Pts',(-7.93901575180353,-40.7335509968694,
-0.137043042087696));
#17364=CARTESIAN_POINT('Ctrl Pts',(-7.92744885398147,-40.7385344220979,
-0.273914065095848));
#17365=CARTESIAN_POINT('Ctrl Pts',(-7.90502864323289,-40.7538057116238,
-0.547624684008695));
#17366=CARTESIAN_POINT('Ctrl Pts',(-7.8941825814094,-40.7640944186137,-0.684384502473543));
#17367=CARTESIAN_POINT('Ctrl Pts',(-7.86274596139053,-40.8029092867107,
-1.09422919239435));
#17368=CARTESIAN_POINT('Ctrl Pts',(-7.8432869311216,-40.8393666280175,-1.36653715783867));
#17369=CARTESIAN_POINT('Ctrl Pts',(-7.78942904928734,-40.9802981987834,
-2.17926357855915));
#17370=CARTESIAN_POINT('Ctrl Pts',(-7.75971205509762,-41.1161093962788,
-2.71362913030393));
#17371=CARTESIAN_POINT('Ctrl Pts',(-7.7120439733908,-41.4696829616657,-3.75949691623912));
#17372=CARTESIAN_POINT('Ctrl Pts',(-7.69422964590224,-41.6872426581296,
-4.26925519586819));
#17373=CARTESIAN_POINT('Ctrl Pts',(-7.66864299491693,-42.1990770319903,
-5.25006061967085));
#17374=CARTESIAN_POINT('Ctrl Pts',(-7.66112555224713,-42.4923406106851,
-5.71959225708845));
#17375=CARTESIAN_POINT('Ctrl Pts',(-7.658588626964,-42.8205093412367,-6.16441400296904));
#17376=CARTESIAN_POINT('',(-7.65897167013779,-42.82044083094,6.16441400296896));
#17377=CARTESIAN_POINT('Ctrl Pts',(-7.95095276397622,-40.7312208280702,
-1.38777878078145E-15));
#17378=CARTESIAN_POINT('Ctrl Pts',(-7.85657036643801,-40.7496447782814,
1.09861960926659));
#17379=CARTESIAN_POINT('Ctrl Pts',(-7.7840936099301,-40.9391211892399,2.18971594132748));
#17380=CARTESIAN_POINT('Ctrl Pts',(-7.68711804045607,-41.646611888365,4.28292314717352));
#17381=CARTESIAN_POINT('Ctrl Pts',(-7.66466315363669,-42.1617834658437,
5.27177304443355));
#17382=CARTESIAN_POINT('Ctrl Pts',(-7.65897167013776,-42.8204408309399,
6.16441400296899));
#17383=CARTESIAN_POINT('Origin',(-1.73472347597681E-15,-1.73472347597681E-15,
6.16441400296896));
#17384=CARTESIAN_POINT('Origin',(0.,0.,-6.93889390390723E-15));
#17385=CARTESIAN_POINT('',(-15.6145413203107,-40.6009371733746,6.16441400296896));
#17386=CARTESIAN_POINT('',(-15.3321934223835,-38.563893020008,0.));
#17387=CARTESIAN_POINT('Ctrl Pts',(-15.6145413203107,-40.6009371733746,
6.16441400296898));
#17388=CARTESIAN_POINT('Ctrl Pts',(-15.4397428540445,-39.9773254565378,
5.27531660683075));
#17389=CARTESIAN_POINT('Ctrl Pts',(-15.3208546842607,-39.4861315168337,
4.29109868658265));
#17390=CARTESIAN_POINT('Ctrl Pts',(-15.2221334915371,-38.7939823618226,
2.19783870908461));
#17391=CARTESIAN_POINT('Ctrl Pts',(-15.2425583696598,-38.5995300332388,
1.10199792653054));
#17392=CARTESIAN_POINT('Ctrl Pts',(-15.3321934223835,-38.563893020008,2.4980018054066E-15));
#17393=CARTESIAN_POINT('',(-15.6143872638446,-40.6009964209586,-6.16441400296898));
#17394=CARTESIAN_POINT('Ctrl Pts',(-15.6143872638446,-40.6009964209586,
-6.164414002969));
#17395=CARTESIAN_POINT('Ctrl Pts',(-15.4389420434457,-39.9771776635648,
-5.27472971844796));
#17396=CARTESIAN_POINT('Ctrl Pts',(-15.3215610503336,-39.4852277273297,
-4.28982003740452));
#17397=CARTESIAN_POINT('Ctrl Pts',(-15.2474291081464,-38.9669376181131,
-2.72134440716479));
#17398=CARTESIAN_POINT('Ctrl Pts',(-15.2397722663402,-38.8316218835454,
-2.18467279509807));
#17399=CARTESIAN_POINT('Ctrl Pts',(-15.254622909041,-38.6871163772095,-1.36905841490953));
#17400=CARTESIAN_POINT('Ctrl Pts',(-15.2639410255199,-38.6487537976598,
-1.09600303225455));
#17401=CARTESIAN_POINT('Ctrl Pts',(-15.2845639945731,-38.6059048579417,
-0.685230045232502));
#17402=CARTESIAN_POINT('Ctrl Pts',(-15.2925374872687,-38.5940776984981,
-0.548230322286331));
#17403=CARTESIAN_POINT('Ctrl Pts',(-15.3107058126117,-38.5753161429334,
-0.274077591982354));
#17404=CARTESIAN_POINT('Ctrl Pts',(-15.3208934838215,-38.5683856381055,
-0.137016510472968));
#17405=CARTESIAN_POINT('Ctrl Pts',(-15.3321934223835,-38.563893020008,-1.2490009027033E-15));
#17406=CARTESIAN_POINT('',(-13.6746290992012,-41.2947274963679,-6.16441400296901));
#17407=CARTESIAN_POINT('Origin',(-5.20417042793042E-15,1.73472347597681E-15,
-6.16441400296897));
#17408=CARTESIAN_POINT('',(-13.6666806339864,-39.1850971728874,0.));
#17409=CARTESIAN_POINT('Ctrl Pts',(-13.6666806339864,-39.1850971728873,
1.70002900645727E-15));
#17410=CARTESIAN_POINT('Ctrl Pts',(-13.6551967409802,-39.1891024378853,
-0.137043042092346));
#17411=CARTESIAN_POINT('Ctrl Pts',(-13.6444567928547,-39.1956812802236,
-0.273914065098134));
#17412=CARTESIAN_POINT('Ctrl Pts',(-13.6244381186219,-39.2139878587089,
-0.547624684011075));
#17413=CARTESIAN_POINT('Ctrl Pts',(-13.6151666897398,-39.2257153970312,
-0.684384502476133));
#17414=CARTESIAN_POINT('Ctrl Pts',(-13.5895739808594,-39.268609083232,-1.09422919239856));
#17415=CARTESIAN_POINT('Ctrl Pts',(-13.5755014360926,-39.3074646501175,
-1.36653715784331));
#17416=CARTESIAN_POINT('Ctrl Pts',(-13.5422484035402,-39.4546265164425,
-2.17926357856199));
#17417=CARTESIAN_POINT('Ctrl Pts',(-13.5321618341116,-39.5932845209921,
-2.71362913030486));
#17418=CARTESIAN_POINT('Ctrl Pts',(-13.5352977095238,-39.9500430926316,
-3.75949691623844));
#17419=CARTESIAN_POINT('Ctrl Pts',(-13.5486266792216,-40.1679235882157,
-4.26925519586768));
#17420=CARTESIAN_POINT('Ctrl Pts',(-13.5961420895942,-40.6781895862498,
-5.25006061967041));
#17421=CARTESIAN_POINT('Ctrl Pts',(-13.6304369224277,-40.9695380082016,
-5.71959225708826));
#17422=CARTESIAN_POINT('Ctrl Pts',(-13.6746290992012,-41.2947274963679,
-6.16441400296904));
#17423=CARTESIAN_POINT('',(-13.674998493507,-41.2946051706828,6.16441400296896));
#17424=CARTESIAN_POINT('Ctrl Pts',(-13.6666806339864,-39.1850971728873,
-2.22044604925031E-15));
#17425=CARTESIAN_POINT('Ctrl Pts',(-13.5758809146616,-39.216765609492,1.09861960926666));
#17426=CARTESIAN_POINT('Ctrl Pts',(-13.5311071718143,-39.4146279416704,
2.1897159413276));
#17427=CARTESIAN_POINT('Ctrl Pts',(-13.5358050982361,-40.1287184680819,
4.28292314717352));
#17428=CARTESIAN_POINT('Ctrl Pts',(-13.5868953295191,-40.641842005304,5.2717730444335));
#17429=CARTESIAN_POINT('Ctrl Pts',(-13.674998493507,-41.2946051706828,6.16441400296898));
#17430=CARTESIAN_POINT('Origin',(-1.73472347597681E-15,-1.73472347597681E-15,
6.16441400296896));
#17431=CARTESIAN_POINT('Origin',(0.,0.,-6.93889390390723E-15));
#17432=CARTESIAN_POINT('',(-21.2337236115519,-37.9654972519553,6.16441400296896));
#17433=CARTESIAN_POINT('',(-20.6643479988718,-35.9893695663251,0.));
#17434=CARTESIAN_POINT('Ctrl Pts',(-21.2337236115519,-37.9654972519553,
6.16441400296898));
#17435=CARTESIAN_POINT('Ctrl Pts',(-20.9719551410068,-37.3731094186791,
5.27531660683075));
#17436=CARTESIAN_POINT('Ctrl Pts',(-20.784372895279,-36.9038346756933,4.29109868658264));
#17437=CARTESIAN_POINT('Ctrl Pts',(-20.5881534468967,-36.2327800916602,
2.19783870908455));
#17438=CARTESIAN_POINT('Ctrl Pts',(-20.5806969775162,-36.0374002441775,
1.10199792653042));
#17439=CARTESIAN_POINT('Ctrl Pts',(-20.6643479988717,-35.9893695663251,
2.22044604925031E-15));
#17440=CARTESIAN_POINT('',(-21.2335795549793,-37.9655778209995,-6.16441400296897));
#17441=CARTESIAN_POINT('Ctrl Pts',(-21.2335795549793,-37.9655778209995,
-6.16441400296899));
#17442=CARTESIAN_POINT('Ctrl Pts',(-20.9711414482259,-37.373077096907,-5.27472971792917));
#17443=CARTESIAN_POINT('Ctrl Pts',(-20.7849434486971,-36.9028395585411,
-4.28982003626091));
#17444=CARTESIAN_POINT('Ctrl Pts',(-20.5885966819103,-36.2323298404348,
-2.19678068843132));
#17445=CARTESIAN_POINT('Ctrl Pts',(-20.5795757025526,-36.0380440569569,
-1.10143126012878));
#17446=CARTESIAN_POINT('Ctrl Pts',(-20.6643479988717,-35.9893695663251,
-5.55111512312578E-16));
#17447=CARTESIAN_POINT('',(-19.4122935573269,-38.9283040838433,-6.16441400296902));
#17448=CARTESIAN_POINT('Origin',(-5.20417042793042E-15,1.73472347597681E-15,
-6.16441400296897));
#17449=CARTESIAN_POINT('',(-19.1041942977411,-36.8412779397534,0.));
#17450=CARTESIAN_POINT('Ctrl Pts',(-19.1041942977411,-36.8412779397534,
1.66533453693773E-15));
#17451=CARTESIAN_POINT('Ctrl Pts',(-19.0175901854858,-36.8861868538853,
-1.09924021646038));
#17452=CARTESIAN_POINT('Ctrl Pts',(-19.0022157487917,-37.0882313865091,
-2.19104319734134));
#17453=CARTESIAN_POINT('Ctrl Pts',(-19.0830118167184,-37.6171355518865,
-3.75949691436112));
#17454=CARTESIAN_POINT('Ctrl Pts',(-19.1272127442119,-37.8309014280932,
-4.26925519440142));
#17455=CARTESIAN_POINT('Ctrl Pts',(-19.2468629392382,-38.3292115063353,
-5.25006061898198));
#17456=CARTESIAN_POINT('Ctrl Pts',(-19.322271903712,-38.6127137580402,-5.71959225676187));
#17457=CARTESIAN_POINT('Ctrl Pts',(-19.4122935573269,-38.9283040838433,
-6.16441400296904));
#17458=CARTESIAN_POINT('',(-19.4126417829876,-38.9281304329582,6.16441400296896));
#17459=CARTESIAN_POINT('Ctrl Pts',(-19.1041942977411,-36.8412779397534,
5.55111512312578E-16));
#17460=CARTESIAN_POINT('Ctrl Pts',(-19.0188256770704,-36.8855461847065,
1.09861960926669));
#17461=CARTESIAN_POINT('Ctrl Pts',(-19.0026664121712,-37.0877665316095,
2.18971594132765));
#17462=CARTESIAN_POINT('Ctrl Pts',(-19.1089421982546,-37.7939200614567,
4.28292314717352));
#17463=CARTESIAN_POINT('Ctrl Pts',(-19.2325374978632,-38.2945498429305,
5.27177304443354));
#17464=CARTESIAN_POINT('Ctrl Pts',(-19.4126417829876,-38.9281304329582,
6.16441400296899));
#17465=CARTESIAN_POINT('Origin',(-1.73472347597681E-15,-1.73472347597681E-15,
6.16441400296896));
#17466=CARTESIAN_POINT('Origin',(0.,0.,-6.93889390390723E-15));
#17467=CARTESIAN_POINT('',(-26.4206485230644,-34.5571892899393,6.16441400296896));
#17468=CARTESIAN_POINT('',(-25.5758360411617,-32.6822063330434,0.));
#17469=CARTESIAN_POINT('Ctrl Pts',(-26.4206485230644,-34.5571892899393,
6.16441400296898));
#17470=CARTESIAN_POINT('Ctrl Pts',(-26.0772388994227,-34.0080846482038,
5.27531660683074));
#17471=CARTESIAN_POINT('Ctrl Pts',(-25.8247812113314,-33.5702821824271,
4.29109868658261));
#17472=CARTESIAN_POINT('Ctrl Pts',(-25.5350579694094,-32.9339829055412,
2.19783870908459));
#17473=CARTESIAN_POINT('Ctrl Pts',(-25.4998719447394,-32.7416529094253,
1.1019979265305));
#17474=CARTESIAN_POINT('Ctrl Pts',(-25.5758360411617,-32.6822063330433,
8.32667268468867E-16));
#17475=CARTESIAN_POINT('',(-26.4205173989538,-34.5572895402921,-6.16441400296898));
#17476=CARTESIAN_POINT('Ctrl Pts',(-26.4205173989538,-34.5572895402921,
-6.16441400296899));
#17477=CARTESIAN_POINT('Ctrl Pts',(-26.0764288890034,-34.0081684559713,
-5.27472971793099));
#17478=CARTESIAN_POINT('Ctrl Pts',(-25.825204337397,-33.5692159959191,-4.2898200362617));
#17479=CARTESIAN_POINT('Ctrl Pts',(-25.5354326154955,-32.9334741583167,
-2.1967806884535));
#17480=CARTESIAN_POINT('Ctrl Pts',(-25.498853706854,-32.7424497431807,-1.10143126024324));
#17481=CARTESIAN_POINT('Ctrl Pts',(-25.5758360411617,-32.6822063330433,
-1.94289029309402E-15));
#17482=CARTESIAN_POINT('',(-24.7547796990836,-35.7694126601185,-6.16441400296902));
#17483=CARTESIAN_POINT('Origin',(-5.20417042793042E-15,1.73472347597681E-15,
-6.16441400296897));
#17484=CARTESIAN_POINT('',(-24.1528016575408,-33.7474765292385,0.));
#17485=CARTESIAN_POINT('Ctrl Pts',(-24.1528016575407,-33.7474765292384,
7.63278329429795E-16));
#17486=CARTESIAN_POINT('Ctrl Pts',(-24.1429113564378,-33.7545549394024,
-0.137043042102339));
#17487=CARTESIAN_POINT('Ctrl Pts',(-24.1344599257467,-33.7638930854468,
-0.273914065100194));
#17488=CARTESIAN_POINT('Ctrl Pts',(-24.1204097076412,-33.7870980311517,
-0.547624684011823));
#17489=CARTESIAN_POINT('Ctrl Pts',(-24.1148178661299,-33.8009625851348,
-0.684384502477576));
#17490=CARTESIAN_POINT('Ctrl Pts',(-24.1023463896684,-33.8493290749669,
-1.09422919240133));
#17491=CARTESIAN_POINT('Ctrl Pts',(-24.0997907600507,-33.8905754123975,
-1.36653715784733));
#17492=CARTESIAN_POINT('Ctrl Pts',(-24.1093449978383,-34.0411446510019,
-2.17926357856575));
#17493=CARTESIAN_POINT('Ctrl Pts',(-24.1387314794962,-34.1770277470944,
-2.71362913030714));
#17494=CARTESIAN_POINT('Ctrl Pts',(-24.2422508344842,-34.5184516116601,
-3.75949691623867));
#17495=CARTESIAN_POINT('Ctrl Pts',(-24.3164239163555,-34.7237512115516,
-4.26925519586687));
#17496=CARTESIAN_POINT('Ctrl Pts',(-24.5057731630367,-35.199961213288,-5.25006061966791));
#17497=CARTESIAN_POINT('Ctrl Pts',(-24.6207611500201,-35.4698460060844,
-5.71959225708702));
#17498=CARTESIAN_POINT('Ctrl Pts',(-24.7547796990836,-35.7694126601185,
-6.16441400296905));
#17499=CARTESIAN_POINT('',(-24.7550996672026,-35.7691912190766,6.16441400296896));
#17500=CARTESIAN_POINT('Ctrl Pts',(-24.1528016575407,-33.7474765292384,
0.));
#17501=CARTESIAN_POINT('Ctrl Pts',(-24.0746019944582,-33.8034434087318,
1.09861960926657));
#17502=CARTESIAN_POINT('Ctrl Pts',(-24.087386163541,-34.0059051472517,2.18971594132744));
#17503=CARTESIAN_POINT('Ctrl Pts',(-24.2930763407555,-34.6897464310456,
4.28292314717365));
#17504=CARTESIAN_POINT('Ctrl Pts',(-24.486660664809,-35.1676910781175,5.2717730444337));
#17505=CARTESIAN_POINT('Ctrl Pts',(-24.7550996672026,-35.7691912190766,
6.16441400296898));
#17506=CARTESIAN_POINT('Origin',(-1.73472347597681E-15,-1.73472347597681E-15,
6.16441400296896));
#17507=CARTESIAN_POINT('Origin',(0.,0.,-6.93889390390723E-15));
#17508=CARTESIAN_POINT('',(-31.069725221506,-30.4453966086848,6.16441400296896));
#17509=CARTESIAN_POINT('',(-29.9666738162742,-28.7097276265211,0.));
#17510=CARTESIAN_POINT('Ctrl Pts',(-31.069725221506,-30.4453966086848,6.164414002969));
#17511=CARTESIAN_POINT('Ctrl Pts',(-30.6516652743934,-29.9507533455087,
5.27531660683074));
#17512=CARTESIAN_POINT('Ctrl Pts',(-30.3394714544404,-29.5533355526261,
4.29109868658259));
#17513=CARTESIAN_POINT('Ctrl Pts',(-29.9621423486912,-28.9647448012293,
2.19783870908461));
#17514=CARTESIAN_POINT('Ctrl Pts',(-29.899943054726,-28.7793799405673,1.10199792653053));
#17515=CARTESIAN_POINT('Ctrl Pts',(-29.9666738162742,-28.7097276265211,
1.11022302462516E-15));
#17516=CARTESIAN_POINT('',(-31.069609699158,-30.4455144995448,-6.16441400296898));
#17517=CARTESIAN_POINT('Ctrl Pts',(-31.0696096991579,-30.4455144995448,
-6.164414002969));
#17518=CARTESIAN_POINT('Ctrl Pts',(-30.6508754357951,-29.9509515767416,
-5.27472971793068));
#17519=CARTESIAN_POINT('Ctrl Pts',(-30.3397385395325,-29.5522200012418,
-4.28982003626194));
#17520=CARTESIAN_POINT('Ctrl Pts',(-29.9624407791487,-28.9641879146137,
-2.19678068845436));
#17521=CARTESIAN_POINT('Ctrl Pts',(-29.8990485823063,-28.7803135740586,
-1.10143126024342));
#17522=CARTESIAN_POINT('Ctrl Pts',(-29.9666738162742,-28.7097276265211,
-1.38777878078145E-15));
#17523=CARTESIAN_POINT('',(-29.5933299130507,-31.8823591451032,-6.16441400296901));
#17524=CARTESIAN_POINT('Origin',(-5.20417042793042E-15,1.73472347597681E-15,
-6.16441400296897));
#17525=CARTESIAN_POINT('',(-28.7097276265213,-29.9666738162741,0.));
#17526=CARTESIAN_POINT('Ctrl Pts',(-28.7097276265212,-29.9666738162741,
3.81639164714898E-16));
#17527=CARTESIAN_POINT('Ctrl Pts',(-28.7009453572214,-29.97508771503,-0.137043042104982));
#17528=CARTESIAN_POINT('Ctrl Pts',(-28.6939089066536,-29.9855335762034,
-0.273914065099642));
#17529=CARTESIAN_POINT('Ctrl Pts',(-28.6833041076052,-30.0105018835366,
-0.547624684008771));
#17530=CARTESIAN_POINT('Ctrl Pts',(-28.6797423147354,-30.0250211183715,
-0.684384502473487));
#17531=CARTESIAN_POINT('Ctrl Pts',(-28.674281049099,-30.0746701832321,-1.09422919239485));
#17532=CARTESIAN_POINT('Ctrl Pts',(-28.677621397945,-30.1158603964369,-1.36653715783935));
#17533=CARTESIAN_POINT('Ctrl Pts',(-28.7085066242031,-30.2635373474942,
-2.17926357855851));
#17534=CARTESIAN_POINT('Ctrl Pts',(-28.7569321746901,-30.3938552172152,
-2.71362913030275));
#17535=CARTESIAN_POINT('Ctrl Pts',(-28.9079875339794,-30.7170715388663,
-3.75949691623764));
#17536=CARTESIAN_POINT('Ctrl Pts',(-29.0106228201944,-30.9097255546857,
-4.26925519586596));
#17537=CARTESIAN_POINT('Ctrl Pts',(-29.2658165139508,-31.3541412178217,
-5.25006061967079));
#17538=CARTESIAN_POINT('Ctrl Pts',(-29.418042699661,-31.6049144758011,-5.71959225708859));
#17539=CARTESIAN_POINT('Ctrl Pts',(-29.5933299130507,-31.8823591451032,
-6.16441400296904));
#17540=CARTESIAN_POINT('',(-29.5936151100058,-31.8820944218042,6.16441400296897));
#17541=CARTESIAN_POINT('Ctrl Pts',(-28.7097276265212,-29.966673816274,0.));
#17542=CARTESIAN_POINT('Ctrl Pts',(-28.640288840658,-30.0332000060364,1.09861960926665));
#17543=CARTESIAN_POINT('Ctrl Pts',(-28.6817561949068,-30.2317815990284,
2.18971594132759));
#17544=CARTESIAN_POINT('Ctrl Pts',(-28.9826735044057,-30.8793896002663,
4.28292314717353));
#17545=CARTESIAN_POINT('Ctrl Pts',(-29.2423060343175,-31.3249195382003,
5.27177304443354));
#17546=CARTESIAN_POINT('Ctrl Pts',(-29.5936151100058,-31.8820944218042,
6.16441400296899));
#17547=CARTESIAN_POINT('Origin',(-1.73472347597681E-15,-1.73472347597681E-15,
6.16441400296896));
#17548=CARTESIAN_POINT('Origin',(0.,0.,-6.93889390390723E-15));
#17549=CARTESIAN_POINT('',(-35.0863119121265,-25.7138234497512,6.16441400296896));
#17550=CARTESIAN_POINT('',(-33.7474765292386,-24.1528016575407,0.));
#17551=CARTESIAN_POINT('Ctrl Pts',(-35.0863119121264,-25.7138234497512,
6.164414002969));
#17552=CARTESIAN_POINT('Ctrl Pts',(-34.602112136481,-25.2837110755395,5.27531660683076));
#17553=CARTESIAN_POINT('Ctrl Pts',(-34.2365375505477,-24.9347682357558,
4.29109868658263));
#17554=CARTESIAN_POINT('Ctrl Pts',(-33.7792839134372,-24.4058680201909,
2.19783870908452));
#17555=CARTESIAN_POINT('Ctrl Pts',(-33.691337548434,-24.2312417889978,1.10199792653034));
#17556=CARTESIAN_POINT('Ctrl Pts',(-33.7474765292385,-24.1528016575406,
2.77555756156289E-16));
#17557=CARTESIAN_POINT('',(-35.0862143432467,-25.7139565811984,-6.16441400296897));
#17558=CARTESIAN_POINT('Ctrl Pts',(-35.0862143432467,-25.7139565811983,
-6.164414002969));
#17559=CARTESIAN_POINT('Ctrl Pts',(-34.6013585485437,-25.2840196948202,
-5.27472971793046));
#17560=CARTESIAN_POINT('Ctrl Pts',(-34.2366431575829,-24.9336260289062,
-4.28982003626259));
#17561=CARTESIAN_POINT('Ctrl Pts',(-33.7795000530746,-24.4052743307777,
-2.19678068842248));
#17562=CARTESIAN_POINT('Ctrl Pts',(-33.6905850503741,-24.2322932161148,
-1.10143126006778));
#17563=CARTESIAN_POINT('Ctrl Pts',(-33.7474765292385,-24.1528016575406,
-1.94289029309402E-15));
#17564=CARTESIAN_POINT('',(-33.8294452700949,-27.3462727390344,-6.16441400296902));
#17565=CARTESIAN_POINT('Origin',(-5.20417042793042E-15,1.73472347597681E-15,
-6.16441400296897));
#17566=CARTESIAN_POINT('',(-32.6822063330435,-25.5758360411616,1.04083408558608E-14));
#17567=CARTESIAN_POINT('Ctrl Pts',(-32.6822063330434,-25.5758360411615,
1.35308431126191E-14));
#17568=CARTESIAN_POINT('Ctrl Pts',(-32.6747108772234,-25.5854141457942,
-0.137043042106718));
#17569=CARTESIAN_POINT('Ctrl Pts',(-32.6692326486208,-25.5967550744865,
-0.273914065103458));
#17570=CARTESIAN_POINT('Ctrl Pts',(-32.6622891517574,-25.6229784607124,
-0.547624684015696));
#17571=CARTESIAN_POINT('Ctrl Pts',(-32.6608299153614,-25.6378568066473,
-0.684384502481298));
#17572=CARTESIAN_POINT('Ctrl Pts',(-32.6624900361727,-25.6877777347498,
-1.09422919240422));
#17573=CARTESIAN_POINT('Ctrl Pts',(-32.6716583636155,-25.7280733097688,
-1.36653715784883));
#17574=CARTESIAN_POINT('Ctrl Pts',(-32.7232458442116,-25.8698516964151,
-2.17926357856531));
#17575=CARTESIAN_POINT('Ctrl Pts',(-32.7897246589715,-25.9919514437395,
-2.71362913030676));
#17576=CARTESIAN_POINT('Ctrl Pts',(-32.9852409710453,-26.2903804702531,
-3.7594969162393));
#17577=CARTESIAN_POINT('Ctrl Pts',(-33.1142491031337,-26.4664670218237,
-4.26925519586842));
#17578=CARTESIAN_POINT('Ctrl Pts',(-33.4300922362676,-26.8700413250523,
-5.25006061967152));
#17579=CARTESIAN_POINT('Ctrl Pts',(-33.6164577345519,-27.0965980278499,
-5.71959225708876));
#17580=CARTESIAN_POINT('Ctrl Pts',(-33.8294452700949,-27.3462727390344,
-6.16441400296905));
#17581=CARTESIAN_POINT('',(-33.829689890108,-27.345970122472,6.16441400296896));
#17582=CARTESIAN_POINT('Ctrl Pts',(-32.6822063330434,-25.5758360411615,
9.99200722162641E-15));
#17583=CARTESIAN_POINT('Ctrl Pts',(-32.6229419978348,-25.651567259815,1.09861960926662));
#17584=CARTESIAN_POINT('Ctrl Pts',(-32.692248381499,-25.8422261587078,2.18971594132752));
#17585=CARTESIAN_POINT('Ctrl Pts',(-33.0822670146348,-26.4404174460317,
4.28292314717354));
#17586=CARTESIAN_POINT('Ctrl Pts',(-33.4026623808143,-26.8444629700938,
5.27177304443356));
#17587=CARTESIAN_POINT('Ctrl Pts',(-33.829689890108,-27.345970122472,6.164414002969));
#17588=CARTESIAN_POINT('Origin',(-1.73472347597681E-15,-1.73472347597681E-15,
6.16441400296896));
#17589=CARTESIAN_POINT('Origin',(0.,0.,-6.93889390390723E-15));
#17590=CARTESIAN_POINT('',(-38.3886424727843,-20.4587909979242,6.16441400296896));
#17591=CARTESIAN_POINT('',(-36.8412779397535,-19.104194297741,3.46944695195361E-15));
#17592=CARTESIAN_POINT('Ctrl Pts',(-38.3886424727843,-20.4587909979242,
6.16441400296899));
#17593=CARTESIAN_POINT('Ctrl Pts',(-37.8481597797212,-20.101965360274,5.27531660683071));
#17594=CARTESIAN_POINT('Ctrl Pts',(-37.4366464721472,-19.8086009435392,
4.29109868658253));
#17595=CARTESIAN_POINT('Ctrl Pts',(-36.9087766691165,-19.3501581469729,
2.19783870908465));
#17596=CARTESIAN_POINT('Ctrl Pts',(-36.7968735674502,-19.1898254317353,
1.10199792653061));
#17597=CARTESIAN_POINT('Ctrl Pts',(-36.8412779397534,-19.1041942977409,
3.05311331771918E-15));
#17598=CARTESIAN_POINT('',(-38.3885648435901,-20.4589366597944,-6.16441400296897));
#17599=CARTESIAN_POINT('Ctrl Pts',(-38.3885648435901,-20.4589366597944,
-6.16441400296899));
#17600=CARTESIAN_POINT('Ctrl Pts',(-37.8474577833227,-20.1023780850071,
-5.27472971793101));
#17601=CARTESIAN_POINT('Ctrl Pts',(-37.4365884512732,-19.807455333257,-4.28982003626108));
#17602=CARTESIAN_POINT('Ctrl Pts',(-36.9089061179334,-19.3495397405838,
-2.19678068837342));
#17603=CARTESIAN_POINT('Ctrl Pts',(-36.796278362415,-19.1909732484813,-1.10143125981476));
#17604=CARTESIAN_POINT('Ctrl Pts',(-36.8412779397534,-19.1041942977409,
2.4980018054066E-15));
#17605=CARTESIAN_POINT('',(-37.37689067751,-22.2534950801323,-6.16441400296901));
#17606=CARTESIAN_POINT('Origin',(-5.20417042793042E-15,1.73472347597681E-15,
-6.16441400296897));
#17607=CARTESIAN_POINT('',(-35.9893695663252,-20.6643479988716,0.));
#17608=CARTESIAN_POINT('Ctrl Pts',(-35.9893695663251,-20.6643479988716,
2.46330733588707E-15));
#17609=CARTESIAN_POINT('Ctrl Pts',(-35.9833135098508,-20.6748953267903,
-0.137043042103492));
#17610=CARTESIAN_POINT('Ctrl Pts',(-35.9795050241501,-20.6869004543967,
-0.273914065100136));
#17611=CARTESIAN_POINT('Ctrl Pts',(-35.9763641790442,-20.7138450869921,
-0.547624684010087));
#17612=CARTESIAN_POINT('Ctrl Pts',(-35.9770372049667,-20.7287796638086,
-0.684384502474728));
#17613=CARTESIAN_POINT('Ctrl Pts',(-35.9857849169524,-20.7779562090156,
-1.09422919239792));
#17614=CARTESIAN_POINT('Ctrl Pts',(-36.0005945822839,-20.8165368441443,
-1.36653715784288));
#17615=CARTESIAN_POINT('Ctrl Pts',(-36.071834144877,-20.9495304672835,-2.17926357856208));
#17616=CARTESIAN_POINT('Ctrl Pts',(-36.15501290695,-21.0609264934646,-2.71362913030558));
#17617=CARTESIAN_POINT('Ctrl Pts',(-36.3910100235187,-21.3284930704613,
-3.75949691623798));
#17618=CARTESIAN_POINT('Ctrl Pts',(-36.5437647679417,-21.4844275433842,
-4.26925519586578));
#17619=CARTESIAN_POINT('Ctrl Pts',(-36.9138276850818,-21.8389448777016,
-5.25006061966817));
#17620=CARTESIAN_POINT('Ctrl Pts',(-37.1305386318308,-22.0366729841827,
-5.71959225708717));
#17621=CARTESIAN_POINT('Ctrl Pts',(-37.3768906775099,-22.2534950801323,
-6.16441400296905));
#17622=CARTESIAN_POINT('',(-37.3770897408172,-22.253160730712,6.16441400296896));
#17623=CARTESIAN_POINT('Ctrl Pts',(-35.9893695663251,-20.6643479988716,
-1.11022302462516E-15));
#17624=CARTESIAN_POINT('Ctrl Pts',(-35.9414861327318,-20.7477425771951,
1.09861960926678));
#17625=CARTESIAN_POINT('Ctrl Pts',(-36.0372206677032,-20.9265975166223,
2.18971594132783));
#17626=CARTESIAN_POINT('Ctrl Pts',(-36.508400969826,-21.4631946404635,4.28292314717348));
#17627=CARTESIAN_POINT('Ctrl Pts',(-36.8830368465616,-21.8175305489547,
5.27177304443343));
#17628=CARTESIAN_POINT('Ctrl Pts',(-37.3770897408172,-22.253160730712,6.16441400296898));
#17629=CARTESIAN_POINT('Origin',(-1.73472347597681E-15,-1.73472347597681E-15,
6.16441400296896));
#17630=CARTESIAN_POINT('Origin',(0.,0.,-6.93889390390723E-15));
#17631=CARTESIAN_POINT('',(-40.9094909763995,-14.7872765596607,6.16441400296896));
#17632=CARTESIAN_POINT('',(-39.1850971728874,-13.6666806339863,0.));
#17633=CARTESIAN_POINT('Ctrl Pts',(-40.9094909763995,-14.7872765596607,
6.16441400296899));
#17634=CARTESIAN_POINT('Ctrl Pts',(-40.3237280349261,-14.5110015995545,
5.27531660683078));
#17635=CARTESIAN_POINT('Ctrl Pts',(-39.8746532299474,-14.2791876594002,
4.29109868658268));
#17636=CARTESIAN_POINT('Ctrl Pts',(-39.2869131679351,-13.9005348551307,
2.19783870908458));
#17637=CARTESIAN_POINT('Ctrl Pts',(-39.1533313540539,-13.7577595675694,
1.10199792653047));
#17638=CARTESIAN_POINT('Ctrl Pts',(-39.1850971728874,-13.6666806339863,
5.55111512312578E-16));
#17639=CARTESIAN_POINT('',(-40.9094348672063,-14.7874317866831,-6.16441400296897));
#17640=CARTESIAN_POINT('Ctrl Pts',(-40.9094348672063,-14.7874317866831,
-6.16441400296899));
#17641=CARTESIAN_POINT('Ctrl Pts',(-40.3230919206938,-14.5115100278443,
-5.27472971793063));
#17642=CARTESIAN_POINT('Ctrl Pts',(-39.8744327623002,-14.2780619670101,
-4.28982003626127));
#17643=CARTESIAN_POINT('Ctrl Pts',(-39.2869532907287,-13.8999043207298,
-2.19678068831752));
#17644=CARTESIAN_POINT('Ctrl Pts',(-39.1529055587102,-13.7589804076816,
-1.10143125951959));
#17645=CARTESIAN_POINT('Ctrl Pts',(-39.1850971728874,-13.6666806339863,
-1.38777878078145E-15));
#17646=CARTESIAN_POINT('',(-40.1634503767788,-16.7077004351894,-6.16441400296902));
#17647=CARTESIAN_POINT('Origin',(-5.20417042793042E-15,1.73472347597681E-15,
-6.16441400296897));
#17648=CARTESIAN_POINT('',(-38.5638930200081,-15.3321934223834,0.));
#17649=CARTESIAN_POINT('Ctrl Pts',(-38.563893020008,-15.3321934223834,8.67361737988404E-16));
#17650=CARTESIAN_POINT('Ctrl Pts',(-38.5593996467226,-15.3434952604117,
-0.137043042096665));
#17651=CARTESIAN_POINT('Ctrl Pts',(-38.5573384337076,-15.3559201971581,
-0.273914065096707));
#17652=CARTESIAN_POINT('Ctrl Pts',(-38.5580641789047,-15.3830375611115,
-0.547624684006058));
#17653=CARTESIAN_POINT('Ctrl Pts',(-38.5608557662775,-15.397724343896,-0.684384502470298));
#17654=CARTESIAN_POINT('Ctrl Pts',(-38.5765129912447,-15.4451554135661,
-1.09422919239245));
#17655=CARTESIAN_POINT('Ctrl Pts',(-38.5966625123853,-15.481235718332,-1.36653715783741));
#17656=CARTESIAN_POINT('Ctrl Pts',(-38.6861039249185,-15.6027372113193,
-2.17926357855849));
#17657=CARTESIAN_POINT('Ctrl Pts',(-38.7842893545795,-15.7011618144977,
-2.71362913030383));
#17658=CARTESIAN_POINT('Ctrl Pts',(-39.0559630549181,-15.9324190580551,
-3.75949691623976));
#17659=CARTESIAN_POINT('Ctrl Pts',(-39.2293547655943,-16.0650270761305,
-4.26925519586824));
#17660=CARTESIAN_POINT('Ctrl Pts',(-39.646104052922,-16.3632704909573,-5.25006061967103));
#17661=CARTESIAN_POINT('Ctrl Pts',(-39.8887488381972,-16.5281448270819,
-5.71959225708847));
#17662=CARTESIAN_POINT('Ctrl Pts',(-40.1634503767788,-16.7077004351894,
-6.16441400296903));
#17663=CARTESIAN_POINT('',(-40.1635998310294,-16.707341159291,6.16441400296896));
#17664=CARTESIAN_POINT('Ctrl Pts',(-38.563893020008,-15.3321934223834,-1.38777878078145E-15));
#17665=CARTESIAN_POINT('Ctrl Pts',(-38.5283652566534,-15.4215536872524,
1.09861960926663));
#17666=CARTESIAN_POINT('Ctrl Pts',(-38.6485790638755,-15.584963696422,2.18971594132755));
#17667=CARTESIAN_POINT('Ctrl Pts',(-39.191329162806,-16.0490430867576,4.28292314717361));
#17668=CARTESIAN_POINT('Ctrl Pts',(-39.6125790440083,-16.3464561224017,
5.27177304443367));
#17669=CARTESIAN_POINT('Ctrl Pts',(-40.1635998310294,-16.707341159291,6.16441400296898));
#17670=CARTESIAN_POINT('Origin',(-1.73472347597681E-15,-1.73472347597681E-15,
6.16441400296896));
#17671=CARTESIAN_POINT('Origin',(0.,0.,-6.93889390390723E-15));
#17672=CARTESIAN_POINT('',(-42.5975402169652,-8.81473581362673,6.16441400296896));
#17673=CARTESIAN_POINT('',(-40.7312208280702,-7.95095276397609,0.));
#17674=CARTESIAN_POINT('Ctrl Pts',(-42.5975458454602,-8.81473754185287,
6.16442208586936));
#17675=CARTESIAN_POINT('Ctrl Pts',(-41.9784270998641,-8.62463742076724,
5.27532468973115));
#17676=CARTESIAN_POINT('Ctrl Pts',(-41.5009270369901,-8.45909129229262,
4.29109868658267));
#17677=CARTESIAN_POINT('Ctrl Pts',(-40.8652814087566,-8.1679367594703,2.19783870908461));
#17678=CARTESIAN_POINT('Ctrl Pts',(-40.712740223173,-8.04562539271016,1.10199792653052));
#17679=CARTESIAN_POINT('Ctrl Pts',(-40.7312208280702,-7.95095276397607,
5.55111512312578E-16));
#17680=CARTESIAN_POINT('',(-42.5975067699919,-8.81489744582999,-6.16441400296896));
#17681=CARTESIAN_POINT('Ctrl Pts',(-42.5975067699918,-8.81489744582997,
-6.16441400296899));
#17682=CARTESIAN_POINT('Ctrl Pts',(-41.9778641887521,-8.62522947425753,
-5.27472971793024));
#17683=CARTESIAN_POINT('Ctrl Pts',(-41.5005486106554,-8.45800843364591,
-4.28982003626188));
#17684=CARTESIAN_POINT('Ctrl Pts',(-40.8652313887449,-8.16730693291995,
-2.19678068827478));
#17685=CARTESIAN_POINT('Ctrl Pts',(-40.7124925054799,-8.04689440340105,
-1.10143125929045));
#17686=CARTESIAN_POINT('Ctrl Pts',(-40.7312208280702,-7.95095276397607,
-1.38777878078145E-15));
#17687=CARTESIAN_POINT('',(-42.1323980482118,-10.8217851903945,-6.16441400296901));
#17688=CARTESIAN_POINT('Origin',(-5.20417042793042E-15,1.73472347597681E-15,
-6.16441400296897));
#17689=CARTESIAN_POINT('',(-40.3533668208877,-9.68791960221017,1.04083408558608E-14));
#17690=CARTESIAN_POINT('Ctrl Pts',(-40.3533668208876,-9.68791960221017,
1.2038980923279E-14));
#17691=CARTESIAN_POINT('Ctrl Pts',(-40.3505276029147,-9.69974587751488,
-0.137043042091313));
#17692=CARTESIAN_POINT('Ctrl Pts',(-40.3502556229396,-9.71233768751765,
-0.273914065097098));
#17693=CARTESIAN_POINT('Ctrl Pts',(-40.3548331843628,-9.73907575149574,
-0.547624684009998));
#17694=CARTESIAN_POINT('Ctrl Pts',(-40.3596865045181,-9.75321575970265,
-0.684384502475249));
#17695=CARTESIAN_POINT('Ctrl Pts',(-40.3819345065204,-9.79793579403437,
-1.09422919239669));
#17696=CARTESIAN_POINT('Ctrl Pts',(-40.4070136973265,-9.8307812774791,-1.36653715784155));
#17697=CARTESIAN_POINT('Ctrl Pts',(-40.5128361905684,-9.93831722029971,
-2.17926357856093));
#17698=CARTESIAN_POINT('Ctrl Pts',(-40.62402951561,-10.0217667593921,-2.7136291303046));
#17699=CARTESIAN_POINT('Ctrl Pts',(-40.9258493066162,-10.2120069389282,
-3.75949691623883));
#17700=CARTESIAN_POINT('Ctrl Pts',(-41.1163482283345,-10.3185889853199,
-4.26925519586717));
#17701=CARTESIAN_POINT('Ctrl Pts',(-41.5713000721685,-10.5544871047827,
-5.25006061967));
#17702=CARTESIAN_POINT('Ctrl Pts',(-41.8349391478766,-10.6831513045169,
-5.71959225708799));
#17703=CARTESIAN_POINT('Ctrl Pts',(-42.1323980482118,-10.8217851903945,
-6.16441400296903));
#17704=CARTESIAN_POINT('',(-42.1324948509394,-10.8214083018602,6.16441400296896));
#17705=CARTESIAN_POINT('Ctrl Pts',(-40.3533668208876,-9.68791960221018,
8.60422844084496E-15));
#17706=CARTESIAN_POINT('Ctrl Pts',(-40.33091797058,-9.78142643632573,1.09861960926666));
#17707=CARTESIAN_POINT('Ctrl Pts',(-40.4731638436058,-9.92606495868674,
2.18971594132761));
#17708=CARTESIAN_POINT('Ctrl Pts',(-41.0764349124918,-10.3081792974238,
4.2829231471735));
#17709=CARTESIAN_POINT('Ctrl Pts',(-41.5357233653636,-10.5426149884832,
5.27177304443348));
#17710=CARTESIAN_POINT('Ctrl Pts',(-42.1324948509394,-10.8214083018602,
6.16441400296899));
#17711=CARTESIAN_POINT('Origin',(-1.73472347597681E-15,-1.73472347597681E-15,
6.16441400296896));
#17712=CARTESIAN_POINT('Origin',(0.,0.,-6.93889390390723E-15));
#17713=CARTESIAN_POINT('',(-43.4184263798756,-2.66275246602631,6.16441400296896));
#17714=CARTESIAN_POINT('',(-41.448174286335,-2.0733664243457,0.));
#17715=CARTESIAN_POINT('Ctrl Pts',(-43.4184263798755,-2.66275246602631,
6.16441400296899));
#17716=CARTESIAN_POINT('Ctrl Pts',(-42.7785553024261,-2.56269707422304,
5.27531660683071));
#17717=CARTESIAN_POINT('Ctrl Pts',(-42.2823616483505,-2.46679222047884,
4.29109868658253));
#17718=CARTESIAN_POINT('Ctrl Pts',(-41.611750365836,-2.26906302577168,2.19783870908463));
#17719=CARTESIAN_POINT('Ctrl Pts',(-41.4433551071959,-2.16970548652307,
1.10199792653057));
#17720=CARTESIAN_POINT('Ctrl Pts',(-41.4481742863349,-2.07336642434569,
1.11022302462516E-15));
#17721=CARTESIAN_POINT('',(-43.4184162760053,-2.66291721304384,-6.16441400296897));
#17722=CARTESIAN_POINT('Ctrl Pts',(-43.4184220936431,-2.66291811752308,
-6.16442208610002));
#17723=CARTESIAN_POINT('Ctrl Pts',(-42.7780940137297,-2.56336502615921,
-5.27473780106136));
#17724=CARTESIAN_POINT('Ctrl Pts',(-42.2818329669972,-2.46577423945546,
-4.28982003626243));
#17725=CARTESIAN_POINT('Ctrl Pts',(-41.6116112212699,-2.26844672853033,
-2.19678068820493));
#17726=CARTESIAN_POINT('Ctrl Pts',(-41.4432905099648,-2.17099683438165,
-1.10143125891921));
#17727=CARTESIAN_POINT('Ctrl Pts',(-41.4481742863349,-2.07336642434569,
2.77555756156289E-16));
#17728=CARTESIAN_POINT('',(-43.2436515951817,-4.7155696065853,-6.16441400296901));
#17729=CARTESIAN_POINT('Origin',(-5.20417042793042E-15,1.73472347597681E-15,
-6.16441400296897));
#17730=CARTESIAN_POINT('',(-41.3213624427943,-3.84642767658903,0.));
#17731=CARTESIAN_POINT('Ctrl Pts',(-41.3213624427943,-3.84642767658904,
1.83880688453542E-15));
#17732=CARTESIAN_POINT('Ctrl Pts',(-41.320235178424,-3.85853764030828,-0.137043042087949));
#17733=CARTESIAN_POINT('Ctrl Pts',(-41.3217579682172,-3.87103999062632,
-0.27391406509514));
#17734=CARTESIAN_POINT('Ctrl Pts',(-41.3300941599161,-3.89685444475066,
-0.547624684006307));
#17735=CARTESIAN_POINT('Ctrl Pts',(-41.3369104132512,-3.91015982858841,
-0.684384502470434));
#17736=CARTESIAN_POINT('Ctrl Pts',(-41.3652962871257,-3.95125845664314,
-1.09422919239298));
#17737=CARTESIAN_POINT('Ctrl Pts',(-41.3947946075951,-3.98020047944156,
-1.36653715783799));
#17738=CARTESIAN_POINT('Ctrl Pts',(-41.5148439407502,-4.07158175040666,
-2.17926357855872));
#17739=CARTESIAN_POINT('Ctrl Pts',(-41.6367815857305,-4.13835743344657,
-2.71362913030384));
#17740=CARTESIAN_POINT('Ctrl Pts',(-41.9626032868359,-4.28370780751825,
-3.7594969162383));
#17741=CARTESIAN_POINT('Ctrl Pts',(-42.1663314109023,-4.36209417912445,
-4.26925519586628));
#17742=CARTESIAN_POINT('Ctrl Pts',(-42.6502243036723,-4.53084479779167,
-5.25006061966883));
#17743=CARTESIAN_POINT('Ctrl Pts',(-42.9294907385031,-4.62067962906769,
-5.71959225708739));
#17744=CARTESIAN_POINT('Ctrl Pts',(-43.2436515951816,-4.7155696065853,-6.16441400296904));
#17745=CARTESIAN_POINT('',(-43.2436937757663,-4.71518277776806,6.16441400296896));
#17746=CARTESIAN_POINT('Ctrl Pts',(-41.3213624427943,-3.84642767658904,
-8.32667268468867E-16));
#17747=CARTESIAN_POINT('Ctrl Pts',(-41.3124494993889,-3.94217755045996,
1.09861960926659));
#17748=CARTESIAN_POINT('Ctrl Pts',(-41.4738317224467,-4.06510016280015,
2.18971594132748));
#17749=CARTESIAN_POINT('Ctrl Pts',(-42.1253429020158,-4.3574707039288,4.28292314717357));
#17750=CARTESIAN_POINT('Ctrl Pts',(-42.6133201381353,-4.5241566157904,5.2717730444336));
#17751=CARTESIAN_POINT('Ctrl Pts',(-43.2436937757662,-4.71518277776806,
6.16441400296899));
#17752=CARTESIAN_POINT('Origin',(-1.73472347597681E-15,-1.73472347597681E-15,
6.16441400296896));
#17753=CARTESIAN_POINT('Origin',(0.,0.,-6.93889390390723E-15));
#17754=CARTESIAN_POINT('',(-43.3554385900939,3.54343684303835,6.16441400296897));
#17755=CARTESIAN_POINT('',(-41.3213624427943,3.84642767658933,0.));
#17756=CARTESIAN_POINT('Ctrl Pts',(-43.3554444774928,3.54343677054778,6.16442208586936));
#17757=CARTESIAN_POINT('Ctrl Pts',(-42.7078469980911,3.55141059382748,5.27532468973115));
#17758=CARTESIAN_POINT('Ctrl Pts',(-42.2030493088126,3.57572362730252,4.2910986865827));
#17759=CARTESIAN_POINT('Ctrl Pts',(-41.5111240838457,3.67600228769425,2.19783870908447));
#17760=CARTESIAN_POINT('Ctrl Pts',(-41.3303027940033,3.7503833664557,1.10199792653022));
#17761=CARTESIAN_POINT('Ctrl Pts',(-41.3213624427943,3.84642767658933,1.94289029309402E-15));
#17762=CARTESIAN_POINT('',(-43.3554520350115,3.54327233497867,-6.16441400296897));
#17763=CARTESIAN_POINT('Ctrl Pts',(-43.3554579221549,3.54327226764192,-6.16442208610002));
#17764=CARTESIAN_POINT('Ctrl Pts',(-42.707479577098,3.55068386494164,-5.27473780157895));
#17765=CARTESIAN_POINT('Ctrl Pts',(-42.2023811354534,3.57665600751496,-4.28982003740415));
#17766=CARTESIAN_POINT('Ctrl Pts',(-41.6842000357502,3.65154612751076,-2.72134440716138));
#17767=CARTESIAN_POINT('Ctrl Pts',(-41.5522083575935,3.68232228947575,-2.18467279509217));
#17768=CARTESIAN_POINT('Ctrl Pts',(-41.4177402491549,3.73728328257893,-1.36905841490162));
#17769=CARTESIAN_POINT('Ctrl Pts',(-41.3835568404079,3.75703193749213,-1.09600303224686));
#17770=CARTESIAN_POINT('Ctrl Pts',(-41.3482537456227,3.78889147274118,-0.685230045226319));
#17771=CARTESIAN_POINT('Ctrl Pts',(-41.3391520617229,3.79987407882911,-0.548230322281482));
#17772=CARTESIAN_POINT('Ctrl Pts',(-41.3262690897369,3.82259220036053,-0.274077591980457));
#17773=CARTESIAN_POINT('Ctrl Pts',(-41.322489517709,3.83431974815085,-0.137016510473668));
#17774=CARTESIAN_POINT('Ctrl Pts',(-41.3213624427943,3.84642767658934,-1.66533453693773E-15));
#17775=CARTESIAN_POINT('',(-43.4745891000669,1.48664137583784,-6.16441400296901));
#17776=CARTESIAN_POINT('Origin',(-5.20417042793042E-15,1.73472347597681E-15,
-6.16441400296897));
#17777=CARTESIAN_POINT('',(-41.4481742863349,2.07336642434601,0.));
#17778=CARTESIAN_POINT('Ctrl Pts',(-41.4481742863349,2.07336642434599,1.2490009027033E-15));
#17779=CARTESIAN_POINT('Ctrl Pts',(-41.4487819234188,2.06121929614942,-0.137043042079584));
#17780=CARTESIAN_POINT('Ctrl Pts',(-41.452068483371,2.04906091731251,-0.273914065091576));
#17781=CARTESIAN_POINT('Ctrl Pts',(-41.4639936045221,2.0246955808817,-0.547624684002258));
#17782=CARTESIAN_POINT('Ctrl Pts',(-41.4726340317754,2.01249568065706,-0.68438450246554));
#17783=CARTESIAN_POINT('Ctrl Pts',(-41.5065799229875,1.97585510842473,-1.09422919238728));
#17784=CARTESIAN_POINT('Ctrl Pts',(-41.5398968723813,1.95140572239379,-1.36653715783194));
#17785=CARTESIAN_POINT('Ctrl Pts',(-41.67172918722,1.87803938243819,-2.17926357855389));
#17786=CARTESIAN_POINT('Ctrl Pts',(-41.8019288533266,1.82929691579476,-2.71362913030093));
#17787=CARTESIAN_POINT('Ctrl Pts',(-42.1451196742907,1.73179526165578,-3.75949691623917));
#17788=CARTESIAN_POINT('Ctrl Pts',(-42.3579296836043,1.68320028532058,-4.2692551958683));
#17789=CARTESIAN_POINT('Ctrl Pts',(-42.8609129614465,1.58503244341179,-5.25006061967115));
#17790=CARTESIAN_POINT('Ctrl Pts',(-43.1501216961234,1.535855758695,-5.71959225708858));
#17791=CARTESIAN_POINT('Ctrl Pts',(-43.4745891000668,1.48664137583782,-6.16441400296904));
#17792=CARTESIAN_POINT('',(-43.4745757998335,1.48703027021514,6.16441400296896));
#17793=CARTESIAN_POINT('Ctrl Pts',(-41.4481742863349,2.07336642434599,-2.77555756156289E-16));
#17794=CARTESIAN_POINT('Ctrl Pts',(-41.4529786916566,1.97732270203186,1.09861960926673));
#17795=CARTESIAN_POINT('Ctrl Pts',(-41.6302119880731,1.87861834962018,2.18971594132774));
#17796=CARTESIAN_POINT('Ctrl Pts',(-42.3167003895122,1.68194342719036,4.28292314717356));
#17797=CARTESIAN_POINT('Ctrl Pts',(-42.8234325995621,1.58640053900966,5.27177304443357));
#17798=CARTESIAN_POINT('Ctrl Pts',(-43.4745757998335,1.48703027021513,6.16441400296899));
#17799=CARTESIAN_POINT('Origin',(-1.73472347597681E-15,-1.73472347597681E-15,
6.16441400296896));
#17800=CARTESIAN_POINT('Origin',(0.,0.,-6.93889390390723E-15));
#17801=CARTESIAN_POINT('',(-42.4098590973784,9.67749199640682,6.16441400296896));
#17802=CARTESIAN_POINT('',(-40.3533668208876,9.68791960221045,0.));
#17803=CARTESIAN_POINT('Ctrl Pts',(-42.4098649351686,9.67749276251832,6.16442208586937));
#17804=CARTESIAN_POINT('Ctrl Pts',(-41.7677242709781,9.59322269322707,5.27532468973104));
#17805=CARTESIAN_POINT('Ctrl Pts',(-41.2646045888914,9.54544805356745,4.29109868658242));
#17806=CARTESIAN_POINT('Ctrl Pts',(-40.5654510237052,9.54623479529791,2.19783870908471));
#17807=CARTESIAN_POINT('Ctrl Pts',(-40.375884702676,9.59412522930591,1.10199792653074));
#17808=CARTESIAN_POINT('Ctrl Pts',(-40.3533668208875,9.68791960221046,8.32667268468867E-16));
#17809=CARTESIAN_POINT('',(-42.4098958173841,9.67733107621259,-6.16441400296897));
#17810=CARTESIAN_POINT('Ctrl Pts',(-42.4098958173841,9.6773310762126,-6.164414002969));
#17811=CARTESIAN_POINT('Ctrl Pts',(-41.7674581769275,9.59245030070757,-5.27472971793047));
#17812=CARTESIAN_POINT('Ctrl Pts',(-41.263810524451,9.54627585245725,-4.28982003626203));
#17813=CARTESIAN_POINT('Ctrl Pts',(-40.5651438845123,9.54678692661234,-2.19678068831686));
#17814=CARTESIAN_POINT('Ctrl Pts',(-40.3761865368333,9.59286799091328,-1.1014312595142));
#17815=CARTESIAN_POINT('Ctrl Pts',(-40.3533668208875,9.68791960221045,-2.77555756156289E-16));
#17816=CARTESIAN_POINT('',(-42.8205093412364,7.65858862696565,-6.16441400296902));
#17817=CARTESIAN_POINT('Origin',(-5.20417042793042E-15,1.73472347597681E-15,
-6.16441400296897));
#17818=CARTESIAN_POINT('',(-40.7312208280702,7.95095276397637,0.));
#17819=CARTESIAN_POINT('Ctrl Pts',(-40.7312208280702,7.95095276397635,1.66533453693773E-15));
#17820=CARTESIAN_POINT('Ctrl Pts',(-40.7499114176564,7.85520442356475,-1.0992402164504));
#17821=CARTESIAN_POINT('Ctrl Pts',(-40.939440247702,7.78353023681697,-2.19104319733171));
#17822=CARTESIAN_POINT('Ctrl Pts',(-41.4696829608985,7.71204397345954,-3.75949691436094));
#17823=CARTESIAN_POINT('Ctrl Pts',(-41.6872426574349,7.69422964594872,-4.26925519440169));
#17824=CARTESIAN_POINT('Ctrl Pts',(-42.1990770315599,7.66864299493069,-5.25006061898242));
#17825=CARTESIAN_POINT('Ctrl Pts',(-42.4923406104441,7.66112555225126,-5.7195922567623));
#17826=CARTESIAN_POINT('Ctrl Pts',(-42.8205093412364,7.65858862696564,-6.16441400296903));
#17827=CARTESIAN_POINT('',(-42.82044083094,7.65897167013792,6.16441400296897));
#17828=CARTESIAN_POINT('Ctrl Pts',(-40.7312208280702,7.95095276397636,0.));
#17829=CARTESIAN_POINT('Ctrl Pts',(-40.7496447782814,7.85657036643813,1.09861960926664));
#17830=CARTESIAN_POINT('Ctrl Pts',(-40.9391211892399,7.78409360993022,2.18971594132758));
#17831=CARTESIAN_POINT('Ctrl Pts',(-41.646611888365,7.68711804045621,4.28292314717358));
#17832=CARTESIAN_POINT('Ctrl Pts',(-42.1617834658437,7.66466315363683,5.27177304443359));
#17833=CARTESIAN_POINT('Ctrl Pts',(-42.8204408309399,7.6589716701379,6.16441400296898));
#17834=CARTESIAN_POINT('Origin',(-1.73472347597681E-15,-1.73472347597681E-15,
6.16441400296896));
#17835=CARTESIAN_POINT('Origin',(0.,0.,-6.93889390390723E-15));
#17836=CARTESIAN_POINT('',(-40.6009371733746,15.6145413203108,6.16441400296896));
#17837=CARTESIAN_POINT('',(-38.563893020008,15.3321934223837,0.));
#17838=CARTESIAN_POINT('Ctrl Pts',(-40.6009428427155,15.6145429094286,6.16442208586937));
#17839=CARTESIAN_POINT('Ctrl Pts',(-39.9773311258786,15.4397444431623,5.27532468973107));
#17840=CARTESIAN_POINT('Ctrl Pts',(-39.4861315168336,15.3208546842608,4.29109868658248));
#17841=CARTESIAN_POINT('Ctrl Pts',(-38.7939823618226,15.2221334915372,2.19783870908464));
#17842=CARTESIAN_POINT('Ctrl Pts',(-38.5995300332387,15.24255836966,1.1019979265306));
#17843=CARTESIAN_POINT('Ctrl Pts',(-38.5638930200079,15.3321934223837,2.77555756156289E-15));
#17844=CARTESIAN_POINT('',(-40.6009964209562,15.6143872638508,-6.16441400296897));
#17845=CARTESIAN_POINT('Ctrl Pts',(-40.6010020885999,15.6143888578416,-6.16442208610002));
#17846=CARTESIAN_POINT('Ctrl Pts',(-39.9772648207974,15.4389665558936,-5.27485402124692));
#17847=CARTESIAN_POINT('Ctrl Pts',(-39.4853557749724,15.3215914526481,-4.29007656912573));
#17848=CARTESIAN_POINT('Ctrl Pts',(-38.7936501568704,15.2226313606678,-2.19706468916282));
#17849=CARTESIAN_POINT('Ctrl Pts',(-38.60001241506,15.2413450715728,-1.10157448566469));
#17850=CARTESIAN_POINT('Ctrl Pts',(-38.5638930200079,15.3321934223837,5.55111512312578E-16));
#17851=CARTESIAN_POINT('',(-41.2947274963707,13.6746290991927,-6.16441400296902));
#17852=CARTESIAN_POINT('Origin',(-5.20417042793042E-15,1.73472347597681E-15,
-6.16441400296897));
#17853=CARTESIAN_POINT('',(-39.1850971728873,13.6666806339866,0.));
#17854=CARTESIAN_POINT('Ctrl Pts',(-39.1850971728873,13.6666806339865,2.08166817117217E-15));
#17855=CARTESIAN_POINT('Ctrl Pts',(-39.189102437885,13.6551967409812,-0.137043042091231));
#17856=CARTESIAN_POINT('Ctrl Pts',(-39.195681280223,13.6444567928563,-0.273914065094698));
#17857=CARTESIAN_POINT('Ctrl Pts',(-39.2139878587076,13.6244381186245,-0.547624684004344));
#17858=CARTESIAN_POINT('Ctrl Pts',(-39.2257153970297,13.6151666897426,-0.684384502468343));
#17859=CARTESIAN_POINT('Ctrl Pts',(-39.2686090832299,13.5895739808625,-1.0942291923894));
#17860=CARTESIAN_POINT('Ctrl Pts',(-39.3074646501152,13.5755014360956,-1.36653715783395));
#17861=CARTESIAN_POINT('Ctrl Pts',(-39.4546265164404,13.5422484035419,-2.17926357855595));
#17862=CARTESIAN_POINT('Ctrl Pts',(-39.593284520991,13.5321618341122,-2.71362913030224));
#17863=CARTESIAN_POINT('Ctrl Pts',(-39.9500430926314,13.5352977095237,-3.75949691623775));
#17864=CARTESIAN_POINT('Ctrl Pts',(-40.1679235882143,13.5486266792222,-4.26925519586518));
#17865=CARTESIAN_POINT('Ctrl Pts',(-40.6781895862499,13.5961420895901,-5.25006061966842));
#17866=CARTESIAN_POINT('Ctrl Pts',(-40.9695380082035,13.6304369224201,-5.71959225708742));
#17867=CARTESIAN_POINT('Ctrl Pts',(-41.2947274963707,13.6746290991927,-6.16441400296904));
#17868=CARTESIAN_POINT('',(-41.2946051706828,13.6749984935072,6.16441400296896));
#17869=CARTESIAN_POINT('Ctrl Pts',(-39.1850971728873,13.6666806339865,-8.32667268468867E-16));
#17870=CARTESIAN_POINT('Ctrl Pts',(-39.2167656094919,13.5758809146617,1.09861960926663));
#17871=CARTESIAN_POINT('Ctrl Pts',(-39.4146279416703,13.5311071718144,2.18971594132755));
#17872=CARTESIAN_POINT('Ctrl Pts',(-40.1287184680819,13.5358050982362,4.2829231471736));
#17873=CARTESIAN_POINT('Ctrl Pts',(-40.6418420053041,13.5868953295193,5.27177304443364));
#17874=CARTESIAN_POINT('Ctrl Pts',(-41.2946051706828,13.6749984935071,6.16441400296898));
#17875=CARTESIAN_POINT('Origin',(-1.73472347597681E-15,-1.73472347597681E-15,
6.16441400296896));
#17876=CARTESIAN_POINT('Origin',(0.,0.,-6.93889390390723E-15));
#17877=CARTESIAN_POINT('',(-37.9654972519552,21.2337236115521,6.16441400296896));
#17878=CARTESIAN_POINT('',(-35.989369566325,20.6643479988719,0.));
#17879=CARTESIAN_POINT('Ctrl Pts',(-37.9654972519552,21.2337236115521,6.16441400296898));
#17880=CARTESIAN_POINT('Ctrl Pts',(-37.373109418679,20.9719551410069,5.27531660683082));
#17881=CARTESIAN_POINT('Ctrl Pts',(-36.9038346756933,20.7843728952792,4.2910986865828));
#17882=CARTESIAN_POINT('Ctrl Pts',(-36.2327800916601,20.5881534468968,2.19783870908457));
#17883=CARTESIAN_POINT('Ctrl Pts',(-36.0374002441774,20.5806969775163,1.10199792653046));
#17884=CARTESIAN_POINT('Ctrl Pts',(-35.989369566325,20.6643479988719,1.66533453693773E-15));
#17885=CARTESIAN_POINT('',(-37.9655778209999,21.2335795549786,-6.16441400296897));
#17886=CARTESIAN_POINT('Ctrl Pts',(-37.9655778209998,21.2335795549787,-6.164414002969));
#17887=CARTESIAN_POINT('Ctrl Pts',(-37.3731544963908,20.9711757310147,-5.27484593906402));
#17888=CARTESIAN_POINT('Ctrl Pts',(-36.9029619776899,20.7849917652438,-4.29007657121778));
#17889=CARTESIAN_POINT('Ctrl Pts',(-36.2323804143448,20.5885989707591,-2.19706469153212));
#17890=CARTESIAN_POINT('Ctrl Pts',(-36.0380503864369,20.5795646790257,-1.10157448711653));
#17891=CARTESIAN_POINT('Ctrl Pts',(-35.989369566325,20.6643479988719,-2.4980018054066E-15));
#17892=CARTESIAN_POINT('',(-38.92830408384,19.4122935573335,-6.16441400296897));
#17893=CARTESIAN_POINT('Origin',(-5.20417042793042E-15,1.73472347597681E-15,
-6.16441400296897));
#17894=CARTESIAN_POINT('',(-36.8412779397533,19.1041942977412,0.));
#17895=CARTESIAN_POINT('Ctrl Pts',(-36.8412779397533,19.1041942977412,1.56125112837913E-15));
#17896=CARTESIAN_POINT('Ctrl Pts',(-36.8468754499426,19.0933998394437,-0.137010845862136));
#17897=CARTESIAN_POINT('Ctrl Pts',(-36.85491331931,19.0837074965195,-0.273849719843199));
#17898=CARTESIAN_POINT('Ctrl Pts',(-36.8758752981302,19.0665008944353,-0.547496131370911));
#17899=CARTESIAN_POINT('Ctrl Pts',(-36.8887981733475,19.0589938273842,-0.684223919463285));
#17900=CARTESIAN_POINT('Ctrl Pts',(-36.9348797930799,19.0397674368009,-1.09397285881179));
#17901=CARTESIAN_POINT('Ctrl Pts',(-36.9753262536641,19.0313667108818,-1.36621764183654));
#17902=CARTESIAN_POINT('Ctrl Pts',(-37.1256601264042,19.0193858351339,-2.17875768610691));
#17903=CARTESIAN_POINT('Ctrl Pts',(-37.2642828595668,19.0291203079234,-2.71300426677318));
#17904=CARTESIAN_POINT('Ctrl Pts',(-37.6168941909717,19.082964194744,-3.75889728641727));
#17905=CARTESIAN_POINT('Ctrl Pts',(-37.8306847292239,19.127164138192,-4.26878718251841));
#17906=CARTESIAN_POINT('Ctrl Pts',(-38.3290788364577,19.2468276666523,-5.24984087225394));
#17907=CARTESIAN_POINT('Ctrl Pts',(-38.6126451863175,19.32225227825,-5.71949644942051));
#17908=CARTESIAN_POINT('Ctrl Pts',(-38.9283097929753,19.4122951858561,-6.1644220499366));
#17909=CARTESIAN_POINT('',(-38.9281304329582,19.4126417829877,6.16441400296896));
#17910=CARTESIAN_POINT('Ctrl Pts',(-36.8412779397533,19.1041942977412,-1.11022302462516E-15));
#17911=CARTESIAN_POINT('Ctrl Pts',(-36.8855461847064,19.0188256770705,1.09861960926665));
#17912=CARTESIAN_POINT('Ctrl Pts',(-37.0877665316094,19.0026664121713,2.18971594132759));
#17913=CARTESIAN_POINT('Ctrl Pts',(-37.7939200614566,19.1089421982548,4.28292314717358));
#17914=CARTESIAN_POINT('Ctrl Pts',(-38.2945498429305,19.2325374978634,5.27177304443359));
#17915=CARTESIAN_POINT('Ctrl Pts',(-38.9281304329581,19.4126417829877,6.16441400296898));
#17916=CARTESIAN_POINT('Origin',(-1.73472347597681E-15,-1.73472347597681E-15,
6.16441400296896));
#17917=CARTESIAN_POINT('Origin',(0.,0.,-6.93889390390723E-15));
#17918=CARTESIAN_POINT('',(-34.5571892899392,26.4206485230646,6.16441400296896));
#17919=CARTESIAN_POINT('',(-32.6822063330433,25.5758360411618,0.));
#17920=CARTESIAN_POINT('Ctrl Pts',(-34.5571892899392,26.4206485230645,6.16441400296899));
#17921=CARTESIAN_POINT('Ctrl Pts',(-34.0080846482037,26.0772388994228,5.27531660683079));
#17922=CARTESIAN_POINT('Ctrl Pts',(-33.570282182427,25.8247812113316,4.29109868658273));
#17923=CARTESIAN_POINT('Ctrl Pts',(-32.9339829055411,25.5350579694094,2.19783870908454));
#17924=CARTESIAN_POINT('Ctrl Pts',(-32.7416529094252,25.4998719447395,1.10199792653037));
#17925=CARTESIAN_POINT('Ctrl Pts',(-32.6822063330432,25.5758360411618,2.22044604925031E-15));
#17926=CARTESIAN_POINT('',(-34.5572895403017,26.4205173989413,-6.16441400296897));
#17927=CARTESIAN_POINT('Ctrl Pts',(-34.5572895403017,26.4205173989413,-6.16441400296899));
#17928=CARTESIAN_POINT('Ctrl Pts',(-34.0082401881207,26.0764738375471,-5.27484593811451));
#17929=CARTESIAN_POINT('Ctrl Pts',(-33.5693302919162,25.8252695836891,-4.29007656912472));
#17930=CARTESIAN_POINT('Ctrl Pts',(-32.9335238913029,25.5354420784063,-2.19706468924495));
#17931=CARTESIAN_POINT('Ctrl Pts',(-32.7424575770002,25.4988436963698,-1.10157448610462));
#17932=CARTESIAN_POINT('Ctrl Pts',(-32.6822063330432,25.5758360411618,-2.22044604925031E-15));
#17933=CARTESIAN_POINT('',(-35.7694126601179,24.7547796990844,-6.16441400296897));
#17934=CARTESIAN_POINT('Origin',(-5.20417042793042E-15,1.73472347597681E-15,
-6.16441400296897));
#17935=CARTESIAN_POINT('',(-33.7474765292384,24.1528016575409,0.));
#17936=CARTESIAN_POINT('Ctrl Pts',(-33.7474765292383,24.1528016575408,1.59594559789866E-15));
#17937=CARTESIAN_POINT('Ctrl Pts',(-33.7545532764259,24.14291368003,-0.137010845725497));
#17938=CARTESIAN_POINT('Ctrl Pts',(-33.7638886960774,24.1344638992668,-0.273849719561638));
#17939=CARTESIAN_POINT('Ctrl Pts',(-33.7870860669391,24.1204156362138,-0.547496130807132));
#17940=CARTESIAN_POINT('Ctrl Pts',(-33.8009457729327,24.114824097178,-0.684223918759467));
#17941=CARTESIAN_POINT('Ctrl Pts',(-33.8492945488111,24.102351501781,-1.09397285769029));
#17942=CARTESIAN_POINT('Ctrl Pts',(-33.8905248706266,24.0997924146199,-1.3662176404398));
#17943=CARTESIAN_POINT('Ctrl Pts',(-34.0410336174364,24.1093282276174,-2.17875768389756));
#17944=CARTESIAN_POINT('Ctrl Pts',(-34.1768600108832,24.1386916892626,-2.7130042640453));
#17945=CARTESIAN_POINT('Ctrl Pts',(-34.5182194830287,24.2421693473779,-3.75889728380116));
#17946=CARTESIAN_POINT('Ctrl Pts',(-34.7235436341634,24.3163449650229,-4.268787180477));
#17947=CARTESIAN_POINT('Ctrl Pts',(-35.1998349126634,24.5057193681843,-5.24984087129627));
#17948=CARTESIAN_POINT('Ctrl Pts',(-35.4697758584422,24.6207297677425,-5.71948809597562));
#17949=CARTESIAN_POINT('Ctrl Pts',(-35.7694126601179,24.7547796990843,-6.164414002969));
#17950=CARTESIAN_POINT('',(-35.7691912190766,24.7550996672027,6.16441400296896));
#17951=CARTESIAN_POINT('Ctrl Pts',(-33.7474765292383,24.1528016575408,-1.94289029309402E-15));
#17952=CARTESIAN_POINT('Ctrl Pts',(-33.8034434087317,24.0746019944583,1.09861960926657));
#17953=CARTESIAN_POINT('Ctrl Pts',(-34.0059051472516,24.0873861635411,2.18971594132745));
#17954=CARTESIAN_POINT('Ctrl Pts',(-34.6897464310455,24.2930763407556,4.28292314717356));
#17955=CARTESIAN_POINT('Ctrl Pts',(-35.1676910781174,24.4866606648091,5.27177304443356));
#17956=CARTESIAN_POINT('Ctrl Pts',(-35.7691912190765,24.7550996672027,6.16441400296898));
#17957=CARTESIAN_POINT('Origin',(-1.73472347597681E-15,-1.73472347597681E-15,
6.16441400296896));
#17958=CARTESIAN_POINT('Origin',(0.,0.,-6.93889390390723E-15));
#17959=CARTESIAN_POINT('',(-30.4453966086847,31.0697252215061,6.16441400296896));
#17960=CARTESIAN_POINT('',(-28.709727626521,29.9666738162743,0.));
#17961=CARTESIAN_POINT('Ctrl Pts',(-30.4453966086847,31.0697252215061,6.16441400296899));
#17962=CARTESIAN_POINT('Ctrl Pts',(-29.9507533455086,30.6516652743936,5.27531660683076));
#17963=CARTESIAN_POINT('Ctrl Pts',(-29.553335552626,30.3394714544405,4.29109868658263));
#17964=CARTESIAN_POINT('Ctrl Pts',(-28.9647448012292,29.9621423486913,2.19783870908456));
#17965=CARTESIAN_POINT('Ctrl Pts',(-28.7793799405672,29.8999430547261,1.10199792653042));
#17966=CARTESIAN_POINT('Ctrl Pts',(-28.709727626521,29.9666738162743,8.32667268468867E-16));
#17967=CARTESIAN_POINT('',(-30.4455144995497,31.0696096991531,-6.16441400296897));
#17968=CARTESIAN_POINT('Ctrl Pts',(-30.4455144995497,31.0696096991531,-6.164414002969));
#17969=CARTESIAN_POINT('Ctrl Pts',(-29.9510161819033,30.650930135392,-5.27484593811665));
#17970=CARTESIAN_POINT('Ctrl Pts',(-29.5523238483592,30.3398193877234,-4.29007656912482));
#17971=CARTESIAN_POINT('Ctrl Pts',(-28.964235794694,29.9624572234644,-2.19706468924138));
#17972=CARTESIAN_POINT('Ctrl Pts',(-28.7803227527792,29.8990397885854,-1.10157448608512));
#17973=CARTESIAN_POINT('Ctrl Pts',(-28.709727626521,29.9666738162743,-1.66533453693773E-15));
#17974=CARTESIAN_POINT('',(-31.8823591451153,29.5933299130377,-6.16441400296897));
#17975=CARTESIAN_POINT('Origin',(-5.20417042793042E-15,1.73472347597681E-15,
-6.16441400296897));
#17976=CARTESIAN_POINT('',(-29.966673816274,28.7097276265214,0.));
#17977=CARTESIAN_POINT('Ctrl Pts',(-29.966673816274,28.7097276265213,3.46944695195361E-15));
#17978=CARTESIAN_POINT('Ctrl Pts',(-29.9750857383085,28.700947420486,-0.137010845869001));
#17979=CARTESIAN_POINT('Ctrl Pts',(-29.9855286660442,28.6939122150399,-0.273849719844409));
#17980=CARTESIAN_POINT('Ctrl Pts',(-30.0104891974366,28.683308273128,-0.547496131370688));
#17981=CARTESIAN_POINT('Ctrl Pts',(-30.0250035906016,28.6797460897162,-0.684223919463375));
#17982=CARTESIAN_POINT('Ctrl Pts',(-30.0746352811261,28.6742811955938,-1.09397285881368));
#17983=CARTESIAN_POINT('Ctrl Pts',(-30.1158101338558,28.677615842858,-1.36621764183967));
#17984=CARTESIAN_POINT('Ctrl Pts',(-30.2634298311996,28.7084742231121,-2.17875768611005));
#17985=CARTESIAN_POINT('Ctrl Pts',(-30.3936948517388,28.7568689184108,-2.71300426677516));
#17986=CARTESIAN_POINT('Ctrl Pts',(-30.7168533707347,28.9078738414552,-3.75889728641947));
#17987=CARTESIAN_POINT('Ctrl Pts',(-30.9095313269425,29.0105151315892,-4.26878718252155));
#17988=CARTESIAN_POINT('Ctrl Pts',(-31.3540238590941,29.2657452924843,-5.24984087225396));
#17989=CARTESIAN_POINT('Ctrl Pts',(-31.604849508625,29.4180016539176,-5.71948809642924));
#17990=CARTESIAN_POINT('Ctrl Pts',(-31.8823591451152,29.5933299130376,-6.16441400296899));
#17991=CARTESIAN_POINT('',(-31.8820944218041,29.5936151100059,6.16441400296896));
#17992=CARTESIAN_POINT('Ctrl Pts',(-29.966673816274,28.7097276265213,-1.66533453693773E-15));
#17993=CARTESIAN_POINT('Ctrl Pts',(-30.0332000060363,28.6402888406582,1.09861960926661));
#17994=CARTESIAN_POINT('Ctrl Pts',(-30.2317815990283,28.6817561949069,2.18971594132752));
#17995=CARTESIAN_POINT('Ctrl Pts',(-30.8793896002662,28.9826735044058,4.28292314717356));
#17996=CARTESIAN_POINT('Ctrl Pts',(-31.3249195382002,29.2423060343176,5.27177304443357));
#17997=CARTESIAN_POINT('Ctrl Pts',(-31.8820944218041,29.5936151100059,6.16441400296898));
#17998=CARTESIAN_POINT('Origin',(-1.73472347597681E-15,-1.73472347597681E-15,
6.16441400296896));
#17999=CARTESIAN_POINT('Origin',(0.,0.,-6.93889390390723E-15));
#18000=CARTESIAN_POINT('',(-25.7138234497511,35.0863119121265,6.16441400296896));
#18001=CARTESIAN_POINT('',(-24.1528016575405,33.7474765292386,0.));
#18002=CARTESIAN_POINT('Ctrl Pts',(-25.7138234497511,35.0863119121265,6.16441400296898));
#18003=CARTESIAN_POINT('Ctrl Pts',(-25.2837110755394,34.6021121364811,5.2753166068308));
#18004=CARTESIAN_POINT('Ctrl Pts',(-24.9347682357557,34.2365375505478,4.29109868658277));
#18005=CARTESIAN_POINT('Ctrl Pts',(-24.4058680201908,33.7792839134373,2.19783870908457));
#18006=CARTESIAN_POINT('Ctrl Pts',(-24.2312417889977,33.691337548434,1.10199792653045));
#18007=CARTESIAN_POINT('Ctrl Pts',(-24.1528016575405,33.7474765292386,8.32667268468867E-16));
#18008=CARTESIAN_POINT('',(-25.7139565811841,35.0862143432572,-6.16441400296897));
#18009=CARTESIAN_POINT('Ctrl Pts',(-25.713956581184,35.0862143432571,-6.164414002969));
#18010=CARTESIAN_POINT('Ctrl Pts',(-25.2840758578099,34.6014218856657,-5.27484593811654));
#18011=CARTESIAN_POINT('Ctrl Pts',(-24.9337173131132,34.2367379618409,-4.29007656912594));
#18012=CARTESIAN_POINT('Ctrl Pts',(-24.4053193832555,33.7795231440466,-2.19706468921581));
#18013=CARTESIAN_POINT('Ctrl Pts',(-24.2323035529049,33.6905776524152,-1.10157448595032));
#18014=CARTESIAN_POINT('Ctrl Pts',(-24.1528016575405,33.7474765292386,-2.77555756156289E-16));
#18015=CARTESIAN_POINT('',(-27.3462727390392,33.829445270091,-6.16441400296897));
#18016=CARTESIAN_POINT('Origin',(-5.20417042793042E-15,1.73472347597681E-15,
-6.16441400296897));
#18017=CARTESIAN_POINT('',(-25.5758360411614,32.6822063330436,0.));
#18018=CARTESIAN_POINT('Ctrl Pts',(-25.5758360411614,32.6822063330435,2.60208521396521E-15));
#18019=CARTESIAN_POINT('Ctrl Pts',(-25.5854118955599,32.6747126381701,-0.137010845868782));
#18020=CARTESIAN_POINT('Ctrl Pts',(-25.5967497434736,32.6692352245436,-0.273849719843329));
#18021=CARTESIAN_POINT('Ctrl Pts',(-25.6229653109245,32.662291469459,-0.54749613136761));
#18022=CARTESIAN_POINT('Ctrl Pts',(-25.6378389200515,32.6608311574538,-0.684223919459034));
#18023=CARTESIAN_POINT('Ctrl Pts',(-25.6877431670541,32.6624852140826,-1.09397285880905));
#18024=CARTESIAN_POINT('Ctrl Pts',(-25.7280243493679,32.6716457119514,-1.36621764183439));
#18025=CARTESIAN_POINT('Ctrl Pts',(-25.8697498856529,32.7231984717371,-2.17875768610485));
#18026=CARTESIAN_POINT('Ctrl Pts',(-25.991801712879,32.7896392241448,-2.71300426677193));
#18027=CARTESIAN_POINT('Ctrl Pts',(-26.290180702901,32.9850973871755,-3.7588972864174));
#18028=CARTESIAN_POINT('Ctrl Pts',(-26.4662900967129,33.1141148691595,-4.26878718251803));
#18029=CARTESIAN_POINT('Ctrl Pts',(-26.8699352967195,33.4300050378598,-5.24984087225432));
#18030=CARTESIAN_POINT('Ctrl Pts',(-27.0965395633502,33.6164078608134,-5.71948809642964));
#18031=CARTESIAN_POINT('Ctrl Pts',(-27.3462727390392,33.829445270091,-6.164414002969));
#18032=CARTESIAN_POINT('',(-27.3459701224718,33.8296898901081,6.16441400296896));
#18033=CARTESIAN_POINT('Ctrl Pts',(-25.5758360411614,32.6822063330435,-1.66533453693773E-15));
#18034=CARTESIAN_POINT('Ctrl Pts',(-25.6515672598148,32.6229419978349,1.09861960926661));
#18035=CARTESIAN_POINT('Ctrl Pts',(-25.8422261587077,32.6922483814991,2.18971594132752));
#18036=CARTESIAN_POINT('Ctrl Pts',(-26.4404174460316,33.0822670146349,4.2829231471735));
#18037=CARTESIAN_POINT('Ctrl Pts',(-26.8444629700937,33.4026623808144,5.27177304443351));
#18038=CARTESIAN_POINT('Ctrl Pts',(-27.3459701224718,33.829689890108,6.16441400296898));
#18039=CARTESIAN_POINT('Origin',(-1.73472347597681E-15,-1.73472347597681E-15,
6.16441400296896));
#18040=CARTESIAN_POINT('Origin',(0.,0.,-6.93889390390723E-15));
#18041=CARTESIAN_POINT('',(-20.4587909979241,38.3886424727844,6.16441400296896));
#18042=CARTESIAN_POINT('',(-19.1041942977416,36.8412779397542,-3.46944695195361E-15));
#18043=CARTESIAN_POINT('Ctrl Pts',(-20.458790997924,38.3886424727844,6.16441400296899));
#18044=CARTESIAN_POINT('Ctrl Pts',(-20.1019653602739,37.8481597797213,5.2753166068308));
#18045=CARTESIAN_POINT('Ctrl Pts',(-19.8086009435391,37.4366464721473,4.29109868658275));
#18046=CARTESIAN_POINT('Ctrl Pts',(-19.3501581469722,36.9087766691158,2.19783870908188));
#18047=CARTESIAN_POINT('Ctrl Pts',(-19.1898254317347,36.7968735674505,1.10199792652465));
#18048=CARTESIAN_POINT('Ctrl Pts',(-19.1041942977408,36.8412779397535,2.72004641033163E-14));
#18049=CARTESIAN_POINT('',(-20.4589366597763,38.3885648435998,-6.16441400296897));
#18050=CARTESIAN_POINT('Ctrl Pts',(-20.4589366597763,38.3885648435998,-6.16441400296901));
#18051=CARTESIAN_POINT('Ctrl Pts',(-20.1024246625312,37.8475284685869,-5.27484593811536));
#18052=CARTESIAN_POINT('Ctrl Pts',(-19.8075321962687,37.4366952816587,-4.29007656912531));
#18053=CARTESIAN_POINT('Ctrl Pts',(-19.3495810482861,36.9089353855174,-2.19706468916458));
#18054=CARTESIAN_POINT('Ctrl Pts',(-19.1909845328821,36.7962725108431,-1.10157448568023));
#18055=CARTESIAN_POINT('Ctrl Pts',(-19.1041942977408,36.8412779397535,-3.13638004456607E-14));
#18056=CARTESIAN_POINT('',(-22.2534950801163,37.3768906775195,-6.16441400296897));
#18057=CARTESIAN_POINT('Origin',(-5.20417042793042E-15,1.73472347597681E-15,
-6.16441400296897));
#18058=CARTESIAN_POINT('',(-20.6643479988715,35.9893695663253,0.));
#18059=CARTESIAN_POINT('Ctrl Pts',(-20.6643479988715,35.9893695663252,2.63677968348475E-15));
#18060=CARTESIAN_POINT('Ctrl Pts',(-20.6748928488527,35.983314932631,-0.137010845869154));
#18061=CARTESIAN_POINT('Ctrl Pts',(-20.6868948110568,35.9795068151698,-0.273849719847874));
#18062=CARTESIAN_POINT('Ctrl Pts',(-20.7138317412126,35.9763646017424,-0.5474961313763));
#18063=CARTESIAN_POINT('Ctrl Pts',(-20.7287617825115,35.9770358888855,-0.68422391946899));
#18064=CARTESIAN_POINT('Ctrl Pts',(-20.7779226794341,35.9857752244446,-1.09397285881967));
#18065=CARTESIAN_POINT('Ctrl Pts',(-20.8164901826204,36.0005750915999,-1.36621764184467));
#18066=CARTESIAN_POINT('Ctrl Pts',(-20.9494364346273,36.0717727653988,-2.1787576861109));
#18067=CARTESIAN_POINT('Ctrl Pts',(-21.0607904453043,36.1549070327976,-2.71300426677424));
#18068=CARTESIAN_POINT('Ctrl Pts',(-21.3283157705729,36.390839471264,-3.75889728641524));
#18069=CARTESIAN_POINT('Ctrl Pts',(-21.4842715225984,36.5436067212097,-4.26878718251598));
#18070=CARTESIAN_POINT('Ctrl Pts',(-21.8388523381951,36.9137262848343,-5.24984087225303));
#18071=CARTESIAN_POINT('Ctrl Pts',(-22.0366222125189,37.1304809453829,-5.71948809642907));
#18072=CARTESIAN_POINT('Ctrl Pts',(-22.2534950801163,37.3768906775195,-6.16441400296901));
#18073=CARTESIAN_POINT('',(-22.2531607307118,37.3770897408173,6.16441400296896));
#18074=CARTESIAN_POINT('Ctrl Pts',(-20.6643479988715,35.9893695663252,-5.55111512312578E-16));
#18075=CARTESIAN_POINT('Ctrl Pts',(-20.747742577195,35.9414861327319,1.09861960926664));
#18076=CARTESIAN_POINT('Ctrl Pts',(-20.9265975166221,36.0372206677032,2.18971594132757));
#18077=CARTESIAN_POINT('Ctrl Pts',(-21.4631946404634,36.5084009698261,4.28292314717356));
#18078=CARTESIAN_POINT('Ctrl Pts',(-21.8175305489547,36.8830368465618,5.27177304443358));
#18079=CARTESIAN_POINT('Ctrl Pts',(-22.2531607307118,37.3770897408172,6.16441400296897));
#18080=CARTESIAN_POINT('Origin',(-1.73472347597681E-15,-1.73472347597681E-15,
6.16441400296896));
#18081=CARTESIAN_POINT('Origin',(0.,0.,-6.93889390390723E-15));
#18082=CARTESIAN_POINT('',(-14.7872765596605,40.9094909763996,6.16441400296896));
#18083=CARTESIAN_POINT('',(-13.6666806339862,39.1850971728874,0.));
#18084=CARTESIAN_POINT('Ctrl Pts',(-14.7872765596605,40.9094909763996,6.16441400296899));
#18085=CARTESIAN_POINT('Ctrl Pts',(-14.5110015995543,40.3237280349262,5.27531660683078));
#18086=CARTESIAN_POINT('Ctrl Pts',(-14.2791876594001,39.8746532299474,4.29109868658268));
#18087=CARTESIAN_POINT('Ctrl Pts',(-13.9005348551306,39.2869131679352,2.19783870908465));
#18088=CARTESIAN_POINT('Ctrl Pts',(-13.7577595675692,39.153331354054,1.10199792653061));
#18089=CARTESIAN_POINT('Ctrl Pts',(-13.6666806339861,39.1850971728874,-5.55111512312578E-16));
#18090=CARTESIAN_POINT('',(-14.7874317866676,40.9094348672119,-6.16441400296897));
#18091=CARTESIAN_POINT('Ctrl Pts',(-14.7874317866676,40.9094348672119,-6.164414002969));
#18092=CARTESIAN_POINT('Ctrl Pts',(-14.5115460717139,40.3231685151577,-5.27484593811608));
#18093=CARTESIAN_POINT('Ctrl Pts',(-14.2781228441205,39.8745494440526,-4.29007656912554));
#18094=CARTESIAN_POINT('Ctrl Pts',(-13.8999410427714,39.2869881391078,-2.19706468910641));
#18095=CARTESIAN_POINT('Ctrl Pts',(-13.7589924099841,39.1529013726383,-1.1015744853717));
#18096=CARTESIAN_POINT('Ctrl Pts',(-13.6666806339861,39.1850971728874,-8.32667268468867E-16));
#18097=CARTESIAN_POINT('',(-16.7077004351661,40.1634503767885,-6.16441400296897));
#18098=CARTESIAN_POINT('Origin',(-5.20417042793042E-15,1.73472347597681E-15,
-6.16441400296897));
#18099=CARTESIAN_POINT('',(-15.3321934223833,38.5638930200081,0.));
#18100=CARTESIAN_POINT('Ctrl Pts',(-15.3321934223833,38.5638930200081,1.2490009027033E-15));
#18101=CARTESIAN_POINT('Ctrl Pts',(-15.3434926052115,38.5594007023744,-0.137010845860815));
#18102=CARTESIAN_POINT('Ctrl Pts',(-15.3559143563672,38.5573394033676,-0.273849719841542));
#18103=CARTESIAN_POINT('Ctrl Pts',(-15.3830242910103,38.5580626980003,-0.547496131368016));
#18104=CARTESIAN_POINT('Ctrl Pts',(-15.3977068318951,38.5608519188208,-0.684223919460011));
#18105=CARTESIAN_POINT('Ctrl Pts',(-15.4451236046443,38.5764986256395,-1.09397285880962));
#18106=CARTESIAN_POINT('Ctrl Pts',(-15.4811923055565,38.5966365794654,-1.36621764183523));
#18107=CARTESIAN_POINT('Ctrl Pts',(-15.6026528709759,38.6860297879581,-2.17875768610564));
#18108=CARTESIAN_POINT('Ctrl Pts',(-15.7010422185607,38.7841651964068,-2.71300426677201));
#18109=CARTESIAN_POINT('Ctrl Pts',(-15.9322678349351,39.0557690062366,-3.75889728641666));
#18110=CARTESIAN_POINT('Ctrl Pts',(-16.0648951358121,39.2291761234751,-4.26878718251826));
#18111=CARTESIAN_POINT('Ctrl Pts',(-16.3631933241338,39.6459905150347,-5.2498408722538));
#18112=CARTESIAN_POINT('Ctrl Pts',(-16.5281027818355,39.8886845133532,-5.71948809642935));
#18113=CARTESIAN_POINT('Ctrl Pts',(-16.7077004351661,40.1634503767885,-6.16441400296899));
#18114=CARTESIAN_POINT('',(-16.7073411592909,40.1635998310295,6.16441400296896));
#18115=CARTESIAN_POINT('Ctrl Pts',(-15.3321934223833,38.5638930200081,-1.38777878078145E-15));
#18116=CARTESIAN_POINT('Ctrl Pts',(-15.4215536872523,38.5283652566535,1.09861960926664));
#18117=CARTESIAN_POINT('Ctrl Pts',(-15.5849636964219,38.6485790638755,2.18971594132757));
#18118=CARTESIAN_POINT('Ctrl Pts',(-16.0490430867575,39.1913291628061,4.28292314717355));
#18119=CARTESIAN_POINT('Ctrl Pts',(-16.3464561224015,39.6125790440083,5.27177304443356));
#18120=CARTESIAN_POINT('Ctrl Pts',(-16.7073411592909,40.1635998310294,6.16441400296897));
#18121=CARTESIAN_POINT('Origin',(-1.73472347597681E-15,-1.73472347597681E-15,
6.16441400296896));
#18122=CARTESIAN_POINT('Origin',(0.,0.,-6.93889390390723E-15));
#18123=CARTESIAN_POINT('',(-8.81473581362657,42.5975402169653,6.16441400296896));
#18124=CARTESIAN_POINT('',(-7.95095276397595,40.7312208280703,0.));
#18125=CARTESIAN_POINT('Ctrl Pts',(-8.81473754185273,42.5975458454602,6.16442208586935));
#18126=CARTESIAN_POINT('Ctrl Pts',(-8.62463742076709,41.9784270998641,5.27532468973107));
#18127=CARTESIAN_POINT('Ctrl Pts',(-8.45909129229247,41.5009270369901,4.29109868658251));
#18128=CARTESIAN_POINT('Ctrl Pts',(-8.16793675947019,40.8652814087567,2.19783870908467));
#18129=CARTESIAN_POINT('Ctrl Pts',(-8.04562539271004,40.712740223173,1.10199792653066));
#18130=CARTESIAN_POINT('Ctrl Pts',(-7.95095276397594,40.7312208280702,2.77555756156289E-15));
#18131=CARTESIAN_POINT('',(-8.81489744582791,42.5975067699923,-6.16441400296897));
#18132=CARTESIAN_POINT('Ctrl Pts',(-8.8148974458279,42.5975067699923,-6.164414002969));
#18133=CARTESIAN_POINT('Ctrl Pts',(-8.62525425073438,41.9779451331706,-5.27484593811627));
#18134=CARTESIAN_POINT('Ctrl Pts',(-8.45805208556847,41.500672768472,-4.29007656912508));
#18135=CARTESIAN_POINT('Ctrl Pts',(-8.16733832174611,40.8652711085092,-2.19706468906603));
#18136=CARTESIAN_POINT('Ctrl Pts',(-8.046906879285,40.7124900701204,-1.10157448515744));
#18137=CARTESIAN_POINT('Ctrl Pts',(-7.95095276397593,40.7312208280702,-1.38777878078145E-15));
#18138=CARTESIAN_POINT('',(-10.8217851903811,42.1323980482153,-6.16441400296897));
#18139=CARTESIAN_POINT('Origin',(-5.20417042793042E-15,1.73472347597681E-15,
-6.16441400296897));
#18140=CARTESIAN_POINT('',(-9.68791960221003,40.3533668208877,1.04083408558608E-14));
#18141=CARTESIAN_POINT('Ctrl Pts',(-9.68791960221003,40.3533668208876,1.21777588013572E-14));
#18142=CARTESIAN_POINT('Ctrl Pts',(-9.6997430991055,40.3505282699472,-0.137010845855937));
#18143=CARTESIAN_POINT('Ctrl Pts',(-9.71233176817975,40.3502557514989,-0.273849719840574));
#18144=CARTESIAN_POINT('Ctrl Pts',(-9.7390628272182,40.3548298299997,-0.547496131367697));
#18145=CARTESIAN_POINT('Ctrl Pts',(-9.75319897349705,40.3596802040055,-0.68422391945948));
#18146=CARTESIAN_POINT('Ctrl Pts',(-9.79790635331839,40.3819157602545,-1.09397285880777));
#18147=CARTESIAN_POINT('Ctrl Pts',(-9.83074199722052,40.4069818500838,-1.36621764183255));
#18148=CARTESIAN_POINT('Ctrl Pts',(-9.93824428920808,40.5127508053321,-2.17875768610361));
#18149=CARTESIAN_POINT('Ctrl Pts',(-10.0216660503199,40.6238896009114,-2.71300426677103));
#18150=CARTESIAN_POINT('Ctrl Pts',(-10.2118848710492,40.9256357117768,-3.75889728641691));
#18151=CARTESIAN_POINT('Ctrl Pts',(-10.3184838113872,41.1161526274701,-4.26878718251867));
#18152=CARTESIAN_POINT('Ctrl Pts',(-10.5544268815369,41.5711767079492,-5.24984087225478));
#18153=CARTESIAN_POINT('Ctrl Pts',(-10.6831188416198,41.8348694941026,-5.71948809642984));
#18154=CARTESIAN_POINT('Ctrl Pts',(-10.8217851903811,42.1323980482152,-6.164414002969));
#18155=CARTESIAN_POINT('',(-10.82140830186,42.1324948509394,6.16441400296896));
#18156=CARTESIAN_POINT('Ctrl Pts',(-9.68791960221004,40.3533668208876,9.15933995315754E-15));
#18157=CARTESIAN_POINT('Ctrl Pts',(-9.78142643632559,40.3309179705801,1.09861960926654));
#18158=CARTESIAN_POINT('Ctrl Pts',(-9.92606495868656,40.4731638436057,2.18971594132738));
#18159=CARTESIAN_POINT('Ctrl Pts',(-10.3081792974237,41.0764349124918,4.2829231471736));
#18160=CARTESIAN_POINT('Ctrl Pts',(-10.5426149884832,41.5357233653637,5.27177304443365));
#18161=CARTESIAN_POINT('Ctrl Pts',(-10.82140830186,42.1324948509394,6.16441400296898));
#18162=CARTESIAN_POINT('Origin',(-1.73472347597681E-15,-1.73472347597681E-15,
6.16441400296896));
#18163=CARTESIAN_POINT('Origin',(0.,0.,-6.93889390390723E-15));
#18164=CARTESIAN_POINT('',(-2.66275246602648,43.4184263798755,6.16441400296896));
#18165=CARTESIAN_POINT('',(-2.07336642434587,41.448174286335,0.));
#18166=CARTESIAN_POINT('Ctrl Pts',(-2.66275246602647,43.4184263798755,6.16441400296898));
#18167=CARTESIAN_POINT('Ctrl Pts',(-2.56269707422321,42.7785553024261,5.27531660683073));
#18168=CARTESIAN_POINT('Ctrl Pts',(-2.46679222047902,42.2823616483505,4.29109868658259));
#18169=CARTESIAN_POINT('Ctrl Pts',(-2.26906302577184,41.611750365836,2.19783870908463));
#18170=CARTESIAN_POINT('Ctrl Pts',(-2.16970548652324,41.4433551071959,1.1019979265306));
#18171=CARTESIAN_POINT('Ctrl Pts',(-2.07336642434585,41.4481742863349,1.38777878078145E-15));
#18172=CARTESIAN_POINT('',(-2.66291721304304,43.4184162760053,-6.16441400296898));
#18173=CARTESIAN_POINT('Ctrl Pts',(-2.66291721304302,43.4184162760053,-6.16441400296899));
#18174=CARTESIAN_POINT('Ctrl Pts',(-2.56337712638027,42.7781718426724,-5.27484593811571));
#18175=CARTESIAN_POINT('Ctrl Pts',(-2.46579977756426,42.2819620733826,-4.29007656912569));
#18176=CARTESIAN_POINT('Ctrl Pts',(-2.26847214514445,41.6116550038393,-2.197064688993));
#18177=CARTESIAN_POINT('Ctrl Pts',(-2.17100952986355,41.4432898748974,-1.1015744847684));
#18178=CARTESIAN_POINT('Ctrl Pts',(-2.07336642434585,41.4481742863349,-1.66533453693773E-15));
#18179=CARTESIAN_POINT('',(-4.71556960658337,43.2436515951818,-6.16441400296897));
#18180=CARTESIAN_POINT('Origin',(-5.20417042793042E-15,1.73472347597681E-15,
-6.16441400296897));
#18181=CARTESIAN_POINT('',(-3.84642767658888,41.3213624427944,0.));
#18182=CARTESIAN_POINT('Ctrl Pts',(-3.8464276765889,41.3213624427943,2.35922392732846E-15));
#18183=CARTESIAN_POINT('Ctrl Pts',(-3.85853479525186,41.3202354432581,-0.137010845849856));
#18184=CARTESIAN_POINT('Ctrl Pts',(-3.87103411324552,41.321757253058,-0.273849719835895));
#18185=CARTESIAN_POINT('Ctrl Pts',(-3.89684212940387,41.3300890003785,-0.547496131360071));
#18186=CARTESIAN_POINT('Ctrl Pts',(-3.91014410990392,41.3369017879418,-0.684223919450046));
#18187=CARTESIAN_POINT('Ctrl Pts',(-3.95123198346989,41.3652735418179,-1.09397285879913));
#18188=CARTESIAN_POINT('Ctrl Pts',(-3.98016613134168,41.3947574943464,-1.36621764182406));
#18189=CARTESIAN_POINT('Ctrl Pts',(-4.07152171324077,41.5147490454345,-2.17875768609805));
#18190=CARTESIAN_POINT('Ctrl Pts',(-4.13827766138895,41.6366287627654,-2.71300426676847));
#18191=CARTESIAN_POINT('Ctrl Pts',(-4.28361737982964,41.9623744940143,-3.75889728641876));
#18192=CARTESIAN_POINT('Ctrl Pts',(-4.36201791261577,42.1661228331631,-4.26878718252147));
#18193=CARTESIAN_POINT('Ctrl Pts',(-4.53080274409615,42.6500936244629,-5.24984087225698));
#18194=CARTESIAN_POINT('Ctrl Pts',(-4.62065740937212,42.9294171737523,-5.71948809643096));
#18195=CARTESIAN_POINT('Ctrl Pts',(-4.71556960658338,43.2436515951818,-6.164414002969));
#18196=CARTESIAN_POINT('',(-4.71518277776789,43.2436937757662,6.16441400296896));
#18197=CARTESIAN_POINT('Ctrl Pts',(-3.84642767658889,41.3213624427943,-1.66533453693773E-15));
#18198=CARTESIAN_POINT('Ctrl Pts',(-3.94217755045982,41.3124494993889,1.09861960926671));
#18199=CARTESIAN_POINT('Ctrl Pts',(-4.06510016280003,41.4738317224468,2.18971594132769));
#18200=CARTESIAN_POINT('Ctrl Pts',(-4.35747070392864,42.1253429020159,4.28292314717349));
#18201=CARTESIAN_POINT('Ctrl Pts',(-4.52415661579022,42.6133201381352,5.27177304443345));
#18202=CARTESIAN_POINT('Ctrl Pts',(-4.71518277776791,43.2436937757662,6.16441400296897));
#18203=CARTESIAN_POINT('Origin',(-1.73472347597681E-15,-1.73472347597681E-15,
6.16441400296896));
#18204=CARTESIAN_POINT('Origin',(0.,0.,-6.93889390390723E-15));
#18205=CARTESIAN_POINT('',(3.54343684303851,43.3554385900939,6.16441400296897));
#18206=CARTESIAN_POINT('',(3.84642767658947,41.3213624427943,0.));
#18207=CARTESIAN_POINT('Ctrl Pts',(3.54343684303853,43.3554385900938,6.16441400296898));
#18208=CARTESIAN_POINT('Ctrl Pts',(3.55141066631822,42.7078411106921,5.27531660683074));
#18209=CARTESIAN_POINT('Ctrl Pts',(3.57572362730268,42.2030493088126,4.29109868658261));
#18210=CARTESIAN_POINT('Ctrl Pts',(3.67600228769439,41.5111240838458,2.1978387090846));
#18211=CARTESIAN_POINT('Ctrl Pts',(3.75038336645583,41.3303027940033,1.10199792653051));
#18212=CARTESIAN_POINT('Ctrl Pts',(3.84642767658948,41.3213624427942,2.77555756156289E-16));
#18213=CARTESIAN_POINT('',(3.54327233497914,43.3554520350114,-6.16441400296898));
#18214=CARTESIAN_POINT('Ctrl Pts',(3.54327233497913,43.3554520350114,-6.16441400296901));
#18215=CARTESIAN_POINT('Ctrl Pts',(3.55068296410195,42.7075583355186,-5.27484593811621));
#18216=CARTESIAN_POINT('Ctrl Pts',(3.57664910313154,42.2025125615888,-4.29007656912535));
#18217=CARTESIAN_POINT('Ctrl Pts',(3.6765735825726,41.5109456014396,-2.19706468906318));
#18218=CARTESIAN_POINT('Ctrl Pts',(3.74908331283908,41.3304238103958,-1.1015744851416));
#18219=CARTESIAN_POINT('Ctrl Pts',(3.84642767658949,41.3213624427942,-8.32667268468867E-16));
#18220=CARTESIAN_POINT('',(1.48664137583834,43.4745891000668,-6.16441400296897));
#18221=CARTESIAN_POINT('Origin',(-5.20417042793042E-15,1.73472347597681E-15,
-6.16441400296897));
#18222=CARTESIAN_POINT('',(2.07336642434584,41.448174286335,0.));
#18223=CARTESIAN_POINT('Ctrl Pts',(2.07336642434582,41.4481742863349,1.80411241501588E-15));
#18224=CARTESIAN_POINT('Ctrl Pts',(2.06122214993787,41.4487817806634,-0.137010845843175));
#18225=CARTESIAN_POINT('Ctrl Pts',(2.04906663309415,41.4520669390525,-0.273849719833891));
#18226=CARTESIAN_POINT('Ctrl Pts',(2.02470703660085,41.4639867448445,-0.547496131359161));
#18227=CARTESIAN_POINT('Ctrl Pts',(2.01251001184276,41.4726232572572,-0.684223919449438));
#18228=CARTESIAN_POINT('Ctrl Pts',(1.97587807515069,41.5065536416689,-1.09397285879738));
#18229=CARTESIAN_POINT('Ctrl Pts',(1.95143443912054,41.5398552486479,-1.36621764182242));
#18230=CARTESIAN_POINT('Ctrl Pts',(1.8780853035088,41.6716267136228,-2.17875768609688));
#18231=CARTESIAN_POINT('Ctrl Pts',(1.82935412691927,41.8017662331319,-2.71300426676794));
#18232=CARTESIAN_POINT('Ctrl Pts',(1.73185220830974,42.144880341048,-3.75889728641881));
#18233=CARTESIAN_POINT('Ctrl Pts',(1.68324609183628,42.3577123750292,-4.26878718252151));
#18234=CARTESIAN_POINT('Ctrl Pts',(1.58505547146645,42.8607776274967,-5.24984087225669));
#18235=CARTESIAN_POINT('Ctrl Pts',(1.53586728286775,43.1500457179624,-5.7194880964307));
#18236=CARTESIAN_POINT('Ctrl Pts',(1.48664137583833,43.4745891000668,-6.164414002969));
#18237=CARTESIAN_POINT('',(1.48703027021497,43.4745757998335,6.16441400296896));
#18238=CARTESIAN_POINT('Ctrl Pts',(2.07336642434583,41.4481742863349,-2.22044604925031E-15));
#18239=CARTESIAN_POINT('Ctrl Pts',(1.97732270203171,41.4529786916566,1.09861960926666));
#18240=CARTESIAN_POINT('Ctrl Pts',(1.87861834962003,41.630211988073,2.18971594132761));
#18241=CARTESIAN_POINT('Ctrl Pts',(1.6819434271902,42.3167003895122,4.28292314717354));
#18242=CARTESIAN_POINT('Ctrl Pts',(1.58640053900949,42.8234325995621,5.27177304443355));
#18243=CARTESIAN_POINT('Ctrl Pts',(1.48703027021496,43.4745757998335,6.16441400296897));
#18244=CARTESIAN_POINT('Origin',(-1.73472347597681E-15,-1.73472347597681E-15,
6.16441400296896));
#18245=CARTESIAN_POINT('Origin',(0.,0.,-6.93889390390723E-15));
#18246=CARTESIAN_POINT('',(9.67749199640695,42.4098590973783,6.16441400296896));
#18247=CARTESIAN_POINT('',(9.68791960221059,40.3533668208876,0.));
#18248=CARTESIAN_POINT('Ctrl Pts',(9.67749199640696,42.4098590973783,6.164414002969));
#18249=CARTESIAN_POINT('Ctrl Pts',(9.59322192711572,41.7677184331879,5.27531660683075));
#18250=CARTESIAN_POINT('Ctrl Pts',(9.54544805356759,41.2646045888914,4.29109868658259));
#18251=CARTESIAN_POINT('Ctrl Pts',(9.54623479529805,40.5654510237051,2.19783870908456));
#18252=CARTESIAN_POINT('Ctrl Pts',(9.59412522930608,40.3758847026759,1.10199792653043));
#18253=CARTESIAN_POINT('Ctrl Pts',(9.6879196022106,40.3533668208875,1.38777878078145E-15));
#18254=CARTESIAN_POINT('',(9.67733107622405,42.4098958173815,-6.16441400296897));
#18255=CARTESIAN_POINT('Ctrl Pts',(9.67733107622405,42.4098958173815,-6.16441400296901));
#18256=CARTESIAN_POINT('Ctrl Pts',(9.59246138876394,41.767542099079,-5.2748459381158));
#18257=CARTESIAN_POINT('Ctrl Pts',(9.54628772229279,41.2639415960375,-4.29007656912554));
#18258=CARTESIAN_POINT('Ctrl Pts',(9.54677487451954,40.5651930542696,-2.19706468910642));
#18259=CARTESIAN_POINT('Ctrl Pts',(9.59285563076488,40.376189504222,-1.10157448537283));
#18260=CARTESIAN_POINT('Ctrl Pts',(9.68791960221059,40.3533668208875,0.));
#18261=CARTESIAN_POINT('',(7.6585886269646,42.8205093412366,-6.16441400296898));
#18262=CARTESIAN_POINT('Origin',(-5.20417042793042E-15,1.73472347597681E-15,
-6.16441400296897));
#18263=CARTESIAN_POINT('',(7.95095276397653,40.7312208280702,0.));
#18264=CARTESIAN_POINT('Ctrl Pts',(7.95095276397649,40.7312208280701,2.98372437868011E-15));
#18265=CARTESIAN_POINT('Ctrl Pts',(7.93901855622804,40.7335504494307,-0.137010845850136));
#18266=CARTESIAN_POINT('Ctrl Pts',(7.92745429180435,40.738532080058,-0.273849719836056));
#18267=CARTESIAN_POINT('Ctrl Pts',(7.90503900611341,40.7537972914492,-0.547496131360746));
#18268=CARTESIAN_POINT('Ctrl Pts',(7.89419523334797,40.7640817142243,-0.684223919451336));
#18269=CARTESIAN_POINT('Ctrl Pts',(7.86276495412265,40.8028800043923,-1.09397285879932));
#18270=CARTESIAN_POINT('Ctrl Pts',(7.84330943187384,40.8393213411377,-1.36621764182423));
#18271=CARTESIAN_POINT('Ctrl Pts',(7.78945991942847,40.9801902329702,-2.17875768609855));
#18272=CARTESIAN_POINT('Ctrl Pts',(7.75974554062361,41.1159402893316,-2.71300426676885));
#18273=CARTESIAN_POINT('Ctrl Pts',(7.71206627973686,41.4694379601366,-3.75889728641854));
#18274=CARTESIAN_POINT('Ctrl Pts',(7.6942440599413,41.6870210424949,-4.26878718252084));
#18275=CARTESIAN_POINT('Ctrl Pts',(7.66864652855301,42.1989397983105,-5.24984087225615));
#18276=CARTESIAN_POINT('Ctrl Pts',(7.66112614630197,42.4922637658111,-5.71948809643045));
#18277=CARTESIAN_POINT('Ctrl Pts',(7.65858862696456,42.8205093412366,-6.164414002969));
#18278=CARTESIAN_POINT('',(7.65897167013808,42.8204408309399,6.16441400296896));
#18279=CARTESIAN_POINT('Ctrl Pts',(7.95095276397651,40.7312208280701,2.77555756156289E-16));
#18280=CARTESIAN_POINT('Ctrl Pts',(7.85657036643829,40.7496447782813,1.09861960926667));
#18281=CARTESIAN_POINT('Ctrl Pts',(7.78409360993039,40.9391211892399,2.18971594132763));
#18282=CARTESIAN_POINT('Ctrl Pts',(7.68711804045638,41.646611888365,4.28292314717352));
#18283=CARTESIAN_POINT('Ctrl Pts',(7.66466315363699,42.1617834658436,5.27177304443353));
#18284=CARTESIAN_POINT('Ctrl Pts',(7.65897167013807,42.8204408309399,6.16441400296898));
#18285=CARTESIAN_POINT('Origin',(-1.73472347597681E-15,-1.73472347597681E-15,
6.16441400296896));
#18286=CARTESIAN_POINT('Origin',(0.,0.,-6.93889390390723E-15));
#18287=CARTESIAN_POINT('',(15.6145413203109,40.6009371733745,6.16441400296896));
#18288=CARTESIAN_POINT('',(15.3321934223838,38.5638930200079,0.));
#18289=CARTESIAN_POINT('Ctrl Pts',(15.6145413203109,40.6009371733745,6.16441400296897));
#18290=CARTESIAN_POINT('Ctrl Pts',(15.4397428540447,39.9773254565376,5.27531660683071));
#18291=CARTESIAN_POINT('Ctrl Pts',(15.320854684261,39.4861315168335,4.29109868658256));
#18292=CARTESIAN_POINT('Ctrl Pts',(15.2221334915373,38.7939823618225,2.1978387090846));
#18293=CARTESIAN_POINT('Ctrl Pts',(15.2425583696601,38.5995300332387,1.10199792653053));
#18294=CARTESIAN_POINT('Ctrl Pts',(15.3321934223838,38.5638930200079,2.4980018054066E-15));
#18295=CARTESIAN_POINT('',(15.6143872638506,40.6009964209563,-6.16441400296898));
#18296=CARTESIAN_POINT('Ctrl Pts',(15.6143872638506,40.6009964209562,-6.16441400296901));
#18297=CARTESIAN_POINT('Ctrl Pts',(15.4389649620045,39.9772591535156,-5.27484593863204));
#18298=CARTESIAN_POINT('Ctrl Pts',(15.321591452786,39.4853557755399,-4.29007657026461));
#18299=CARTESIAN_POINT('Ctrl Pts',(15.2474362658641,38.9670300715335,-2.72168992255469));
#18300=CARTESIAN_POINT('Ctrl Pts',(15.2397716853914,38.8316817981346,-2.18495234743865));
#18301=CARTESIAN_POINT('Ctrl Pts',(15.2546174490221,38.6871424443347,-1.36923477589022));
#18302=CARTESIAN_POINT('Ctrl Pts',(15.2639350598672,38.648771103302,-1.09614446426196));
#18303=CARTESIAN_POINT('Ctrl Pts',(15.2845589828127,38.6059128200838,-0.685318587195841));
#18304=CARTESIAN_POINT('Ctrl Pts',(15.2925330768462,38.5940831817694,-0.548301186445323));
#18305=CARTESIAN_POINT('Ctrl Pts',(15.3107031781166,38.5753179353705,-0.274113036182014));
#18306=CARTESIAN_POINT('Ctrl Pts',(15.3208920224688,38.5683862191086,-0.137034229960439));
#18307=CARTESIAN_POINT('Ctrl Pts',(15.3321934223838,38.5638930200079,3.46944695195361E-17));
#18308=CARTESIAN_POINT('',(13.6746290992085,41.2947274963655,-6.16441400296897));
#18309=CARTESIAN_POINT('Origin',(-5.20417042793042E-15,1.73472347597681E-15,
-6.16441400296897));
#18310=CARTESIAN_POINT('',(13.6666806339867,39.1850971728872,0.));
#18311=CARTESIAN_POINT('Ctrl Pts',(13.6666806339867,39.1850971728872,1.83880688453542E-15));
#18312=CARTESIAN_POINT('Ctrl Pts',(13.6551994389513,39.1891014969075,-0.137010845854186));
#18313=CARTESIAN_POINT('Ctrl Pts',(13.6444618420215,39.1956781881393,-0.273849719837921));
#18314=CARTESIAN_POINT('Ctrl Pts',(13.6244471777075,39.2139780494479,-0.547496131363585));
#18315=CARTESIAN_POINT('Ctrl Pts',(13.6151774048766,39.2257010213957,-0.684223919454799));
#18316=CARTESIAN_POINT('Ctrl Pts',(13.5895886129639,39.2685773960179,-1.09397285880287));
#18317=CARTESIAN_POINT('Ctrl Pts',(13.5755172628236,39.3074166220021,-1.36621764182792));
#18318=CARTESIAN_POINT('Ctrl Pts',(13.5422635943279,39.4545152562871,-2.17875768610036));
#18319=CARTESIAN_POINT('Ctrl Pts',(13.5321709123718,39.5931123698236,-2.71300426676916));
#18320=CARTESIAN_POINT('Ctrl Pts',(13.5352849214684,39.9497974103412,-3.75889728641716));
#18321=CARTESIAN_POINT('Ctrl Pts',(13.5486094073549,40.1677021769759,-4.26878718251941));
#18322=CARTESIAN_POINT('Ctrl Pts',(13.5961260568799,40.6780532465201,-5.2498408722557));
#18323=CARTESIAN_POINT('Ctrl Pts',(13.6304265742773,40.9694618609525,-5.71948809643038));
#18324=CARTESIAN_POINT('Ctrl Pts',(13.6746290992085,41.2947274963655,-6.16441400296901));
#18325=CARTESIAN_POINT('',(13.6749984935073,41.2946051706827,6.16441400296896));
#18326=CARTESIAN_POINT('Ctrl Pts',(13.6666806339867,39.1850971728872,-8.32667268468867E-16));
#18327=CARTESIAN_POINT('Ctrl Pts',(13.5758809146619,39.2167656094919,1.0986196092667));
#18328=CARTESIAN_POINT('Ctrl Pts',(13.5311071718145,39.4146279416703,2.18971594132769));
#18329=CARTESIAN_POINT('Ctrl Pts',(13.5358050982364,40.1287184680818,4.28292314717347));
#18330=CARTESIAN_POINT('Ctrl Pts',(13.5868958926851,40.6418470803382,5.27178170541197));
#18331=CARTESIAN_POINT('Ctrl Pts',(13.6749992876916,41.2946110548517,6.16442204944812));
#18332=CARTESIAN_POINT('Origin',(-1.73472347597681E-15,-1.73472347597681E-15,
6.16441400296896));
#18333=CARTESIAN_POINT('Origin',(0.,0.,-6.93889390390723E-15));
#18334=CARTESIAN_POINT('',(21.2337236115522,37.9654972519551,6.16441400296897));
#18335=CARTESIAN_POINT('',(20.664347998872,35.989369566325,0.));
#18336=CARTESIAN_POINT('Ctrl Pts',(21.2337236115522,37.9654972519551,6.16441400296898));
#18337=CARTESIAN_POINT('Ctrl Pts',(20.971955141007,37.3731094186789,5.27531660683071));
#18338=CARTESIAN_POINT('Ctrl Pts',(20.7843728952793,36.9038346756932,4.29109868658253));
#18339=CARTESIAN_POINT('Ctrl Pts',(20.588153446897,36.2327800916601,2.19783870908462));
#18340=CARTESIAN_POINT('Ctrl Pts',(20.5806969775164,36.0374002441774,1.10199792653056));
#18341=CARTESIAN_POINT('Ctrl Pts',(20.664347998872,35.9893695663249,-2.77555756156289E-16));
#18342=CARTESIAN_POINT('',(21.2335795549855,37.965577820996,-6.16441400296897));
#18343=CARTESIAN_POINT('Ctrl Pts',(21.2335819393416,37.9655832041028,-6.16442208610002));
#18344=CARTESIAN_POINT('Ctrl Pts',(20.9711781152475,37.3731598792073,-5.27485402176265));
#18345=CARTESIAN_POINT('Ctrl Pts',(20.7849917650648,36.9029619772348,-4.29007657026496));
#18346=CARTESIAN_POINT('Ctrl Pts',(20.6378259322843,36.4004654649649,-2.72168992255382));
#18347=CARTESIAN_POINT('Ctrl Pts',(20.6109772985515,36.2675856253627,-2.18495234743789));
#18348=CARTESIAN_POINT('Ctrl Pts',(20.6051018589552,36.1224047013253,-1.36923477588968));
#18349=CARTESIAN_POINT('Ctrl Pts',(20.6088638187637,36.0830978909367,-1.0961444642612));
#18350=CARTESIAN_POINT('Ctrl Pts',(20.6231784502659,36.0377407529866,-0.685318587194771));
#18351=CARTESIAN_POINT('Ctrl Pts',(20.6293878464561,36.0248966914307,-0.548301186444714));
#18352=CARTESIAN_POINT('Ctrl Pts',(20.644702429288,36.0037365731592,-0.274113036178763));
#18353=CARTESIAN_POINT('Ctrl Pts',(20.6538010798168,35.9954253880384,-0.137034229958601));
#18354=CARTESIAN_POINT('Ctrl Pts',(20.664347998872,35.9893695663249,2.42861286636753E-16));
#18355=CARTESIAN_POINT('',(19.4122935573318,38.9283040838408,-6.16441400296897));
#18356=CARTESIAN_POINT('Origin',(-5.20417042793042E-15,1.73472347597681E-15,
-6.16441400296897));
#18357=CARTESIAN_POINT('',(19.1041942977414,36.8412779397533,0.));
#18358=CARTESIAN_POINT('Ctrl Pts',(19.1041942977413,36.8412779397532,1.38777878078145E-15));
#18359=CARTESIAN_POINT('Ctrl Pts',(19.0176106207021,36.8861762571209,-1.09898083807772));
#18360=CARTESIAN_POINT('Ctrl Pts',(19.0022226489713,37.0881362268422,-2.19052946959247));
#18361=CARTESIAN_POINT('Ctrl Pts',(19.082964194596,37.6168941902153,-3.75889728453982));
#18362=CARTESIAN_POINT('Ctrl Pts',(19.1271641380397,37.8306847285466,-4.26878718105547));
#18363=CARTESIAN_POINT('Ctrl Pts',(19.246827666541,38.3290788360445,-5.24984087156839));
#18364=CARTESIAN_POINT('Ctrl Pts',(19.3222522781826,38.6126451860877,-5.71949644909548));
#18365=CARTESIAN_POINT('Ctrl Pts',(19.4122951858544,38.9283097929761,-6.16442204993663));
#18366=CARTESIAN_POINT('',(19.4126417829878,38.9281304329581,6.16441400296896));
#18367=CARTESIAN_POINT('Ctrl Pts',(19.1041942977413,36.8412779397532,-5.55111512312578E-16));
#18368=CARTESIAN_POINT('Ctrl Pts',(19.0188256770706,36.8855461847064,1.0986196092667));
#18369=CARTESIAN_POINT('Ctrl Pts',(19.0026664121714,37.0877665316094,2.18971594132768));
#18370=CARTESIAN_POINT('Ctrl Pts',(19.1089421982549,37.7939200614565,4.2829231471735));
#18371=CARTESIAN_POINT('Ctrl Pts',(19.2325374978635,38.2945498429304,5.2717730444335));
#18372=CARTESIAN_POINT('Ctrl Pts',(19.4126417829878,38.9281304329581,6.16441400296897));
#18373=CARTESIAN_POINT('Origin',(-1.73472347597681E-15,-1.73472347597681E-15,
6.16441400296896));
#18374=CARTESIAN_POINT('Origin',(0.,0.,-6.93889390390723E-15));
#18375=CARTESIAN_POINT('',(26.4206485230646,34.5571892899391,6.16441400296896));
#18376=CARTESIAN_POINT('',(25.5758360411619,32.6822063330432,0.));
#18377=CARTESIAN_POINT('Ctrl Pts',(26.4206485230647,34.5571892899391,6.16441400296897));
#18378=CARTESIAN_POINT('Ctrl Pts',(26.0772388994229,34.0080846482036,5.2753166068307));
#18379=CARTESIAN_POINT('Ctrl Pts',(25.8247812113316,33.5702821824269,4.2910986865825));
#18380=CARTESIAN_POINT('Ctrl Pts',(25.5350579694096,32.933982905541,2.19783870908455));
#18381=CARTESIAN_POINT('Ctrl Pts',(25.4998719447396,32.7416529094252,1.10199792653042));
#18382=CARTESIAN_POINT('Ctrl Pts',(25.5758360411619,32.6822063330431,1.11022302462516E-15));
#18383=CARTESIAN_POINT('',(26.4205173989462,34.5572895402979,-6.16441400296898));
#18384=CARTESIAN_POINT('Ctrl Pts',(26.420520525129,34.5572945292832,-6.16442208610004));
#18385=CARTESIAN_POINT('Ctrl Pts',(26.0764769637365,34.0082451771012,-5.27485402124597));
#18386=CARTESIAN_POINT('Ctrl Pts',(25.8252695836875,33.5693302919173,-4.29007656912465));
#18387=CARTESIAN_POINT('Ctrl Pts',(25.5354420784007,32.9335238913062,-2.19706468924219));
#18388=CARTESIAN_POINT('Ctrl Pts',(25.4988436963722,32.7424575769983,-1.10157448609152));
#18389=CARTESIAN_POINT('Ctrl Pts',(25.5758360411619,32.6822063330431,-1.66533453693773E-15));
#18390=CARTESIAN_POINT('',(24.7547796990912,35.7694126601132,-6.16441400296897));
#18391=CARTESIAN_POINT('Origin',(-5.20417042793042E-15,1.73472347597681E-15,
-6.16441400296897));
#18392=CARTESIAN_POINT('',(24.152801657541,33.7474765292383,0.));
#18393=CARTESIAN_POINT('Ctrl Pts',(24.152801657541,33.7474765292382,1.11022302462516E-15));
#18394=CARTESIAN_POINT('Ctrl Pts',(24.0734889742688,33.8042399884658,-1.09898083808803));
#18395=CARTESIAN_POINT('Ctrl Pts',(24.0869995303267,34.0063342336128,-2.19052946960189));
#18396=CARTESIAN_POINT('Ctrl Pts',(24.2421693474788,34.5182194833125,-3.75889728453595));
#18397=CARTESIAN_POINT('Ctrl Pts',(24.3163449651184,34.723543634418,-4.26878718104901));
#18398=CARTESIAN_POINT('Ctrl Pts',(24.5057193682513,35.1998349128155,-5.24984087156284));
#18399=CARTESIAN_POINT('Ctrl Pts',(24.6207297677859,35.4697758585235,-5.71948809610186));
#18400=CARTESIAN_POINT('Ctrl Pts',(24.7547796990912,35.7694126601132,-6.16441400296901));
#18401=CARTESIAN_POINT('',(24.7550996672029,35.7691912190764,6.16441400296897));
#18402=CARTESIAN_POINT('Ctrl Pts',(24.152801657541,33.7474765292382,8.32667268468867E-16));
#18403=CARTESIAN_POINT('Ctrl Pts',(24.0746019944585,33.8034434087317,1.09861960926675));
#18404=CARTESIAN_POINT('Ctrl Pts',(24.0873861635413,34.0059051472516,2.18971594132777));
#18405=CARTESIAN_POINT('Ctrl Pts',(24.2930763407557,34.6897464310454,4.28292314717347));
#18406=CARTESIAN_POINT('Ctrl Pts',(24.4866606648092,35.1676910781172,5.27177304443343));
#18407=CARTESIAN_POINT('Ctrl Pts',(24.7550996672028,35.7691912190764,6.16441400296897));
#18408=CARTESIAN_POINT('Origin',(-1.73472347597681E-15,-1.73472347597681E-15,
6.16441400296896));
#18409=CARTESIAN_POINT('Origin',(0.,0.,-6.93889390390723E-15));
#18410=CARTESIAN_POINT('',(31.0697252215062,30.4453966086846,6.16441400296896));
#18411=CARTESIAN_POINT('',(29.9666738162744,28.7097276265209,0.));
#18412=CARTESIAN_POINT('Ctrl Pts',(31.0697252215062,30.4453966086846,6.16441400296899));
#18413=CARTESIAN_POINT('Ctrl Pts',(30.6516652743936,29.9507533455085,5.27531660683076));
#18414=CARTESIAN_POINT('Ctrl Pts',(30.3394714544406,29.5533355526259,4.29109868658263));
#18415=CARTESIAN_POINT('Ctrl Pts',(29.9621423486914,28.9647448012291,2.19783870908459));
#18416=CARTESIAN_POINT('Ctrl Pts',(29.8999430547262,28.7793799405671,1.1019979265305));
#18417=CARTESIAN_POINT('Ctrl Pts',(29.9666738162744,28.7097276265209,8.32667268468867E-16));
#18418=CARTESIAN_POINT('',(31.0696096991581,30.4455144995447,-6.16441400296899));
#18419=CARTESIAN_POINT('Ctrl Pts',(31.0696096991581,30.4455144995446,-6.16441400296901));
#18420=CARTESIAN_POINT('Ctrl Pts',(30.6509301353917,29.9510161819023,-5.27484593811529));
#18421=CARTESIAN_POINT('Ctrl Pts',(30.3398193877248,29.5523238483581,-4.29007656912537));
#18422=CARTESIAN_POINT('Ctrl Pts',(29.9624572234713,28.9642357946874,-2.19706468924242));
#18423=CARTESIAN_POINT('Ctrl Pts',(29.8990397885865,28.7803227527781,-1.10157448608938));
#18424=CARTESIAN_POINT('Ctrl Pts',(29.9666738162744,28.7097276265209,-1.94289029309402E-15));
#18425=CARTESIAN_POINT('',(29.5933299130458,31.8823591451078,-6.16441400296898));
#18426=CARTESIAN_POINT('Origin',(-5.20417042793042E-15,1.73472347597681E-15,
-6.16441400296897));
#18427=CARTESIAN_POINT('',(28.7097276265215,29.9666738162739,0.));
#18428=CARTESIAN_POINT('Ctrl Pts',(28.7097276265214,29.9666738162739,1.38777878078145E-15));
#18429=CARTESIAN_POINT('Ctrl Pts',(28.7009474204864,29.9750857383081,-0.137010845867973));
#18430=CARTESIAN_POINT('Ctrl Pts',(28.6939122150404,29.9855286660437,-0.273849719843528));
#18431=CARTESIAN_POINT('Ctrl Pts',(28.6833082731284,30.0104891974361,-0.547496131369053));
#18432=CARTESIAN_POINT('Ctrl Pts',(28.6797460897164,30.0250035906012,-0.684223919461066));
#18433=CARTESIAN_POINT('Ctrl Pts',(28.6742811955932,30.0746352811264,-1.09397285881146));
#18434=CARTESIAN_POINT('Ctrl Pts',(28.6776158428565,30.1158101338568,-1.36621764183717));
#18435=CARTESIAN_POINT('Ctrl Pts',(28.708474223108,30.2634298312027,-2.17875768610757));
#18436=CARTESIAN_POINT('Ctrl Pts',(28.7568689184051,30.3936948517435,-2.71300426677357));
#18437=CARTESIAN_POINT('Ctrl Pts',(28.907873841452,30.7168533707375,-3.75889728641903));
#18438=CARTESIAN_POINT('Ctrl Pts',(29.010515131592,30.9095313269397,-4.26878718252163));
#18439=CARTESIAN_POINT('Ctrl Pts',(29.2657452924933,31.3540238590871,-5.24984087225568));
#18440=CARTESIAN_POINT('Ctrl Pts',(29.4180016539271,31.6048495086171,-5.71948809643018));
#18441=CARTESIAN_POINT('Ctrl Pts',(29.5933299130457,31.8823591451077,-6.16441400296901));
#18442=CARTESIAN_POINT('',(29.593615110006,31.882094421804,6.16441400296896));
#18443=CARTESIAN_POINT('Ctrl Pts',(28.7097276265214,29.9666738162739,-8.32667268468867E-16));
#18444=CARTESIAN_POINT('Ctrl Pts',(28.6402888406582,30.0332000060362,1.09861960926672));
#18445=CARTESIAN_POINT('Ctrl Pts',(28.6817561949071,30.2317815990283,2.18971594132772));
#18446=CARTESIAN_POINT('Ctrl Pts',(28.9826735044059,30.8793896002661,4.28292314717346));
#18447=CARTESIAN_POINT('Ctrl Pts',(29.2423060343177,31.3249195382,5.27177304443341));
#18448=CARTESIAN_POINT('Ctrl Pts',(29.593615110006,31.882094421804,6.16441400296897));
#18449=CARTESIAN_POINT('Origin',(-1.73472347597681E-15,-1.73472347597681E-15,
6.16441400296896));
#18450=CARTESIAN_POINT('Origin',(0.,0.,-6.93889390390723E-15));
#18451=CARTESIAN_POINT('',(35.0863119121266,25.713823449751,6.16441400296896));
#18452=CARTESIAN_POINT('',(33.7474765292387,24.1528016575404,0.));
#18453=CARTESIAN_POINT('Ctrl Pts',(35.0863119121266,25.713823449751,6.16441400296898));
#18454=CARTESIAN_POINT('Ctrl Pts',(34.6021121364811,25.2837110755392,5.2753166068307));
#18455=CARTESIAN_POINT('Ctrl Pts',(34.2365375505478,24.9347682357555,4.2910986865825));
#18456=CARTESIAN_POINT('Ctrl Pts',(33.7792839134374,24.4058680201907,2.19783870908459));
#18457=CARTESIAN_POINT('Ctrl Pts',(33.6913375484341,24.2312417889975,1.10199792653051));
#18458=CARTESIAN_POINT('Ctrl Pts',(33.7474765292387,24.1528016575404,1.38777878078145E-15));
#18459=CARTESIAN_POINT('',(35.0862143432449,25.7139565812008,-6.16441400296898));
#18460=CARTESIAN_POINT('Ctrl Pts',(35.0862143432449,25.7139565812008,-6.16441400296901));
#18461=CARTESIAN_POINT('Ctrl Pts',(34.601421885651,25.2840758578288,-5.27484593811562));
#18462=CARTESIAN_POINT('Ctrl Pts',(34.2367379618438,24.933717313109,-4.29007656912498));
#18463=CARTESIAN_POINT('Ctrl Pts',(33.7795231440548,24.4053193832426,-2.19706468921364));
#18464=CARTESIAN_POINT('Ctrl Pts',(33.6905776524145,24.232303552906,-1.10157448593714));
#18465=CARTESIAN_POINT('Ctrl Pts',(33.7474765292387,24.1528016575404,5.55111512312578E-16));
#18466=CARTESIAN_POINT('',(33.8294452700945,27.346272739035,-6.16441400296899));
#18467=CARTESIAN_POINT('Origin',(-5.20417042793042E-15,1.73472347597681E-15,
-6.16441400296897));
#18468=CARTESIAN_POINT('',(32.6822063330436,25.5758360411613,0.));
#18469=CARTESIAN_POINT('Ctrl Pts',(32.6822063330436,25.5758360411613,3.12250225675825E-15));
#18470=CARTESIAN_POINT('Ctrl Pts',(32.6747126381706,25.5854118955592,-0.13701084587003));
#18471=CARTESIAN_POINT('Ctrl Pts',(32.6692352245446,25.5967497434724,-0.273849719845774));
#18472=CARTESIAN_POINT('Ctrl Pts',(32.6622914694609,25.6229653109225,-0.547496131372112));
#18473=CARTESIAN_POINT('Ctrl Pts',(32.6608311574562,25.637838920049,-0.684223919464382));
#18474=CARTESIAN_POINT('Ctrl Pts',(32.6624852140865,25.6877431670502,-1.09397285881505));
#18475=CARTESIAN_POINT('Ctrl Pts',(32.6716457119561,25.7280243493632,-1.36621764184054));
#18476=CARTESIAN_POINT('Ctrl Pts',(32.7231984717437,25.8697498856463,-2.17875768610944));
#18477=CARTESIAN_POINT('Ctrl Pts',(32.7896392241513,25.991801712872,-2.7130042667745));
#18478=CARTESIAN_POINT('Ctrl Pts',(32.9850973871782,26.290180702898,-3.75889728641806));
#18479=CARTESIAN_POINT('Ctrl Pts',(33.1141148691575,26.4662900967167,-4.26878718251969));
#18480=CARTESIAN_POINT('Ctrl Pts',(33.4300050378579,26.8699352967219,-5.24984087225438));
#18481=CARTESIAN_POINT('Ctrl Pts',(33.6164113967186,27.0965438053519,-5.7194964494206));
#18482=CARTESIAN_POINT('Ctrl Pts',(33.8294491231113,27.3462772557344,-6.16442204993664));
#18483=CARTESIAN_POINT('',(33.8296898901082,27.3459701224717,6.16441400296896));
#18484=CARTESIAN_POINT('Ctrl Pts',(32.6822063330436,25.5758360411613,-2.22044604925031E-15));
#18485=CARTESIAN_POINT('Ctrl Pts',(32.622941997835,25.6515672598147,1.0986196092667));
#18486=CARTESIAN_POINT('Ctrl Pts',(32.6922483814993,25.8422261587076,2.18971594132768));
#18487=CARTESIAN_POINT('Ctrl Pts',(33.082267014635,26.4404174460315,4.2829231471735));
#18488=CARTESIAN_POINT('Ctrl Pts',(33.4026623808145,26.8444629700935,5.27177304443349));
#18489=CARTESIAN_POINT('Ctrl Pts',(33.8296898901081,27.3459701224717,6.16441400296898));
#18490=CARTESIAN_POINT('Origin',(-1.73472347597681E-15,-1.73472347597681E-15,
6.16441400296896));
#18491=CARTESIAN_POINT('Origin',(0.,0.,-6.93889390390723E-15));
#18492=CARTESIAN_POINT('',(38.3886424727845,20.4587909979239,6.16441400296896));
#18493=CARTESIAN_POINT('',(36.8412779397543,19.1041942977414,6.93889390390723E-15));
#18494=CARTESIAN_POINT('Ctrl Pts',(38.3886424727844,20.4587909979239,6.16441400296899));
#18495=CARTESIAN_POINT('Ctrl Pts',(37.8481597797213,20.1019653602737,5.27531660683076));
#18496=CARTESIAN_POINT('Ctrl Pts',(37.4366464721474,19.808600943539,4.29109868658265));
#18497=CARTESIAN_POINT('Ctrl Pts',(36.9087766691159,19.3501581469721,2.19783870908195));
#18498=CARTESIAN_POINT('Ctrl Pts',(36.7968735674506,19.1898254317345,1.10199792652477));
#18499=CARTESIAN_POINT('Ctrl Pts',(36.8412779397536,19.1041942977407,3.33066907387547E-14));
#18500=CARTESIAN_POINT('',(38.3885648435948,20.4589366597857,-6.16441400296898));
#18501=CARTESIAN_POINT('Ctrl Pts',(38.3885648435948,20.4589366597857,-6.16441400296902));
#18502=CARTESIAN_POINT('Ctrl Pts',(37.8475284685813,20.1024246625415,-5.27484593811522));
#18503=CARTESIAN_POINT('Ctrl Pts',(37.4366952816589,19.8075321962687,-4.29007656912551));
#18504=CARTESIAN_POINT('Ctrl Pts',(36.9089353855233,19.3495810482744,-2.19706468916407));
#18505=CARTESIAN_POINT('Ctrl Pts',(36.7962725108494,19.19098453287,-1.10157448567205));
#18506=CARTESIAN_POINT('Ctrl Pts',(36.8412779397536,19.1041942977407,-2.02615701994091E-14));
#18507=CARTESIAN_POINT('',(37.3768906775087,22.2534950801344,-6.16441400296898));
#18508=CARTESIAN_POINT('Origin',(-5.20417042793042E-15,1.73472347597681E-15,
-6.16441400296897));
#18509=CARTESIAN_POINT('',(35.9893695663253,20.6643479988714,0.));
#18510=CARTESIAN_POINT('Ctrl Pts',(35.9893695663253,20.6643479988713,1.94289029309402E-15));
#18511=CARTESIAN_POINT('Ctrl Pts',(35.9833149326307,20.6748928488533,-0.137010845865106));
#18512=CARTESIAN_POINT('Ctrl Pts',(35.9795068151691,20.6868948110578,-0.273849719841543));
#18513=CARTESIAN_POINT('Ctrl Pts',(35.9763646017412,20.7138317412138,-0.547496131366511));
#18514=CARTESIAN_POINT('Ctrl Pts',(35.9770358888841,20.7287617825126,-0.684223919458269));
#18515=CARTESIAN_POINT('Ctrl Pts',(35.985775224443,20.7779226794343,-1.09397285880729));
#18516=CARTESIAN_POINT('Ctrl Pts',(36.0005750915987,20.8164901826193,-1.36621764183265));
#18517=CARTESIAN_POINT('Ctrl Pts',(36.0717727653998,20.9494364346224,-2.17875768610445));
#18518=CARTESIAN_POINT('Ctrl Pts',(36.1549070328013,21.0607904452962,-2.71300426677191));
#18519=CARTESIAN_POINT('Ctrl Pts',(36.390839471268,21.3283157705684,-3.75889728641864));
#18520=CARTESIAN_POINT('Ctrl Pts',(36.5436067212089,21.4842715226041,-4.2687871825207));
#18521=CARTESIAN_POINT('Ctrl Pts',(36.9137262848261,21.8388523382117,-5.24984087225524));
#18522=CARTESIAN_POINT('Ctrl Pts',(37.1304809453721,22.0366222125383,-5.71948809642998));
#18523=CARTESIAN_POINT('Ctrl Pts',(37.3768906775087,22.2534950801344,-6.16441400296901));
#18524=CARTESIAN_POINT('',(37.3770897408174,22.2531607307117,6.16441400296896));
#18525=CARTESIAN_POINT('Ctrl Pts',(35.9893695663253,20.6643479988713,2.77555756156289E-16));
#18526=CARTESIAN_POINT('Ctrl Pts',(35.9414861327319,20.7477425771949,1.09861960926664));
#18527=CARTESIAN_POINT('Ctrl Pts',(36.0372206677033,20.9265975166219,2.18971594132757));
#18528=CARTESIAN_POINT('Ctrl Pts',(36.5084009698262,21.4631946404632,4.28292314717355));
#18529=CARTESIAN_POINT('Ctrl Pts',(36.8830368465619,21.8175305489545,5.27177304443358));
#18530=CARTESIAN_POINT('Ctrl Pts',(37.3770897408173,22.2531607307117,6.16441400296898));
#18531=CARTESIAN_POINT('Origin',(-1.73472347597681E-15,-1.73472347597681E-15,
6.16441400296896));
#18532=CARTESIAN_POINT('Origin',(0.,0.,-6.93889390390723E-15));
#18533=CARTESIAN_POINT('',(40.9094909763996,14.7872765596604,6.16441400296896));
#18534=CARTESIAN_POINT('',(39.1850971728875,13.666680633986,0.));
#18535=CARTESIAN_POINT('Ctrl Pts',(40.9094909763996,14.7872765596603,6.16441400296898));
#18536=CARTESIAN_POINT('Ctrl Pts',(40.3237280349262,14.5110015995542,5.27531660683077));
#18537=CARTESIAN_POINT('Ctrl Pts',(39.8746532299475,14.2791876593999,4.29109868658268));
#18538=CARTESIAN_POINT('Ctrl Pts',(39.2869131679352,13.9005348551303,2.19783870908451));
#18539=CARTESIAN_POINT('Ctrl Pts',(39.153331354054,13.757759567569,1.10199792653032));
#18540=CARTESIAN_POINT('Ctrl Pts',(39.1850971728875,13.666680633986,1.66533453693773E-15));
#18541=CARTESIAN_POINT('',(40.9094348672085,14.7874317866772,-6.16441400296898));
#18542=CARTESIAN_POINT('Ctrl Pts',(40.9094348672084,14.7874317866772,-6.164414002969));
#18543=CARTESIAN_POINT('Ctrl Pts',(40.3231685151537,14.5115460717244,-5.27484593811583));
#18544=CARTESIAN_POINT('Ctrl Pts',(39.8745494440533,14.2781228441186,-4.29007656912527));
#18545=CARTESIAN_POINT('Ctrl Pts',(39.2869881391103,13.8999410427645,-2.1970646891068));
#18546=CARTESIAN_POINT('Ctrl Pts',(39.1529013726389,13.7589924099824,-1.10157448537221));
#18547=CARTESIAN_POINT('Ctrl Pts',(39.1850971728875,13.666680633986,-8.32667268468867E-16));
#18548=CARTESIAN_POINT('',(40.1634503767828,16.7077004351798,-6.16441400296898));
#18549=CARTESIAN_POINT('Origin',(-5.20417042793042E-15,1.73472347597681E-15,
-6.16441400296897));
#18550=CARTESIAN_POINT('',(38.5638930200082,15.3321934223831,0.));
#18551=CARTESIAN_POINT('Ctrl Pts',(38.5638930200081,15.3321934223831,1.38777878078145E-16));
#18552=CARTESIAN_POINT('Ctrl Pts',(38.5594007023748,15.3434926052104,-0.137010845860786));
#18553=CARTESIAN_POINT('Ctrl Pts',(38.5573394033684,15.3559143563653,-0.273849719841182));
#18554=CARTESIAN_POINT('Ctrl Pts',(38.5580626980017,15.3830242910068,-0.54749613136722));
#18555=CARTESIAN_POINT('Ctrl Pts',(38.5608519188225,15.3977068318908,-0.684223919458968));
#18556=CARTESIAN_POINT('Ctrl Pts',(38.5764986256418,15.4451236046381,-1.09397285880846));
#18557=CARTESIAN_POINT('Ctrl Pts',(38.5966365794681,15.4811923055493,-1.36621764183395));
#18558=CARTESIAN_POINT('Ctrl Pts',(38.6860297879615,15.602652870967,-2.17875768610512));
#18559=CARTESIAN_POINT('Ctrl Pts',(38.7841651964102,15.7010422185523,-2.7130042667723));
#18560=CARTESIAN_POINT('Ctrl Pts',(39.0557690062388,15.9322678349323,-3.75889728641943));
#18561=CARTESIAN_POINT('Ctrl Pts',(39.2291761234756,16.0648951358156,-4.26878718252243));
#18562=CARTESIAN_POINT('Ctrl Pts',(39.6459905150316,16.3631933241455,-5.24984087225649));
#18563=CARTESIAN_POINT('Ctrl Pts',(39.8886845133482,16.5281027818499,-5.71948809643058));
#18564=CARTESIAN_POINT('Ctrl Pts',(40.1634503767828,16.7077004351798,-6.164414002969));
#18565=CARTESIAN_POINT('',(40.1635998310295,16.7073411592907,6.16441400296896));
#18566=CARTESIAN_POINT('Ctrl Pts',(38.5638930200081,15.3321934223831,-8.32667268468867E-16));
#18567=CARTESIAN_POINT('Ctrl Pts',(38.5283652566535,15.4215536872522,1.0986196092665));
#18568=CARTESIAN_POINT('Ctrl Pts',(38.6485790638755,15.5849636964217,2.18971594132732));
#18569=CARTESIAN_POINT('Ctrl Pts',(39.1913291628061,16.0490430867574,4.28292314717371));
#18570=CARTESIAN_POINT('Ctrl Pts',(39.6125790440085,16.3464561224015,5.27177304443379));
#18571=CARTESIAN_POINT('Ctrl Pts',(40.1635998310295,16.7073411592907,6.16441400296898));
#18572=CARTESIAN_POINT('Origin',(-1.73472347597681E-15,-1.73472347597681E-15,
6.16441400296896));
#18573=CARTESIAN_POINT('Origin',(0.,0.,-6.93889390390723E-15));
#18574=CARTESIAN_POINT('',(42.5975402169653,8.81473581362642,6.16441400296896));
#18575=CARTESIAN_POINT('',(40.7312208280703,7.9509527639758,0.));
#18576=CARTESIAN_POINT('Ctrl Pts',(42.5975402169653,8.8147358136264,6.16441400296897));
#18577=CARTESIAN_POINT('Ctrl Pts',(41.9783611257759,8.62461716345458,5.27522994637944));
#18578=CARTESIAN_POINT('Ctrl Pts',(41.5008344149426,8.45905891928459,4.29090746118671));
#18579=CARTESIAN_POINT('Ctrl Pts',(40.865251830097,8.16791310841239,2.19762693960535));
#18580=CARTESIAN_POINT('Ctrl Pts',(40.7127420143401,8.04561621690129,1.10189111929206));
#18581=CARTESIAN_POINT('Ctrl Pts',(40.7312208280703,7.95095276397578,3.05311331771918E-15));
#18582=CARTESIAN_POINT('',(42.5975067699923,8.81489744582799,-6.16441400296898));
#18583=CARTESIAN_POINT('Ctrl Pts',(42.5975067699923,8.81489744582797,-6.164414002969));
#18584=CARTESIAN_POINT('Ctrl Pts',(41.9779451331701,8.62525425073588,-5.27484593811595));
#18585=CARTESIAN_POINT('Ctrl Pts',(41.5006727684721,8.45805208556826,-4.29007656912516));
#18586=CARTESIAN_POINT('Ctrl Pts',(40.8652711085094,8.16733832174138,-2.19706468906351));
#18587=CARTESIAN_POINT('Ctrl Pts',(40.7124900701213,8.04690687928061,-1.10157448514352));
#18588=CARTESIAN_POINT('Ctrl Pts',(40.7312208280703,7.95095276397578,-1.38777878078145E-15));
#18589=CARTESIAN_POINT('',(42.1323980482129,10.8217851903902,-6.16441400296898));
#18590=CARTESIAN_POINT('Origin',(-5.20417042793042E-15,1.73472347597681E-15,
-6.16441400296897));
#18591=CARTESIAN_POINT('',(40.3533668208877,9.68791960220985,0.));
#18592=CARTESIAN_POINT('Ctrl Pts',(40.3533668208877,9.68791960220986,1.17961196366423E-15));
#18593=CARTESIAN_POINT('Ctrl Pts',(40.3505282699472,9.69974309910533,-0.137010845854389));
#18594=CARTESIAN_POINT('Ctrl Pts',(40.3502557514989,9.71233176817958,-0.273849719838591));
#18595=CARTESIAN_POINT('Ctrl Pts',(40.3548298299996,9.73906282721793,-0.547496131365122));
#18596=CARTESIAN_POINT('Ctrl Pts',(40.3596802040054,9.75319897349669,-0.684223919456776));
#18597=CARTESIAN_POINT('Ctrl Pts',(40.3819157602544,9.79790635331761,-1.09397285880488));
#18598=CARTESIAN_POINT('Ctrl Pts',(40.4069818500837,9.83074199721934,-1.36621764183001));
#18599=CARTESIAN_POINT('Ctrl Pts',(40.5127508053323,9.9382442892057,-2.17875768610251));
#18600=CARTESIAN_POINT('Ctrl Pts',(40.623889600912,10.0216660503167,-2.71300426677077));
#18601=CARTESIAN_POINT('Ctrl Pts',(40.9256357117777,10.2118848710475,-3.75889728641811));
#18602=CARTESIAN_POINT('Ctrl Pts',(41.1161526274704,10.3184838113887,-4.26878718252017));
#18603=CARTESIAN_POINT('Ctrl Pts',(41.5711767079479,10.5544268815438,-5.24984087225546));
#18604=CARTESIAN_POINT('Ctrl Pts',(41.8348694941005,10.683118841629,-5.71948809643011));
#18605=CARTESIAN_POINT('Ctrl Pts',(42.1323980482129,10.8217851903902,-6.164414002969));
#18606=CARTESIAN_POINT('',(42.1324948509395,10.8214083018598,6.16441400296896));
#18607=CARTESIAN_POINT('Ctrl Pts',(40.3533668208877,9.68791960220987,-5.55111512312578E-16));
#18608=CARTESIAN_POINT('Ctrl Pts',(40.3309179705801,9.78142643632542,1.09861960926657));
#18609=CARTESIAN_POINT('Ctrl Pts',(40.4731638436058,9.92606495868641,2.18971594132745));
#18610=CARTESIAN_POINT('Ctrl Pts',(41.0764349124919,10.3081792974235,4.2829231471736));
#18611=CARTESIAN_POINT('Ctrl Pts',(41.5357233653638,10.542614988483,5.27177304443365));
#18612=CARTESIAN_POINT('Ctrl Pts',(42.1324948509395,10.8214083018599,6.16441400296898));
#18613=CARTESIAN_POINT('Origin',(-1.73472347597681E-15,-1.73472347597681E-15,
6.16441400296896));
#18614=CARTESIAN_POINT('Origin',(0.,0.,-6.93889390390723E-15));
#18615=CARTESIAN_POINT('',(43.4184263798756,2.66275246602602,6.16441400296896));
#18616=CARTESIAN_POINT('',(41.448174286335,2.07336642434544,0.));
#18617=CARTESIAN_POINT('Ctrl Pts',(43.4184263798756,2.66275246602601,6.16441400296898));
#18618=CARTESIAN_POINT('Ctrl Pts',(42.7784929341,2.5626873218093,5.27522994637943));
#18619=CARTESIAN_POINT('Ctrl Pts',(42.2822653619025,2.46677335847309,4.29090746118668));
#18620=CARTESIAN_POINT('Ctrl Pts',(41.611717722348,2.26904382492961,2.19762693960537));
#18621=CARTESIAN_POINT('Ctrl Pts',(41.4433555742777,2.16969614920107,1.10189111929209));
#18622=CARTESIAN_POINT('Ctrl Pts',(41.4481742863349,2.07336642434542,1.11022302462516E-15));
#18623=CARTESIAN_POINT('',(43.4184162760054,2.6629172130419,-6.16441400296898));
#18624=CARTESIAN_POINT('Ctrl Pts',(43.4184162760054,2.66291721304189,-6.16441400296901));
#18625=CARTESIAN_POINT('Ctrl Pts',(42.7781718430444,2.56337712643548,-5.27484593863236));
#18626=CARTESIAN_POINT('Ctrl Pts',(42.2819620739562,2.46579977767809,-4.29007657026531));
#18627=CARTESIAN_POINT('Ctrl Pts',(41.7796712516364,2.31793342925177,-2.72168992254993));
#18628=CARTESIAN_POINT('Ctrl Pts',(41.6533701498395,2.26867967212385,-2.18495234742919));
#18629=CARTESIAN_POINT('Ctrl Pts',(41.5280596821275,2.19513167299008,-1.36923477587661));
#18630=CARTESIAN_POINT('Ctrl Pts',(41.4970265580502,2.17071604491098,-1.09614446424856));
#18631=CARTESIAN_POINT('Ctrl Pts',(41.4666087795881,2.1341518904505,-0.685318587183261));
#18632=CARTESIAN_POINT('Ctrl Pts',(41.4591607204606,2.12198419003006,-0.548301186434216));
#18633=CARTESIAN_POINT('Ctrl Pts',(41.4496393847912,2.09766071948028,-0.274113036173078));
#18634=CARTESIAN_POINT('Ctrl Pts',(41.447566672806,2.08551308166182,-0.137034229955334));
#18635=CARTESIAN_POINT('Ctrl Pts',(41.4481742863349,2.07336642434541,-2.0122792321331E-15));
#18636=CARTESIAN_POINT('',(43.2436515951818,4.71556960658337,-6.16441400296898));
#18637=CARTESIAN_POINT('Origin',(-5.20417042793042E-15,1.73472347597681E-15,
-6.16441400296897));
#18638=CARTESIAN_POINT('',(41.3213624427944,3.84642767658874,0.));
#18639=CARTESIAN_POINT('Ctrl Pts',(41.3213624427943,3.84642767658874,1.73472347597681E-16));
#18640=CARTESIAN_POINT('Ctrl Pts',(41.3202354432581,3.85853479525182,-0.137010845851213));
#18641=CARTESIAN_POINT('Ctrl Pts',(41.321757253058,3.87103411324551,-0.273849719837603));
#18642=CARTESIAN_POINT('Ctrl Pts',(41.3300890003786,3.89684212940388,-0.547496131362626));
#18643=CARTESIAN_POINT('Ctrl Pts',(41.336901787942,3.91014410990395,-0.684223919453106));
#18644=CARTESIAN_POINT('Ctrl Pts',(41.3652735418183,3.95123198346985,-1.09397285880268));
#18645=CARTESIAN_POINT('Ctrl Pts',(41.3947574943469,3.98016613134156,-1.36621764182791));
#18646=CARTESIAN_POINT('Ctrl Pts',(41.5147490454351,4.0715217132403,-2.17875768610036));
#18647=CARTESIAN_POINT('Ctrl Pts',(41.6366287627659,4.13827766138837,-2.71300426676958));
#18648=CARTESIAN_POINT('Ctrl Pts',(41.9623744940145,4.2836173798294,-3.75889728641934));
#18649=CARTESIAN_POINT('Ctrl Pts',(42.1661228331635,4.36201791261592,-4.26878718252248));
#18650=CARTESIAN_POINT('Ctrl Pts',(42.6500936244634,4.53080274409635,-5.24984087225778));
#18651=CARTESIAN_POINT('Ctrl Pts',(42.9294171737525,4.6206574093722,-5.71948809643132));
#18652=CARTESIAN_POINT('Ctrl Pts',(43.2436515951818,4.71556960658337,-6.16441400296901));
#18653=CARTESIAN_POINT('',(43.2436937757662,4.71518277776774,6.16441400296896));
#18654=CARTESIAN_POINT('Ctrl Pts',(41.3213624427943,3.84642767658874,-8.32667268468867E-16));
#18655=CARTESIAN_POINT('Ctrl Pts',(41.3124474863202,3.94219917643307,1.09886774242324));
#18656=CARTESIAN_POINT('Ctrl Pts',(41.4739046363274,4.06515557324188,2.190207356141));
#18657=CARTESIAN_POINT('Ctrl Pts',(42.1255613966704,4.35754593773624,4.28336653879353));
#18658=CARTESIAN_POINT('Ctrl Pts',(42.613461821837,4.52419955110993,5.27197367572233));
#18659=CARTESIAN_POINT('Ctrl Pts',(43.2436937757662,4.71518277776774,6.16441400296897));
#18660=CARTESIAN_POINT('Origin',(-1.73472347597681E-15,-1.73472347597681E-15,
6.16441400296896));
#18661=CARTESIAN_POINT('Origin',(0.,0.,-6.93889390390723E-15));
#18662=CARTESIAN_POINT('',(43.3554385900938,-3.54343684303869,6.16441400296896));
#18663=CARTESIAN_POINT('',(41.3213624427943,-3.84642767658963,0.));
#18664=CARTESIAN_POINT('Ctrl Pts',(43.3554444774928,-3.5434367705481,6.16442208586934));
#18665=CARTESIAN_POINT('Ctrl Pts',(42.7077838766714,-3.55141137103749,5.27523802927978));
#18666=CARTESIAN_POINT('Ctrl Pts',(42.2029513180785,-3.57572859433001,4.29090746118662));
#18667=CARTESIAN_POINT('Ctrl Pts',(41.5110890400568,-3.67601664744674,2.19762693960542));
#18668=CARTESIAN_POINT('Ctrl Pts',(41.3303019274915,-3.75039267520991,1.10189111929219));
#18669=CARTESIAN_POINT('Ctrl Pts',(41.3213624427942,-3.84642767658964,5.55111512312578E-16));
#18670=CARTESIAN_POINT('',(43.3554520350114,-3.54327233497894,-6.16441400296897));
#18671=CARTESIAN_POINT('Ctrl Pts',(43.3554520350114,-3.54327233497896,-6.16441400296899));
#18672=CARTESIAN_POINT('Ctrl Pts',(42.7075583358946,-3.55068296409579,-5.27484593863224));
#18673=CARTESIAN_POINT('Ctrl Pts',(42.2025125621728,-3.57664910310152,-4.29007657026532));
#18674=CARTESIAN_POINT('Ctrl Pts',(41.6842907607187,-3.6515269481625,-2.7216899225514));
#18675=CARTESIAN_POINT('Ctrl Pts',(41.5522656815471,-3.68230485218473,-2.18495234743192));
#18676=CARTESIAN_POINT('Ctrl Pts',(41.4177637221115,-3.73727069978806,-1.36923477588026));
#18677=CARTESIAN_POINT('Ctrl Pts',(41.3835717643297,-3.75702133794349,-1.09614446425197));
#18678=CARTESIAN_POINT('Ctrl Pts',(41.3482599732647,-3.78888442081007,-0.68531858718678));
#18679=CARTESIAN_POINT('Ctrl Pts',(41.3391560803224,-3.79986830225437,-0.548301186437842));
#18680=CARTESIAN_POINT('Ctrl Pts',(41.3262700673438,-3.82258916759967,-0.274113036173981));
#18681=CARTESIAN_POINT('Ctrl Pts',(41.3224896634664,-3.8343181823096,-0.137034229955792));
#18682=CARTESIAN_POINT('Ctrl Pts',(41.3213624427942,-3.84642767658964,-4.85722573273506E-16));
#18683=CARTESIAN_POINT('',(43.4745891000668,-1.48664137583804,-6.16441400296898));
#18684=CARTESIAN_POINT('Origin',(-5.20417042793042E-15,1.73472347597681E-15,
-6.16441400296897));
#18685=CARTESIAN_POINT('',(41.4481742863349,-2.07336642434629,1.04083408558608E-14));
#18686=CARTESIAN_POINT('Ctrl Pts',(41.4481742863349,-2.07336642434628,1.11022302462516E-14));
#18687=CARTESIAN_POINT('Ctrl Pts',(41.4530470730269,-1.97595570634813,-1.09898083808598));
#18688=CARTESIAN_POINT('Ctrl Pts',(41.6303639287926,-1.87806111146117,-2.19052946960028));
#18689=CARTESIAN_POINT('Ctrl Pts',(42.1448803402979,-1.73185220848821,-3.75889728453942));
#18690=CARTESIAN_POINT('Ctrl Pts',(42.3577123743482,-1.68324609198078,-4.26878718105493));
#18691=CARTESIAN_POINT('Ctrl Pts',(42.8607776270729,-1.58505547153932,-5.24984087156854));
#18692=CARTESIAN_POINT('Ctrl Pts',(43.1500457177245,-1.53586728290387,-5.71948809610463));
#18693=CARTESIAN_POINT('Ctrl Pts',(43.4745891000668,-1.48664137583802,-6.164414002969));
#18694=CARTESIAN_POINT('',(43.4745757998335,-1.48703027021543,6.16441400296897));
#18695=CARTESIAN_POINT('Ctrl Pts',(41.4481742863349,-2.07336642434627,7.7715611723761E-15));
#18696=CARTESIAN_POINT('Ctrl Pts',(41.4529797767749,-1.97730100969043,1.09886774242324));
#18697=CARTESIAN_POINT('Ctrl Pts',(41.6302920455235,-1.87857387990399,2.19020735614099));
#18698=CARTESIAN_POINT('Ctrl Pts',(42.3169273670934,-1.68190005418599,4.2833665387936));
#18699=CARTESIAN_POINT('Ctrl Pts',(42.8235789514612,-1.58637820440283,5.27197367572244));
#18700=CARTESIAN_POINT('Ctrl Pts',(43.4745757998334,-1.48703027021542,6.16441400296898));
#18701=CARTESIAN_POINT('Origin',(-1.73472347597681E-15,-1.73472347597681E-15,
6.16441400296896));
#18702=CARTESIAN_POINT('Origin',(0.,0.,-6.93889390390723E-15));
#18703=CARTESIAN_POINT('',(42.4098590973783,-9.6774919964071,6.16441400296896));
#18704=CARTESIAN_POINT('',(40.3533668208875,-9.68791960221073,0.));
#18705=CARTESIAN_POINT('Ctrl Pts',(42.4098590973783,-9.67749199640711,6.16441400296899));
#18706=CARTESIAN_POINT('Ctrl Pts',(41.7676558436448,-9.59321371330007,5.27522994637944));
#18707=CARTESIAN_POINT('Ctrl Pts',(41.26450688868,-9.54543902450228,4.29090746118668));
#18708=CARTESIAN_POINT('Ctrl Pts',(40.5654142930054,-9.54624402163765,2.19762693960537));
#18709=CARTESIAN_POINT('Ctrl Pts',(40.3758825202101,-9.59413431999296,1.10189111929208));
#18710=CARTESIAN_POINT('Ctrl Pts',(40.3533668208875,-9.68791960221072,1.38777878078145E-15));
#18711=CARTESIAN_POINT('',(42.4098958173846,-9.67733107621065,-6.16441400296897));
#18712=CARTESIAN_POINT('Ctrl Pts',(42.4098958173845,-9.67733107621065,-6.16441400296901));
#18713=CARTESIAN_POINT('Ctrl Pts',(41.7675420990818,-9.59246138875226,-5.27484593811599));
#18714=CARTESIAN_POINT('Ctrl Pts',(41.2639415960371,-9.54628772229384,-4.29007656912504));
#18715=CARTESIAN_POINT('Ctrl Pts',(40.5651930542684,-9.54677487452529,-2.19706468910702));
#18716=CARTESIAN_POINT('Ctrl Pts',(40.3761895042215,-9.59285563076689,-1.10157448537428));
#18717=CARTESIAN_POINT('Ctrl Pts',(40.3533668208875,-9.68791960221073,-8.32667268468867E-16));
#18718=CARTESIAN_POINT('',(42.8205093412358,-7.65858862696908,-6.16441400296897));
#18719=CARTESIAN_POINT('Origin',(-5.20417042793042E-15,1.73472347597681E-15,
-6.16441400296897));
#18720=CARTESIAN_POINT('',(40.7312208280701,-7.95095276397668,0.));
#18721=CARTESIAN_POINT('Ctrl Pts',(40.7312208280701,-7.95095276397666,2.4980018054066E-15));
#18722=CARTESIAN_POINT('Ctrl Pts',(40.7499070073971,-7.85522701648535,-1.09898083808689));
#18723=CARTESIAN_POINT('Ctrl Pts',(40.93935088668,-7.78356366707505,-2.19052946960111));
#18724=CARTESIAN_POINT('Ctrl Pts',(41.4694379593684,-7.71206627980807,-3.75889728453886));
#18725=CARTESIAN_POINT('Ctrl Pts',(41.6870210418007,-7.69424405998532,-4.26878718105426));
#18726=CARTESIAN_POINT('Ctrl Pts',(42.1989397978802,-7.66864652856466,-5.24984087156736));
#18727=CARTESIAN_POINT('Ctrl Pts',(42.4922637655696,-7.66112614630714,-5.71948809610396));
#18728=CARTESIAN_POINT('Ctrl Pts',(42.8205093412358,-7.65858862696907,-6.16441400296899));
#18729=CARTESIAN_POINT('',(42.8204408309399,-7.65897167013825,6.16441400296896));
#18730=CARTESIAN_POINT('Ctrl Pts',(40.7312208280701,-7.95095276397667,-1.11022302462516E-15));
#18731=CARTESIAN_POINT('Ctrl Pts',(40.7496489394968,-7.85654904932192,1.09886774242332));
#18732=CARTESIAN_POINT('Ctrl Pts',(40.9392067605215,-7.78406098621475,2.19020735614115));
#18733=CARTESIAN_POINT('Ctrl Pts',(41.6468427282638,-7.68710741120429,4.28336653879352));
#18734=CARTESIAN_POINT('Ctrl Pts',(42.1619315066373,-7.66466187441098,5.27197367572231));
#18735=CARTESIAN_POINT('Ctrl Pts',(42.8204408309398,-7.65897167013822,6.16441400296896));
#18736=CARTESIAN_POINT('Origin',(-1.73472347597681E-15,-1.73472347597681E-15,
6.16441400296896));
#18737=CARTESIAN_POINT('Origin',(0.,0.,-6.93889390390723E-15));
#18738=CARTESIAN_POINT('',(40.6009371733745,-15.6145413203111,6.16441400296896));
#18739=CARTESIAN_POINT('',(38.5638930200078,-15.332193422384,1.04083408558608E-14));
#18740=CARTESIAN_POINT('Ctrl Pts',(40.6009371733744,-15.6145413203111,6.16441400296898));
#18741=CARTESIAN_POINT('Ctrl Pts',(39.9772646730137,-15.4397258164132,5.27522994637943));
#18742=CARTESIAN_POINT('Ctrl Pts',(39.4860360960394,-15.3208318429088,4.29090746118668));
#18743=CARTESIAN_POINT('Ctrl Pts',(38.7939446919434,-15.2221373966425,2.19762693960533));
#18744=CARTESIAN_POINT('Ctrl Pts',(38.5995265792476,-15.2425670572197,1.10189111929201));
#18745=CARTESIAN_POINT('Ctrl Pts',(38.5638930200078,-15.332193422384,1.19348975147204E-14));
#18746=CARTESIAN_POINT('',(40.600996420953,-15.614387263859,-6.16441400296897));
#18747=CARTESIAN_POINT('Ctrl Pts',(40.6010020885968,-15.6143888578498,-6.16442208610001));
#18748=CARTESIAN_POINT('Ctrl Pts',(39.9772648207935,-15.4389665559052,-5.27485402124762));
#18749=CARTESIAN_POINT('Ctrl Pts',(39.485355774973,-15.3215914526464,-4.29007656912584));
#18750=CARTESIAN_POINT('Ctrl Pts',(38.793650156874,-15.2226313606578,-2.19706468916126));
#18751=CARTESIAN_POINT('Ctrl Pts',(38.6000124150605,-15.2413450715717,-1.10157448565927));
#18752=CARTESIAN_POINT('Ctrl Pts',(38.5638930200078,-15.332193422384,8.88178419700125E-15));
#18753=CARTESIAN_POINT('',(41.2947274963709,-13.6746290991923,-6.16441400296897));
#18754=CARTESIAN_POINT('Origin',(-5.20417042793042E-15,1.73472347597681E-15,
-6.16441400296897));
#18755=CARTESIAN_POINT('',(39.1850971728872,-13.6666806339868,0.));
#18756=CARTESIAN_POINT('Ctrl Pts',(39.1850971728872,-13.6666806339868,1.04083408558608E-16));
#18757=CARTESIAN_POINT('Ctrl Pts',(39.189101496907,-13.6551994389527,-0.137010845854338));
#18758=CARTESIAN_POINT('Ctrl Pts',(39.1956781881385,-13.6444618420239,-0.273849719838171));
#18759=CARTESIAN_POINT('Ctrl Pts',(39.2139780494464,-13.6244471777117,-0.547496131363631));
#18760=CARTESIAN_POINT('Ctrl Pts',(39.225701021394,-13.6151774048816,-0.684223919454616));
#18761=CARTESIAN_POINT('Ctrl Pts',(39.2685773960156,-13.5895886129705,-1.09397285880303));
#18762=CARTESIAN_POINT('Ctrl Pts',(39.3074166219997,-13.5755172628307,-1.36621764182805));
#18763=CARTESIAN_POINT('Ctrl Pts',(39.4545152562845,-13.5422635943353,-2.17875768610048));
#18764=CARTESIAN_POINT('Ctrl Pts',(39.5931123698217,-13.5321709123776,-2.71300426676969));
#18765=CARTESIAN_POINT('Ctrl Pts',(39.9497974103409,-13.53528492147,-3.7588972864178));
#18766=CARTESIAN_POINT('Ctrl Pts',(40.1677021769761,-13.5486094073543,-4.26878718251924));
#18767=CARTESIAN_POINT('Ctrl Pts',(40.6780532465233,-13.5961260568701,-5.24984087225545));
#18768=CARTESIAN_POINT('Ctrl Pts',(40.9694618609575,-13.6304265742619,-5.71948809643021));
#18769=CARTESIAN_POINT('Ctrl Pts',(41.2947274963708,-13.6746290991923,-6.164414002969));
#18770=CARTESIAN_POINT('',(41.2946051706827,-13.6749984935074,6.16441400296896));
#18771=CARTESIAN_POINT('Ctrl Pts',(39.1850971728872,-13.6666806339868,1.66533453693773E-15));
#18772=CARTESIAN_POINT('Ctrl Pts',(39.2167727620941,-13.5758604067257,1.09886774242333));
#18773=CARTESIAN_POINT('Ctrl Pts',(39.4147172847985,-13.5310870582244,2.19020735614118));
#18774=CARTESIAN_POINT('Ctrl Pts',(40.1289484710636,-13.5358274291177,4.28336653879346));
#18775=CARTESIAN_POINT('Ctrl Pts',(40.6419887213086,-13.5869151317157,5.27197367572221));
#18776=CARTESIAN_POINT('Ctrl Pts',(41.2946051706827,-13.6749984935074,6.16441400296898));
#18777=CARTESIAN_POINT('Origin',(-1.73472347597681E-15,-1.73472347597681E-15,
6.16441400296896));
#18778=CARTESIAN_POINT('Origin',(0.,0.,-6.93889390390723E-15));
#18779=CARTESIAN_POINT('',(37.9654972519551,-21.2337236115523,6.16441400296896));
#18780=CARTESIAN_POINT('',(35.9893695663249,-20.6643479988721,0.));
#18781=CARTESIAN_POINT('Ctrl Pts',(37.965497251955,-21.2337236115523,6.16441400296898));
#18782=CARTESIAN_POINT('Ctrl Pts',(37.3730516785514,-20.9719296263966,5.27522994637944));
#18783=CARTESIAN_POINT('Ctrl Pts',(36.9037434768085,-20.7843367066242,4.29090746118667));
#18784=CARTESIAN_POINT('Ctrl Pts',(36.2327422494516,-20.588151951271,2.19762693960533));
#18785=CARTESIAN_POINT('Ctrl Pts',(36.0373955889743,-20.580705085095,1.101891119292));
#18786=CARTESIAN_POINT('Ctrl Pts',(35.9893695663249,-20.6643479988721,8.32667268468867E-16));
#18787=CARTESIAN_POINT('',(37.9655778209991,-21.23357955498,-6.16441400296898));
#18788=CARTESIAN_POINT('Ctrl Pts',(37.965577820999,-21.23357955498,-6.164414002969));
#18789=CARTESIAN_POINT('Ctrl Pts',(37.3731544963901,-20.9711757310157,-5.27484593906386));
#18790=CARTESIAN_POINT('Ctrl Pts',(36.9029619776889,-20.7849917652452,-4.29007657121741));
#18791=CARTESIAN_POINT('Ctrl Pts',(36.2323804143473,-20.5885989707562,-2.19706469153443));
#18792=CARTESIAN_POINT('Ctrl Pts',(36.038050386442,-20.5795646790169,-1.10157448713195));
#18793=CARTESIAN_POINT('Ctrl Pts',(35.9893695663249,-20.6643479988721,5.55111512312578E-16));
#18794=CARTESIAN_POINT('',(38.9283040838375,-19.4122935573384,-6.16441400296897));
#18795=CARTESIAN_POINT('Origin',(-5.20417042793042E-15,1.73472347597681E-15,
-6.16441400296897));
#18796=CARTESIAN_POINT('',(36.8412779397532,-19.1041942977415,0.));
#18797=CARTESIAN_POINT('Ctrl Pts',(36.8412779397531,-19.1041942977415,4.5102810375397E-16));
#18798=CARTESIAN_POINT('Ctrl Pts',(36.8468754499427,-19.0933998394435,-0.137010845862249));
#18799=CARTESIAN_POINT('Ctrl Pts',(36.8549133193103,-19.083707496519,-0.273849719841702));
#18800=CARTESIAN_POINT('Ctrl Pts',(36.8758752981308,-19.0665008944338,-0.547496131366671));
#18801=CARTESIAN_POINT('Ctrl Pts',(36.8887981733482,-19.0589938273821,-0.684223919457815));
#18802=CARTESIAN_POINT('Ctrl Pts',(36.9348797930813,-19.0397674367968,-1.09397285880578));
#18803=CARTESIAN_POINT('Ctrl Pts',(36.9753262536659,-19.0313667108765,-1.36621764182999));
#18804=CARTESIAN_POINT('Ctrl Pts',(37.1256601264072,-19.0193858351252,-2.17875768610118));
#18805=CARTESIAN_POINT('Ctrl Pts',(37.2642828595705,-19.0291203079137,-2.71300426676973));
#18806=CARTESIAN_POINT('Ctrl Pts',(37.6168941909741,-19.0829641947397,-3.75889728641827));
#18807=CARTESIAN_POINT('Ctrl Pts',(37.8306847292225,-19.1271641381968,-4.2687871825209));
#18808=CARTESIAN_POINT('Ctrl Pts',(38.3290788364555,-19.2468276666622,-5.24984087225791));
#18809=CARTESIAN_POINT('Ctrl Pts',(38.6126398587854,-19.3222508240785,-5.71948809643139));
#18810=CARTESIAN_POINT('Ctrl Pts',(38.9283040838375,-19.4122935573384,-6.16441400296899));
#18811=CARTESIAN_POINT('',(38.928130432958,-19.412641782988,6.16441400296896));
#18812=CARTESIAN_POINT('Ctrl Pts',(36.8412779397531,-19.1041942977415,-8.32667268468867E-16));
#18813=CARTESIAN_POINT('Ctrl Pts',(36.885556183089,-19.0188063957971,1.09886774242324));
#18814=CARTESIAN_POINT('Ctrl Pts',(37.0878578278155,-19.0026592181615,2.19020735614101));
#18815=CARTESIAN_POINT('Ctrl Pts',(37.7941445453238,-19.1089970346771,4.2833665387935));
#18816=CARTESIAN_POINT('Ctrl Pts',(38.2946922474313,-19.2325779783665,5.27197367572228));
#18817=CARTESIAN_POINT('Ctrl Pts',(38.928130432958,-19.412641782988,6.16441400296895));
#18818=CARTESIAN_POINT('Origin',(-1.73472347597681E-15,-1.73472347597681E-15,
6.16441400296896));
#18819=CARTESIAN_POINT('Origin',(0.,0.,-6.93889390390723E-15));
#18820=CARTESIAN_POINT('',(34.557189289939,-26.4206485230648,6.16441400296897));
#18821=CARTESIAN_POINT('',(32.682206333043,-25.575836041162,0.));
#18822=CARTESIAN_POINT('Ctrl Pts',(34.557189289939,-26.4206485230648,6.16441400296899));
#18823=CARTESIAN_POINT('Ctrl Pts',(34.008031126895,-26.0772054272376,5.27522994637943));
#18824=CARTESIAN_POINT('Ctrl Pts',(33.5701970619979,-25.8247324120704,4.29090746118663));
#18825=CARTESIAN_POINT('Ctrl Pts',(32.9339456613615,-25.5350511034992,2.19762693960548));
#18826=CARTESIAN_POINT('Ctrl Pts',(32.7416471477766,-25.4998793072902,1.10189111929232));
#18827=CARTESIAN_POINT('Ctrl Pts',(32.682206333043,-25.575836041162,-2.77555756156289E-16));
#18828=CARTESIAN_POINT('',(34.5572895402933,-26.4205173989522,-6.16441400296897));
#18829=CARTESIAN_POINT('Ctrl Pts',(34.5572895402933,-26.4205173989522,-6.164414002969));
#18830=CARTESIAN_POINT('Ctrl Pts',(34.0082401881097,-26.0764738375632,-5.274845938116));
#18831=CARTESIAN_POINT('Ctrl Pts',(33.5693302919201,-25.8252695836844,-4.29007656912555));
#18832=CARTESIAN_POINT('Ctrl Pts',(32.9335238913098,-25.5354420783965,-2.197064689243));
#18833=CARTESIAN_POINT('Ctrl Pts',(32.7424575769921,-25.4988436963802,-1.1015744860932));
#18834=CARTESIAN_POINT('Ctrl Pts',(32.682206333043,-25.575836041162,1.94289029309402E-15));
#18835=CARTESIAN_POINT('',(35.7694126601179,-24.7547796990844,-6.16441400296897));
#18836=CARTESIAN_POINT('Origin',(-5.20417042793042E-15,1.73472347597681E-15,
-6.16441400296897));
#18837=CARTESIAN_POINT('',(33.7474765292382,-24.1528016575411,0.));
#18838=CARTESIAN_POINT('Ctrl Pts',(33.7474765292382,-24.1528016575411,2.77555756156289E-16));
#18839=CARTESIAN_POINT('Ctrl Pts',(33.754553276426,-24.1429136800298,-0.13701084572592));
#18840=CARTESIAN_POINT('Ctrl Pts',(33.7638886960778,-24.1344638992664,-0.273849719562642));
#18841=CARTESIAN_POINT('Ctrl Pts',(33.7870860669397,-24.1204156362131,-0.547496130807772));
#18842=CARTESIAN_POINT('Ctrl Pts',(33.8009457729332,-24.1148240971771,-0.684223918759634));
#18843=CARTESIAN_POINT('Ctrl Pts',(33.849294548812,-24.1023515017802,-1.09397285769292));
#18844=CARTESIAN_POINT('Ctrl Pts',(33.8905248706275,-24.0997924146194,-1.36621764044298));
#18845=CARTESIAN_POINT('Ctrl Pts',(34.0410336174366,-24.1093282276182,-2.17875768389983));
#18846=CARTESIAN_POINT('Ctrl Pts',(34.1768600108824,-24.1386916892646,-2.71300426404658));
#18847=CARTESIAN_POINT('Ctrl Pts',(34.5182194830272,-24.2421693473793,-3.75889728379987));
#18848=CARTESIAN_POINT('Ctrl Pts',(34.723543634163,-24.3163449650217,-4.2687871804743));
#18849=CARTESIAN_POINT('Ctrl Pts',(35.1998349126628,-24.5057193681818,-5.24984087129297));
#18850=CARTESIAN_POINT('Ctrl Pts',(35.4697758584417,-24.6207297677412,-5.71948809597396));
#18851=CARTESIAN_POINT('Ctrl Pts',(35.7694126601179,-24.7547796990843,-6.164414002969));
#18852=CARTESIAN_POINT('',(35.7691912190763,-24.755099667203,6.16441400296896));
#18853=CARTESIAN_POINT('Ctrl Pts',(33.7474765292382,-24.1528016575411,8.32667268468867E-16));
#18854=CARTESIAN_POINT('Ctrl Pts',(33.8034560493565,-24.0745843323587,1.09886774242322));
#18855=CARTESIAN_POINT('Ctrl Pts',(34.0059965380084,-24.0873920355607,2.19020735614096));
#18856=CARTESIAN_POINT('Ctrl Pts',(34.689960825954,-24.2931625664075,4.28336653879352));
#18857=CARTESIAN_POINT('Ctrl Pts',(35.1678262721695,-24.4867209995526,5.27197367572231));
#18858=CARTESIAN_POINT('Ctrl Pts',(35.7691912190763,-24.755099667203,6.16441400296897));
#18859=CARTESIAN_POINT('Origin',(-1.73472347597681E-15,-1.73472347597681E-15,
6.16441400296896));
#18860=CARTESIAN_POINT('Origin',(0.,0.,-6.93889390390723E-15));
#18861=CARTESIAN_POINT('',(30.4453966086845,-31.0697252215063,6.16441400296896));
#18862=CARTESIAN_POINT('',(28.7097276265208,-29.9666738162745,0.));
#18863=CARTESIAN_POINT('Ctrl Pts',(30.4453966086845,-31.0697252215063,6.16441400296898));
#18864=CARTESIAN_POINT('Ctrl Pts',(29.9507051325582,-30.6516245260304,5.27522994637932));
#18865=CARTESIAN_POINT('Ctrl Pts',(29.5532582434591,-30.3394110379853,4.29090746118637));
#18866=CARTESIAN_POINT('Ctrl Pts',(28.9647089132626,-29.9621302522667,2.19762693960548));
#18867=CARTESIAN_POINT('Ctrl Pts',(28.7793731897637,-29.8999495223686,1.10189111929233));
#18868=CARTESIAN_POINT('Ctrl Pts',(28.7097276265208,-29.9666738162744,-5.55111512312578E-16));
#18869=CARTESIAN_POINT('',(30.44551449954,-31.0696096991627,-6.16441400296898));
#18870=CARTESIAN_POINT('Ctrl Pts',(30.4455144995399,-31.0696096991627,-6.164414002969));
#18871=CARTESIAN_POINT('Ctrl Pts',(29.9510161818958,-30.6509301353986,-5.27484593811587));
#18872=CARTESIAN_POINT('Ctrl Pts',(29.552323848359,-30.3398193877237,-4.29007656912524));
#18873=CARTESIAN_POINT('Ctrl Pts',(28.9642357946952,-29.9624572234643,-2.19706468924339));
#18874=CARTESIAN_POINT('Ctrl Pts',(28.7803227527825,-29.8990397885823,-1.10157448609764));
#18875=CARTESIAN_POINT('Ctrl Pts',(28.7097276265208,-29.9666738162745,-2.77555756156289E-16));
#18876=CARTESIAN_POINT('',(31.882359145105,-29.5933299130488,-6.16441400296898));
#18877=CARTESIAN_POINT('Origin',(-5.20417042793042E-15,1.73472347597681E-15,
-6.16441400296897));
#18878=CARTESIAN_POINT('',(29.9666738162738,-28.7097276265216,0.));
#18879=CARTESIAN_POINT('Ctrl Pts',(29.9666738162737,-28.7097276265215,2.42861286636753E-16));
#18880=CARTESIAN_POINT('Ctrl Pts',(29.9750857383069,-28.7009474204877,-0.137010845870293));
#18881=CARTESIAN_POINT('Ctrl Pts',(29.9855286660416,-28.6939122150426,-0.273849719845077));
#18882=CARTESIAN_POINT('Ctrl Pts',(30.0104891974329,-28.6833082731318,-0.54749613137037));
#18883=CARTESIAN_POINT('Ctrl Pts',(30.0250035905977,-28.6797460897202,-0.68422391946205));
#18884=CARTESIAN_POINT('Ctrl Pts',(30.0746352811228,-28.6742811955971,-1.09397285881242));
#18885=CARTESIAN_POINT('Ctrl Pts',(30.115810133854,-28.6776158428596,-1.36621764183756));
#18886=CARTESIAN_POINT('Ctrl Pts',(30.263429831203,-28.7084742231074,-2.17875768610662));
#18887=CARTESIAN_POINT('Ctrl Pts',(30.3936948517472,-28.7568689184009,-2.71300426677264));
#18888=CARTESIAN_POINT('Ctrl Pts',(30.7168533707401,-28.907873841448,-3.75889728641653));
#18889=CARTESIAN_POINT('Ctrl Pts',(30.9095313269346,-29.0105151315945,-4.26878718251739));
#18890=CARTESIAN_POINT('Ctrl Pts',(31.3540238590801,-29.2657452924991,-5.24984087225377));
#18891=CARTESIAN_POINT('Ctrl Pts',(31.6048495086121,-29.4180016539316,-5.71948809642935));
#18892=CARTESIAN_POINT('Ctrl Pts',(31.8823591451049,-29.5933299130488,-6.16441400296902));
#18893=CARTESIAN_POINT('',(31.8820944218039,-29.5936151100062,6.16441400296897));
#18894=CARTESIAN_POINT('Ctrl Pts',(29.9666738162737,-28.7097276265215,-1.11022302462516E-15));
#18895=CARTESIAN_POINT('Ctrl Pts',(30.0332150315766,-28.6402731572817,1.09886774242332));
#18896=CARTESIAN_POINT('Ctrl Pts',(30.2318712238835,-28.6817750134187,2.19020735614117));
#18897=CARTESIAN_POINT('Ctrl Pts',(30.879589541754,-28.9827893639817,4.28336653879344));
#18898=CARTESIAN_POINT('Ctrl Pts',(31.3250447696425,-29.24238499506,5.27197367572218));
#18899=CARTESIAN_POINT('Ctrl Pts',(31.8820944218039,-29.5936151100061,6.16441400296897));
#18900=CARTESIAN_POINT('Origin',(-1.73472347597681E-15,-1.73472347597681E-15,
6.16441400296896));
#18901=CARTESIAN_POINT('Origin',(0.,0.,-6.93889390390723E-15));
#18902=CARTESIAN_POINT('',(25.7138234497508,-35.0863119121267,6.16441400296896));
#18903=CARTESIAN_POINT('',(24.1528016575403,-33.7474765292388,0.));
#18904=CARTESIAN_POINT('Ctrl Pts',(25.7138234497508,-35.0863119121267,6.16441400296899));
#18905=CARTESIAN_POINT('Ctrl Pts',(25.283669152424,-34.6020649414593,5.27522994637943));
#18906=CARTESIAN_POINT('Ctrl Pts',(24.9347003116427,-34.2364667468035,4.29090746118665));
#18907=CARTESIAN_POINT('Ctrl Pts',(24.4058342190125,-33.7792668327467,2.19762693960535));
#18908=CARTESIAN_POINT('Ctrl Pts',(24.231234186466,-33.6913429895057,1.10189111929205));
#18909=CARTESIAN_POINT('Ctrl Pts',(24.1528016575402,-33.7474765292388,1.94289029309402E-15));
#18910=CARTESIAN_POINT('',(25.7139565811959,-35.0862143432485,-6.16441400296897));
#18911=CARTESIAN_POINT('Ctrl Pts',(25.7139565811959,-35.0862143432484,-6.164414002969));
#18912=CARTESIAN_POINT('Ctrl Pts',(25.2840758578255,-34.6014218856529,-5.27484593811503));
#18913=CARTESIAN_POINT('Ctrl Pts',(24.9337173131074,-34.2367379618448,-4.29007656912494));
#18914=CARTESIAN_POINT('Ctrl Pts',(24.4053193832454,-33.7795231440541,-2.19706468921654));
#18915=CARTESIAN_POINT('Ctrl Pts',(24.2323035529173,-33.6905776524064,-1.10157448595652));
#18916=CARTESIAN_POINT('Ctrl Pts',(24.1528016575402,-33.7474765292388,-1.94289029309402E-15));
#18917=CARTESIAN_POINT('',(27.3462727390257,-33.829445270102,-6.16441400296897));
#18918=CARTESIAN_POINT('Origin',(-5.20417042793042E-15,1.73472347597681E-15,
-6.16441400296897));
#18919=CARTESIAN_POINT('',(25.5758360411612,-32.6822063330437,0.));
#18920=CARTESIAN_POINT('Ctrl Pts',(25.5758360411612,-32.6822063330437,7.63278329429795E-16));
#18921=CARTESIAN_POINT('Ctrl Pts',(25.5854118955597,-32.6747126381702,-0.137010845871668));
#18922=CARTESIAN_POINT('Ctrl Pts',(25.5967497434736,-32.6692352245437,-0.273849719849249));
#18923=CARTESIAN_POINT('Ctrl Pts',(25.6229653109251,-32.6622914694593,-0.547496131378874));
#18924=CARTESIAN_POINT('Ctrl Pts',(25.6378389200524,-32.6608311574542,-0.684223919472369));
#18925=CARTESIAN_POINT('Ctrl Pts',(25.6877431670554,-32.6624852140835,-1.09397285882336));
#18926=CARTESIAN_POINT('Ctrl Pts',(25.7280243493695,-32.6716457119525,-1.36621764184875));
#18927=CARTESIAN_POINT('Ctrl Pts',(25.8697498856548,-32.7231984717385,-2.17875768611436));
#18928=CARTESIAN_POINT('Ctrl Pts',(25.9918017128807,-32.7896392241452,-2.71300426677627));
#18929=CARTESIAN_POINT('Ctrl Pts',(26.2901807029013,-32.9850973871748,-3.75889728641619));
#18930=CARTESIAN_POINT('Ctrl Pts',(26.4662900967122,-33.1141148691595,-4.26878718251706));
#18931=CARTESIAN_POINT('Ctrl Pts',(26.8699352967115,-33.4300050378656,-5.24984087225354));
#18932=CARTESIAN_POINT('Ctrl Pts',(27.0965395633376,-33.6164078608233,-5.7194880964293));
#18933=CARTESIAN_POINT('Ctrl Pts',(27.3462727390257,-33.8294452701019,-6.164414002969));
#18934=CARTESIAN_POINT('',(27.3459701224716,-33.8296898901083,6.16441400296896));
#18935=CARTESIAN_POINT('Ctrl Pts',(25.5758360411612,-32.6822063330437,5.55111512312578E-16));
#18936=CARTESIAN_POINT('Ctrl Pts',(25.651584364394,-32.62292861245,1.09886774242327));
#18937=CARTESIAN_POINT('Ctrl Pts',(25.8423121931576,-32.6922797634123,2.19020735614105));
#18938=CARTESIAN_POINT('Ctrl Pts',(26.4405988638666,-33.0824101495678,4.28336653879351));
#18939=CARTESIAN_POINT('Ctrl Pts',(26.8445756895753,-33.4027583601428,5.2719736757223));
#18940=CARTESIAN_POINT('Ctrl Pts',(27.3459701224716,-33.8296898901082,6.16441400296898));
#18941=CARTESIAN_POINT('Origin',(-1.73472347597681E-15,-1.73472347597681E-15,
6.16441400296896));
#18942=CARTESIAN_POINT('Origin',(0.,0.,-6.93889390390723E-15));
#18943=CARTESIAN_POINT('',(20.4587909979238,-38.3886424727845,6.16441400296896));
#18944=CARTESIAN_POINT('',(19.1041942977406,-36.8412779397537,0.));
#18945=CARTESIAN_POINT('Ctrl Pts',(20.4587909979237,-38.3886424727845,6.16441400296898));
#18946=CARTESIAN_POINT('Ctrl Pts',(20.1019305804272,-37.8481070987954,5.27522994637938));
#18947=CARTESIAN_POINT('Ctrl Pts',(19.8085437872191,-37.4365667224739,4.29090746118653));
#18948=CARTESIAN_POINT('Ctrl Pts',(19.3501271206775,-36.9087549518735,2.19762693960539));
#18949=CARTESIAN_POINT('Ctrl Pts',(19.1898171322411,-36.7968778711866,1.10189111929213));
#18950=CARTESIAN_POINT('Ctrl Pts',(19.1041942977406,-36.8412779397536,2.77555756156289E-16));
#18951=CARTESIAN_POINT('',(20.4589366597946,-38.38856484359,-6.16441400296897));
#18952=CARTESIAN_POINT('Ctrl Pts',(20.4589366597946,-38.38856484359,-6.16441400296901));
#18953=CARTESIAN_POINT('Ctrl Pts',(20.1024246625473,-37.8475284685787,-5.27484593811585));
#18954=CARTESIAN_POINT('Ctrl Pts',(19.8075321962676,-37.4366952816592,-4.29007656912457));
#18955=CARTESIAN_POINT('Ctrl Pts',(19.3495810482794,-36.9089353855215,-2.19706468916629));
#18956=CARTESIAN_POINT('Ctrl Pts',(19.1909845328796,-36.7962725108444,-1.1015744856864));
#18957=CARTESIAN_POINT('Ctrl Pts',(19.1041942977406,-36.8412779397536,-2.22044604925031E-15));
#18958=CARTESIAN_POINT('',(22.2534950801302,-37.3768906775112,-6.16441400296897));
#18959=CARTESIAN_POINT('Origin',(-5.20417042793042E-15,1.73472347597681E-15,
-6.16441400296897));
#18960=CARTESIAN_POINT('',(20.6643479988712,-35.9893695663254,0.));
#18961=CARTESIAN_POINT('Ctrl Pts',(20.6643479988712,-35.9893695663254,1.04083408558608E-15));
#18962=CARTESIAN_POINT('Ctrl Pts',(20.6748928488534,-35.9833149326307,-0.137010845868849));
#18963=CARTESIAN_POINT('Ctrl Pts',(20.6868948110582,-35.9795068151691,-0.273849719849772));
#18964=CARTESIAN_POINT('Ctrl Pts',(20.7138317412147,-35.9763646017415,-0.547496131381827));
#18965=CARTESIAN_POINT('Ctrl Pts',(20.7287617825137,-35.9770358888848,-0.684223919476415));
#18966=CARTESIAN_POINT('Ctrl Pts',(20.7779226794355,-35.9857752244448,-1.09397285882839));
#18967=CARTESIAN_POINT('Ctrl Pts',(20.8164901826204,-36.0005750916014,-1.36621764185478));
#18968=CARTESIAN_POINT('Ctrl Pts',(20.9494364346222,-36.0717727654041,-2.17875768611945));
#18969=CARTESIAN_POINT('Ctrl Pts',(21.0607904452947,-36.1549070328049,-2.71300426677922));
#18970=CARTESIAN_POINT('Ctrl Pts',(21.3283157705668,-36.3908394712685,-3.7588972864172));
#18971=CARTESIAN_POINT('Ctrl Pts',(21.4842715226045,-36.5436067212075,-4.26878718251819));
#18972=CARTESIAN_POINT('Ctrl Pts',(21.8388523382101,-36.913726284825,-5.24984087225241));
#18973=CARTESIAN_POINT('Ctrl Pts',(22.0366222125346,-37.1304809453732,-5.71948809642862));
#18974=CARTESIAN_POINT('Ctrl Pts',(22.2534950801302,-37.3768906775112,-6.164414002969));
#18975=CARTESIAN_POINT('',(22.2531607307116,-37.3770897408175,6.16441400296896));
#18976=CARTESIAN_POINT('Ctrl Pts',(20.6643479988712,-35.9893695663254,-5.55111512312578E-16));
#18977=CARTESIAN_POINT('Ctrl Pts',(20.7477614126131,-35.9414753178263,1.09886774242329));
#18978=CARTESIAN_POINT('Ctrl Pts',(20.9266782092534,-36.0372639741726,2.19020735614109));
#18979=CARTESIAN_POINT('Ctrl Pts',(21.4633538415015,-36.5085684663016,4.2833665387935));
#18980=CARTESIAN_POINT('Ctrl Pts',(21.8176284618318,-36.8831478906138,5.27197367572225));
#18981=CARTESIAN_POINT('Ctrl Pts',(22.2531607307115,-37.3770897408174,6.16441400296898));
#18982=CARTESIAN_POINT('Origin',(-1.73472347597681E-15,-1.73472347597681E-15,
6.16441400296896));
#18983=CARTESIAN_POINT('Origin',(0.,0.,-6.93889390390723E-15));
#18984=CARTESIAN_POINT('',(14.7872765596602,-40.9094909763997,6.16441400296897));
#18985=CARTESIAN_POINT('',(13.6666806339858,-39.1850971728875,0.));
#18986=CARTESIAN_POINT('Ctrl Pts',(14.7872790713139,-40.9094963016524,6.16442208586935));
#18987=CARTESIAN_POINT('Ctrl Pts',(14.5109771826475,-40.3236762657807,5.27523802927974));
#18988=CARTESIAN_POINT('Ctrl Pts',(14.2791424344108,-39.8745661578182,4.2909074611865));
#18989=CARTESIAN_POINT('Ctrl Pts',(13.9005072353241,-39.2868872562402,2.19762693960545));
#18990=CARTESIAN_POINT('Ctrl Pts',(13.7577507400665,-39.1533344328433,1.10189111929226));
#18991=CARTESIAN_POINT('Ctrl Pts',(13.6666806339858,-39.1850971728875,2.77555756156289E-16));
#18992=CARTESIAN_POINT('',(14.787431786677,-40.9094348672085,-6.16441400296898));
#18993=CARTESIAN_POINT('Ctrl Pts',(14.787431786677,-40.9094348672085,-6.164414002969));
#18994=CARTESIAN_POINT('Ctrl Pts',(14.5115460717211,-40.3231685151554,-5.27484593811647));
#18995=CARTESIAN_POINT('Ctrl Pts',(14.2781228441197,-39.8745494440528,-4.29007656912508));
#18996=CARTESIAN_POINT('Ctrl Pts',(13.8999410427704,-39.2869881391093,-2.19706468910962));
#18997=CARTESIAN_POINT('Ctrl Pts',(13.7589924099839,-39.1529013726384,-1.1015744853883));
#18998=CARTESIAN_POINT('Ctrl Pts',(13.6666806339858,-39.1850971728875,-8.32667268468867E-16));
#18999=CARTESIAN_POINT('',(16.7077004351884,-40.1634503767792,-6.16441400296897));
#19000=CARTESIAN_POINT('Origin',(-5.20417042793042E-15,1.73472347597681E-15,
-6.16441400296897));
#19001=CARTESIAN_POINT('',(15.332193422383,-38.5638930200082,0.));
#19002=CARTESIAN_POINT('Ctrl Pts',(15.332193422383,-38.5638930200082,-4.16333634234434E-16));
#19003=CARTESIAN_POINT('Ctrl Pts',(15.3434926052103,-38.5594007023748,-0.137010845862397));
#19004=CARTESIAN_POINT('Ctrl Pts',(15.3559143563653,-38.5573394033684,-0.27384971984452));
#19005=CARTESIAN_POINT('Ctrl Pts',(15.3830242910069,-38.558062698002,-0.547496131373093));
#19006=CARTESIAN_POINT('Ctrl Pts',(15.397706831891,-38.5608519188229,-0.684223919465796));
#19007=CARTESIAN_POINT('Ctrl Pts',(15.4451236046383,-38.5764986256427,-1.09397285881666));
#19008=CARTESIAN_POINT('Ctrl Pts',(15.4811923055495,-38.5966365794692,-1.36621764184235));
#19009=CARTESIAN_POINT('Ctrl Pts',(15.602652870967,-38.6860297879631,-2.17875768611168));
#19010=CARTESIAN_POINT('Ctrl Pts',(15.701042218552,-38.7841651964116,-2.71300426677608));
#19011=CARTESIAN_POINT('Ctrl Pts',(15.9322678349316,-39.0557690062386,-3.75889728641793));
#19012=CARTESIAN_POINT('Ctrl Pts',(16.0648951358144,-39.2291761234743,-4.2687871825184));
#19013=CARTESIAN_POINT('Ctrl Pts',(16.3631933241489,-39.6459905150278,-5.24984087225277));
#19014=CARTESIAN_POINT('Ctrl Pts',(16.5281027818572,-39.8886845133437,-5.71948809642874));
#19015=CARTESIAN_POINT('Ctrl Pts',(16.7077004351884,-40.1634503767792,-6.164414002969));
#19016=CARTESIAN_POINT('',(16.7073411592906,-40.1635998310296,6.16441400296896));
#19017=CARTESIAN_POINT('Ctrl Pts',(15.332193422383,-38.5638930200082,0.));
#19018=CARTESIAN_POINT('Ctrl Pts',(15.4215738700746,-38.5283572323875,1.09886774242323));
#19019=CARTESIAN_POINT('Ctrl Pts',(15.5850374045654,-38.6486334133062,2.19020735614099));
#19020=CARTESIAN_POINT('Ctrl Pts',(16.0491768301248,-39.191517611079,4.28336653879356));
#19021=CARTESIAN_POINT('Ctrl Pts',(16.3465372354506,-39.6127028922473,5.27197367572238));
#19022=CARTESIAN_POINT('Ctrl Pts',(16.7073411592906,-40.1635998310296,6.16441400296899));
#19023=CARTESIAN_POINT('Origin',(-1.73472347597681E-15,-1.73472347597681E-15,
6.16441400296896));
#19024=CARTESIAN_POINT('Origin',(0.,0.,-6.93889390390723E-15));
#19025=CARTESIAN_POINT('',(2.66275246602648,-43.4184263798756,6.16441400296896));
#19026=CARTESIAN_POINT('',(2.07336642434585,-41.4481742863349,0.));
#19027=CARTESIAN_POINT('Ctrl Pts',(2.66275246602646,-43.4184263798755,6.16441400296898));
#19028=CARTESIAN_POINT('Ctrl Pts',(2.5626970742232,-42.7785553024261,5.27531660683072));
#19029=CARTESIAN_POINT('Ctrl Pts',(2.466792220479,-42.2823616483505,4.29109868658257));
#19030=CARTESIAN_POINT('Ctrl Pts',(2.26906302577183,-41.611750365836,2.19783870908466));
#19031=CARTESIAN_POINT('Ctrl Pts',(2.16970548652323,-41.4433551071959,1.10199792653062));
#19032=CARTESIAN_POINT('Ctrl Pts',(2.07336642434584,-41.4481742863349,0.));
#19033=CARTESIAN_POINT('',(2.66291721304303,-43.4184162760053,-6.16441400296897));
#19034=CARTESIAN_POINT('Ctrl Pts',(2.662917213043,-43.4184162760053,-6.164414002969));
#19035=CARTESIAN_POINT('Ctrl Pts',(2.56337712638025,-42.7781718426724,-5.27484593811569));
#19036=CARTESIAN_POINT('Ctrl Pts',(2.46579977756423,-42.2819620733826,-4.29007656912562));
#19037=CARTESIAN_POINT('Ctrl Pts',(2.26847214514444,-41.6116550038394,-2.19706468899303));
#19038=CARTESIAN_POINT('Ctrl Pts',(2.17100952986354,-41.4432898748974,-1.10157448476846));
#19039=CARTESIAN_POINT('Ctrl Pts',(2.07336642434584,-41.4481742863349,-1.94289029309402E-15));
#19040=CARTESIAN_POINT('',(4.71556960657991,-43.2436515951822,-6.16441400296899));
#19041=CARTESIAN_POINT('Origin',(-5.20417042793042E-15,1.73472347597681E-15,
-6.16441400296897));
#19042=CARTESIAN_POINT('',(3.84642767658858,-41.3213624427944,0.));
#19043=CARTESIAN_POINT('Ctrl Pts',(3.8464276765886,-41.3213624427943,1.38777878078145E-15));
#19044=CARTESIAN_POINT('Ctrl Pts',(3.94354036378048,-41.3123226409659,-1.09898083808903));
#19045=CARTESIAN_POINT('Ctrl Pts',(4.06567335249903,-41.4739028133711,-2.19052946960313));
#19046=CARTESIAN_POINT('Ctrl Pts',(4.2836173795468,-41.9623744932969,-3.75889728453861));
#19047=CARTESIAN_POINT('Ctrl Pts',(4.36201791237544,-42.1661228325091,-4.26878718105355));
#19048=CARTESIAN_POINT('Ctrl Pts',(4.53080274396104,-42.6500936240533,-5.24984087156751));
#19049=CARTESIAN_POINT('Ctrl Pts',(4.62065740929872,-42.9294171735218,-5.71948809610405));
#19050=CARTESIAN_POINT('Ctrl Pts',(4.71556960657992,-43.2436515951822,-6.16441400296901));
#19051=CARTESIAN_POINT('',(4.71518277776759,-43.2436937757663,6.16441400296896));
#19052=CARTESIAN_POINT('Ctrl Pts',(3.8464276765886,-41.3213624427943,-1.94289029309402E-15));
#19053=CARTESIAN_POINT('Ctrl Pts',(3.94219917643291,-41.3124474863202,1.09886774242318));
#19054=CARTESIAN_POINT('Ctrl Pts',(4.06515557324172,-41.4739046363273,2.19020735614089));
#19055=CARTESIAN_POINT('Ctrl Pts',(4.3575459377361,-42.1255613966704,4.28336653879355));
#19056=CARTESIAN_POINT('Ctrl Pts',(4.52420114711007,-42.6134666723851,5.27198233656275));
#19057=CARTESIAN_POINT('Ctrl Pts',(4.71518449972428,-43.2436994581107,6.16442204944812));
#19058=CARTESIAN_POINT('Origin',(-1.73472347597681E-15,-1.73472347597681E-15,
6.16441400296896));
#19059=CARTESIAN_POINT('Origin',(0.,0.,-6.93889390390723E-15));
#19060=CARTESIAN_POINT('',(8.81473581362626,-42.5975402169653,6.16441400296897));
#19061=CARTESIAN_POINT('',(7.95095276397613,-40.7312208280712,0.));
#19062=CARTESIAN_POINT('Ctrl Pts',(8.81473754185242,-42.5975458454603,6.16442208586935));
#19063=CARTESIAN_POINT('Ctrl Pts',(8.6246188916806,-41.9783667542709,5.27523802927979));
#19064=CARTESIAN_POINT('Ctrl Pts',(8.45905891928443,-41.5008344149427,4.29090746118661));
#19065=CARTESIAN_POINT('Ctrl Pts',(8.16791310841188,-40.8652518300962,2.19762693960268));
#19066=CARTESIAN_POINT('Ctrl Pts',(8.04561621690065,-40.7127420143402,1.10189111928629));
#19067=CARTESIAN_POINT('Ctrl Pts',(7.95095276397564,-40.7312208280703,2.66453525910038E-14));
#19068=CARTESIAN_POINT('',(8.81489744582342,-42.5975067699932,-6.16441400296899));
#19069=CARTESIAN_POINT('Ctrl Pts',(8.81489744582339,-42.5975067699932,-6.16441400296902));
#19070=CARTESIAN_POINT('Ctrl Pts',(8.62525425083943,-41.9779451335314,-5.27484593863276));
#19071=CARTESIAN_POINT('Ctrl Pts',(8.45805208576314,-41.5006727690235,-4.29007657026494));
#19072=CARTESIAN_POINT('Ctrl Pts',(8.24020736641904,-41.0245381184933,-2.72168992255145));
#19073=CARTESIAN_POINT('Ctrl Pts',(8.17348042064547,-40.9065321202818,-2.18495234743267));
#19074=CARTESIAN_POINT('Ctrl Pts',(8.08284749514825,-40.7929641040503,-1.36923477588193));
#19075=CARTESIAN_POINT('Ctrl Pts',(8.05426390892374,-40.7657215585915,-1.09614446425365));
#19076=CARTESIAN_POINT('Ctrl Pts',(8.01374302361062,-40.740817010984,-0.68531858718774));
#19077=CARTESIAN_POINT('Ctrl Pts',(8.00063920350535,-40.7351764066767,-0.548301186438288));
#19078=CARTESIAN_POINT('Ctrl Pts',(7.97520828346697,-40.7292135752535,-0.274113036175805));
#19079=CARTESIAN_POINT('Ctrl Pts',(7.96288931341435,-40.7288907495992,-0.137034229957148));
#19080=CARTESIAN_POINT('Ctrl Pts',(7.95095276397563,-40.7312208280703,-2.77208811461094E-14));
#19081=CARTESIAN_POINT('',(10.821785190392,-42.1323980482125,-6.16441400296898));
#19082=CARTESIAN_POINT('Origin',(-5.20417042793042E-15,1.73472347597681E-15,
-6.16441400296897));
#19083=CARTESIAN_POINT('',(9.68791960220972,-40.3533668208878,0.));
#19084=CARTESIAN_POINT('Ctrl Pts',(9.68791960220971,-40.3533668208877,6.93889390390723E-17));
#19085=CARTESIAN_POINT('Ctrl Pts',(9.69974309910563,-40.3505282699471,-0.137010845854286));
#19086=CARTESIAN_POINT('Ctrl Pts',(9.71233176818024,-40.3502557514988,-0.273849719837571));
#19087=CARTESIAN_POINT('Ctrl Pts',(9.73906282721921,-40.3548298299992,-0.547496131362149));
#19088=CARTESIAN_POINT('Ctrl Pts',(9.75319897349823,-40.3596802040047,-0.684223919452797));
#19089=CARTESIAN_POINT('Ctrl Pts',(9.79790635332026,-40.3819157602534,-1.09397285880181));
#19090=CARTESIAN_POINT('Ctrl Pts',(9.83074199722253,-40.4069818500826,-1.36621764182707));
#19091=CARTESIAN_POINT('Ctrl Pts',(9.93824428920984,-40.5127508053307,-2.17875768609988));
#19092=CARTESIAN_POINT('Ctrl Pts',(10.0216660503208,-40.6238896009105,-2.71300426676926));
#19093=CARTESIAN_POINT('Ctrl Pts',(10.2118848710489,-40.9256357117772,-3.75889728641769));
#19094=CARTESIAN_POINT('Ctrl Pts',(10.3184838113865,-41.1161526274705,-4.26878718251922));
#19095=CARTESIAN_POINT('Ctrl Pts',(10.554426881542,-41.5711767079482,-5.24984087225529));
#19096=CARTESIAN_POINT('Ctrl Pts',(10.6831188416295,-41.8348694941004,-5.7194880964301));
#19097=CARTESIAN_POINT('Ctrl Pts',(10.821785190392,-42.1323980482124,-6.164414002969));
#19098=CARTESIAN_POINT('',(10.8214083018597,-42.1324948509395,6.16441400296896));
#19099=CARTESIAN_POINT('Ctrl Pts',(9.68791960220971,-40.3533668208877,8.32667268468867E-16));
#19100=CARTESIAN_POINT('Ctrl Pts',(9.7814475556879,-40.3309129003046,1.0988677424233));
#19101=CARTESIAN_POINT('Ctrl Pts',(9.92613018185704,-40.4732281296003,2.19020735614111));
#19102=CARTESIAN_POINT('Ctrl Pts',(10.3082848604908,-41.0766404762988,4.2833665387935));
#19103=CARTESIAN_POINT('Ctrl Pts',(10.5426776504761,-41.5358574965965,5.27197367572226));
#19104=CARTESIAN_POINT('Ctrl Pts',(10.8214083018597,-42.1324948509395,6.16441400296897));
#19105=CARTESIAN_POINT('Origin',(-1.73472347597681E-15,-1.73472347597681E-15,
6.16441400296896));
#19106=CARTESIAN_POINT('Origin',(-1.73472347597681E-15,-1.73472347597681E-15,
11.35));
#19107=CARTESIAN_POINT('',(-42.3548619717231,-1.97942721139887,10.4489096280657));
#19108=CARTESIAN_POINT('',(-42.3779453595728,0.399648641330071,10.4701702229062));
#19109=CARTESIAN_POINT('Ctrl Pts',(-42.3548619717231,-1.97942721139887,
10.4489096280657));
#19110=CARTESIAN_POINT('Ctrl Pts',(-42.277687969919,-1.85081682220853,10.5320034604966));
#19111=CARTESIAN_POINT('Ctrl Pts',(-42.2140016405931,-1.7066924272665,10.6017906159603));
#19112=CARTESIAN_POINT('Ctrl Pts',(-42.113822889283,-1.38567030932352,10.7137049327917));
#19113=CARTESIAN_POINT('Ctrl Pts',(-42.0800217201965,-1.20911028675503,
10.7529995432141));
#19114=CARTESIAN_POINT('Ctrl Pts',(-42.0461300361259,-0.795750669329885,
10.796977768321));
#19115=CARTESIAN_POINT('Ctrl Pts',(-42.0584163598968,-0.559888029352842,
10.7884683253291));
#19116=CARTESIAN_POINT('Ctrl Pts',(-42.1278479976902,-0.194142158176164,
10.7219357482004));
#19117=CARTESIAN_POINT('Ctrl Pts',(-42.1656814408185,-0.0597157582366805,
10.6844661413473));
#19118=CARTESIAN_POINT('Ctrl Pts',(-42.2599040956416,0.186267410922271,
10.5898537840786));
#19119=CARTESIAN_POINT('Ctrl Pts',(-42.3148062568321,0.297900855882757,
10.5342660162233));
#19120=CARTESIAN_POINT('Ctrl Pts',(-42.3779453595727,0.399648641330068,
10.4701702229062));
#19121=CARTESIAN_POINT('',(-43.4414564579485,-2.25607198756206,9.34999999998968));
#19122=CARTESIAN_POINT('Ctrl Pts',(-43.4414564579485,-2.25607198756207,
9.34999999998968));
#19123=CARTESIAN_POINT('Ctrl Pts',(-43.2405264867435,-2.19180199692552,
9.55399283494864));
#19124=CARTESIAN_POINT('Ctrl Pts',(-43.0384692598565,-2.13460442092698,
9.7586494941231));
#19125=CARTESIAN_POINT('Ctrl Pts',(-42.8353155147913,-2.08446078316056,
9.96399986478615));
#19126=CARTESIAN_POINT('Ctrl Pts',(-42.6758357073823,-2.04509701119951,
10.1252040678109));
#19127=CARTESIAN_POINT('Ctrl Pts',(-42.5156798721484,-2.01008129874976,
10.2868360245461));
#19128=CARTESIAN_POINT('Ctrl Pts',(-42.3548619717231,-1.97942721139887,
10.4489096280657));
#19129=CARTESIAN_POINT('',(-43.1481717937249,-5.52134683388194,9.34999999999062));
#19130=CARTESIAN_POINT('Origin',(0.,0.,9.34999999999998));
#19131=CARTESIAN_POINT('',(-42.0034749115207,-5.63542964579464,10.4701702229062));
#19132=CARTESIAN_POINT('Ctrl Pts',(-42.0034749115207,-5.63542964579464,
10.4701702229062));
#19133=CARTESIAN_POINT('Ctrl Pts',(-42.2104648788784,-5.62758774458413,
10.2660612053905));
#19134=CARTESIAN_POINT('Ctrl Pts',(-42.4175418687078,-5.61278982655376,
10.0627475751685));
#19135=CARTESIAN_POINT('Ctrl Pts',(-42.6246751679979,-5.59105439750503,
9.86020040449357));
#19136=CARTESIAN_POINT('Ctrl Pts',(-42.7991408439574,-5.57274692915372,
9.68959756484101));
#19137=CARTESIAN_POINT('Ctrl Pts',(-42.9736466844289,-5.54951680903796,
9.51953800447466));
#19138=CARTESIAN_POINT('Ctrl Pts',(-43.1481717937249,-5.52134683388194,
9.34999999999062));
#19139=CARTESIAN_POINT('',(-41.6420486840548,-7.98700482807827,10.4489096280657));
#19140=CARTESIAN_POINT('Ctrl Pts',(-41.6420486840548,-7.98700482807827,
10.4489096280657));
#19141=CARTESIAN_POINT('Ctrl Pts',(-41.5731662587823,-7.82301570651097,
10.547449245225));
#19142=CARTESIAN_POINT('Ctrl Pts',(-41.526239540548,-7.64031704551109,10.6271602259564));
#19143=CARTESIAN_POINT('Ctrl Pts',(-41.4764846370605,-7.22632801333186,
10.7492445866574));
#19144=CARTESIAN_POINT('Ctrl Pts',(-41.4810105474699,-6.99569328456079,
10.7838550844415));
#19145=CARTESIAN_POINT('Ctrl Pts',(-41.5511566965011,-6.53884015808524,
10.7881210903218));
#19146=CARTESIAN_POINT('Ctrl Pts',(-41.6161107996091,-6.31689994183735,
10.7577447440201));
#19147=CARTESIAN_POINT('Ctrl Pts',(-41.7881771403425,-5.9346381788992,10.6429386483201));
#19148=CARTESIAN_POINT('Ctrl Pts',(-41.8881138550115,-5.77289556463321,
10.5662273743849));
#19149=CARTESIAN_POINT('Ctrl Pts',(-42.0034749115207,-5.63542964579464,
10.4701702229062));
#19150=CARTESIAN_POINT('',(-42.6782125485707,-8.41547227788435,9.34999999999061));
#19151=CARTESIAN_POINT('Ctrl Pts',(-42.6782125485707,-8.41547227788435,
9.34999999999062));
#19152=CARTESIAN_POINT('Ctrl Pts',(-42.4884743280784,-8.32326114672641,
9.55399283494986));
#19153=CARTESIAN_POINT('Ctrl Pts',(-42.2966138161963,-8.23789001801298,
9.75864949412459));
#19154=CARTESIAN_POINT('Ctrl Pts',(-42.1026640670313,-8.15934497780424,
9.96399986478792));
#19155=CARTESIAN_POINT('Ctrl Pts',(-41.9504095829518,-8.09768552928488,
10.125204067812));
#19156=CARTESIAN_POINT('Ctrl Pts',(-41.7968671586498,-8.04023367450976,
10.2868360245467));
#19157=CARTESIAN_POINT('Ctrl Pts',(-41.6420486840548,-7.98700482807828,
10.4489096280657));
#19158=CARTESIAN_POINT('',(-41.9232160376754,-11.6057725748497,9.34999999999155));
#19159=CARTESIAN_POINT('Origin',(0.,0.,9.34999999999998));
#19160=CARTESIAN_POINT('',(-40.7739348422943,-11.5557868365701,10.4701702229111));
#19161=CARTESIAN_POINT('Ctrl Pts',(-40.7739348422943,-11.55578683657,10.4701702229111));
#19162=CARTESIAN_POINT('Ctrl Pts',(-40.9799339692222,-11.5774824983432,
10.2660612053103));
#19163=CARTESIAN_POINT('Ctrl Pts',(-41.1870091772698,-11.592305330102,10.0627475750051));
#19164=CARTESIAN_POINT('Ctrl Pts',(-41.395127432389,-11.600269278368,9.86020040424831));
#19165=CARTESIAN_POINT('Ctrl Pts',(-41.5704227236394,-11.6069772080976,
9.68959756467802));
#19166=CARTESIAN_POINT('Ctrl Pts',(-41.7464583369743,-11.6088183075708,
9.51953800439386));
#19167=CARTESIAN_POINT('Ctrl Pts',(-41.9232160376754,-11.6057725748497,
9.34999999999155));
#19168=CARTESIAN_POINT('',(-40.0815233709313,-13.831990059078,10.4489096280657));
#19169=CARTESIAN_POINT('Ctrl Pts',(-40.0815233709313,-13.831990059078,10.4489096280657));
#19170=CARTESIAN_POINT('Ctrl Pts',(-40.0366801547422,-13.659867119103,10.5474492452249));
#19171=CARTESIAN_POINT('Ctrl Pts',(-40.0162318132297,-13.4723496987262,
10.6271602259563));
#19172=CARTESIAN_POINT('Ctrl Pts',(-40.0259001250805,-13.0554936169285,
10.7492445866574));
#19173=CARTESIAN_POINT('Ctrl Pts',(-40.063202712373,-12.8278505213564,10.7838550844415));
#19174=CARTESIAN_POINT('Ctrl Pts',(-40.1976518535585,-12.3856303388355,
10.7881210903218));
#19175=CARTESIAN_POINT('Ctrl Pts',(-40.2935302035346,-12.1751930866566,
10.7577447440202));
#19176=CARTESIAN_POINT('Ctrl Pts',(-40.51824667799,-11.8213097907414,10.6429386483196));
#19177=CARTESIAN_POINT('Ctrl Pts',(-40.6401845549915,-11.6754359604617,
10.5662273743844));
#19178=CARTESIAN_POINT('Ctrl Pts',(-40.7739348422891,-11.5557868365682,
10.4701702229063));
#19179=CARTESIAN_POINT('',(-41.0461633055059,-14.4035578208467,9.34999999999155));
#19180=CARTESIAN_POINT('Ctrl Pts',(-41.0461633055059,-14.4035578208467,
9.34999999999155));
#19181=CARTESIAN_POINT('Ctrl Pts',(-40.8714793587379,-14.2852827018841,
9.55399283494871));
#19182=CARTESIAN_POINT('Ctrl Pts',(-40.6937212886046,-14.1734759304475,
9.75864949412134));
#19183=CARTESIAN_POINT('Ctrl Pts',(-40.51292379293,-14.0681284383109,9.96399986478255));
#19184=CARTESIAN_POINT('Ctrl Pts',(-40.3709940944081,-13.9854285217927,
10.1252040678084));
#19185=CARTESIAN_POINT('Ctrl Pts',(-40.2271907620149,-13.906710078777,10.2868360245449));
#19186=CARTESIAN_POINT('Ctrl Pts',(-40.0815233709313,-13.831990059078,10.4489096280657));
#19187=CARTESIAN_POINT('',(-39.8448244996705,-17.4539382544775,9.34999999999249));
#19188=CARTESIAN_POINT('Origin',(0.,0.,9.34999999999998));
#19189=CARTESIAN_POINT('',(-38.7143550419872,-17.2409015314864,10.4701702229062));
#19190=CARTESIAN_POINT('Ctrl Pts',(-38.7143550419872,-17.2409015314864,
10.4701702229062));
#19191=CARTESIAN_POINT('Ctrl Pts',(-38.9151697801539,-17.2916930951193,
10.2660612053907));
#19192=CARTESIAN_POINT('Ctrl Pts',(-39.1180277521749,-17.3358349265527,
10.0627475751689));
#19193=CARTESIAN_POINT('Ctrl Pts',(-39.3228942754451,-17.3733361291179,
9.86020040449417));
#19194=CARTESIAN_POINT('Ctrl Pts',(-39.4954506755326,-17.4049229028392,
9.68959756484204));
#19195=CARTESIAN_POINT('Ctrl Pts',(-39.6694324844552,-17.4317977424317,
9.51953800447611));
#19196=CARTESIAN_POINT('Ctrl Pts',(-39.8448244996705,-17.4539382544775,
9.34999999999249));
#19197=CARTESIAN_POINT('',(-37.7050538275441,-19.3953958606403,10.4489096280657));
#19198=CARTESIAN_POINT('Ctrl Pts',(-37.7050538275441,-19.3953958606403,
10.4489096280657));
#19199=CARTESIAN_POINT('Ctrl Pts',(-37.6851626990029,-19.2186430289538,
10.547449245225));
#19200=CARTESIAN_POINT('Ctrl Pts',(-37.6916090034773,-19.0301241631233,
10.6271602259564));
#19201=CARTESIAN_POINT('Ctrl Pts',(-37.7605037117183,-18.6188870194189,
10.7492445866574));
#19202=CARTESIAN_POINT('Ctrl Pts',(-37.8298236027884,-18.3988697140032,
10.7838550844415));
#19203=CARTESIAN_POINT('Ctrl Pts',(-38.025838739333,-17.9802848030953,10.7881210903218));
#19204=CARTESIAN_POINT('Ctrl Pts',(-38.150689529462,-17.7856344105889,10.7577447440201));
#19205=CARTESIAN_POINT('Ctrl Pts',(-38.4234815582465,-17.4673336250894,
10.6429386483201));
#19206=CARTESIAN_POINT('Ctrl Pts',(-38.564938294045,-17.3402981493132,10.5662273743849));
#19207=CARTESIAN_POINT('Ctrl Pts',(-38.7143550419872,-17.2409015314864,
10.4701702229062));
#19208=CARTESIAN_POINT('',(-38.5785325449017,-20.0984284630072,9.34999999999249));
#19209=CARTESIAN_POINT('Ctrl Pts',(-38.5785325449017,-20.0984284630072,
9.34999999999249));
#19210=CARTESIAN_POINT('Ctrl Pts',(-38.4224589332633,-19.956497096582,9.55399283495215));
#19211=CARTESIAN_POINT('Ctrl Pts',(-38.2624219465708,-19.8205307458622,
9.75864949412731));
#19212=CARTESIAN_POINT('Ctrl Pts',(-38.0984572200175,-19.6905253729384,
9.96399986479107));
#19213=CARTESIAN_POINT('Ctrl Pts',(-37.9697415864275,-19.5884685202376,
10.1252040678142));
#19214=CARTESIAN_POINT('Ctrl Pts',(-37.8386047670999,-19.4900859694782,
10.2868360245478));
#19215=CARTESIAN_POINT('Ctrl Pts',(-37.7050538275441,-19.3953958606403,
10.4489096280657));
#19216=CARTESIAN_POINT('',(-36.9553072378377,-22.9467920842455,9.34999999999342));
#19217=CARTESIAN_POINT('Origin',(0.,0.,9.34999999999998));
#19218=CARTESIAN_POINT('',(-35.866662616011,-22.575041189878,10.4701702229062));
#19219=CARTESIAN_POINT('Ctrl Pts',(-35.866662616011,-22.575041189878,10.4701702229062));
#19220=CARTESIAN_POINT('Ctrl Pts',(-36.0582049565313,-22.6538946856141,
10.2660612053895));
#19221=CARTESIAN_POINT('Ctrl Pts',(-36.2527160892939,-22.7264569163318,
10.0627475751663));
#19222=CARTESIAN_POINT('Ctrl Pts',(-36.4501603891734,-22.7927319568543,
9.86020040449035));
#19223=CARTESIAN_POINT('Ctrl Pts',(-36.6164651473186,-22.8485545589344,
9.68959756483981));
#19224=CARTESIAN_POINT('Ctrl Pts',(-36.7848513838357,-22.8999160444089,
9.51953800447548));
#19225=CARTESIAN_POINT('Ctrl Pts',(-36.9553072378377,-22.9467920842455,
9.34999999999343));
#19226=CARTESIAN_POINT('',(-34.5610181206245,-24.5639673341829,10.4489096280657));
#19227=CARTESIAN_POINT('Ctrl Pts',(-34.5610181206245,-24.5639673341829,
10.4489096280657));
#19228=CARTESIAN_POINT('Ctrl Pts',(-34.5664840057471,-24.386182788725,10.547449245225));
#19229=CARTESIAN_POINT('Ctrl Pts',(-34.5996937280388,-24.2005001779056,
10.6271602259564));
#19230=CARTESIAN_POINT('Ctrl Pts',(-34.7264123350862,-23.8032535746304,
10.7492445866574));
#19231=CARTESIAN_POINT('Ctrl Pts',(-34.8263383768538,-23.5953409772319,
10.7838550844415));
#19232=CARTESIAN_POINT('Ctrl Pts',(-35.0799292058383,-23.2089125196238,
10.7881210903218));
#19233=CARTESIAN_POINT('Ctrl Pts',(-35.2312108340732,-23.034011507456,10.7577447440201));
#19234=CARTESIAN_POINT('Ctrl Pts',(-35.5465251581488,-22.7577729184597,
10.6429386483201));
#19235=CARTESIAN_POINT('Ctrl Pts',(-35.7046211015307,-22.6521618731347,
10.5662273743849));
#19236=CARTESIAN_POINT('Ctrl Pts',(-35.866662616011,-22.575041189878,10.4701702229062));
#19237=CARTESIAN_POINT('',(-35.3255541129844,-25.3841530607422,9.34999999999342));
#19238=CARTESIAN_POINT('Ctrl Pts',(-35.3255541129844,-25.3841530607421,
9.34999999999342));
#19239=CARTESIAN_POINT('Ctrl Pts',(-35.1912680451325,-25.2214547601811,
9.55399283495167));
#19240=CARTESIAN_POINT('Ctrl Pts',(-35.0522100334246,-25.0640967129866,
9.7586494941254));
#19241=CARTESIAN_POINT('Ctrl Pts',(-34.9084159249933,-24.912079993766,9.96399986478771));
#19242=CARTESIAN_POINT('Ctrl Pts',(-34.7955346354467,-24.7927437880933,
10.1252040678119));
#19243=CARTESIAN_POINT('Ctrl Pts',(-34.6797338966557,-24.6766999146096,
10.2868360245467));
#19244=CARTESIAN_POINT('Ctrl Pts',(-34.5610181206245,-24.5639673341829,
10.4489096280657));
#19245=CARTESIAN_POINT('',(-33.3134864909484,-27.9725154002619,9.34999999999436));
#19246=CARTESIAN_POINT('Origin',(0.,0.,9.34999999999998));
#19247=CARTESIAN_POINT('',(-32.2888283700867,-27.4496181106866,10.4701702229062));
#19248=CARTESIAN_POINT('Ctrl Pts',(-32.2888283700867,-27.4496181106866,
10.4701702229062));
#19249=CARTESIAN_POINT('Ctrl Pts',(-32.4671990632674,-27.5549283087462,
10.266061205391));
#19250=CARTESIAN_POINT('Ctrl Pts',(-32.6494036710296,-27.6544337809821,
10.0627475751695));
#19251=CARTESIAN_POINT('Ctrl Pts',(-32.8354063509525,-27.7481334907575,
9.86020040449504));
#19252=CARTESIAN_POINT('Ctrl Pts',(-32.9920739818655,-27.8270555339981,
9.68959756484325));
#19253=CARTESIAN_POINT('Ctrl Pts',(-33.1514367877901,-27.9018580936256,
9.51953800447765));
#19254=CARTESIAN_POINT('Ctrl Pts',(-33.3134864909484,-27.9725154002619,
9.34999999999436));
#19255=CARTESIAN_POINT('',(-30.7134197505151,-29.2324872694338,10.4489096280657));
#19256=CARTESIAN_POINT('Ctrl Pts',(-30.7134197505151,-29.2324872694338,
10.4489096280657));
#19257=CARTESIAN_POINT('Ctrl Pts',(-30.7441313796426,-29.0572901908618,
10.547449245225));
#19258=CARTESIAN_POINT('Ctrl Pts',(-30.8034284655748,-28.8782237975454,
10.6271602259564));
#19259=CARTESIAN_POINT('Ctrl Pts',(-30.9853913460153,-28.5030545299773,
10.7492445866574));
#19260=CARTESIAN_POINT('Ctrl Pts',(-31.1138893324329,-28.3114791415085,
10.7838550844415));
#19261=CARTESIAN_POINT('Ctrl Pts',(-31.4198934758748,-27.9650737062297,
10.7881210903218));
#19262=CARTESIAN_POINT('Ctrl Pts',(-31.5945262845248,-27.8134825546352,
10.7577447440201));
#19263=CARTESIAN_POINT('Ctrl Pts',(-31.945944013545,-27.5849295832079,10.6429386483201));
#19264=CARTESIAN_POINT('Ctrl Pts',(-32.1174607870141,-27.5028929046598,
10.5662273743849));
#19265=CARTESIAN_POINT('Ctrl Pts',(-32.2888283700867,-27.4496181106866,
10.4701702229062));
#19266=CARTESIAN_POINT('',(-31.3534492698128,-30.1531295040128,9.34999999999437));
#19267=CARTESIAN_POINT('Ctrl Pts',(-31.3534492698128,-30.1531295040128,
9.34999999999436));
#19268=CARTESIAN_POINT('Ctrl Pts',(-31.2436844228208,-29.9729763375018,
9.55399283498594));
#19269=CARTESIAN_POINT('Ctrl Pts',(-31.1284362061847,-29.7974299498614,
9.7586494941933));
#19270=CARTESIAN_POINT('Ctrl Pts',(-31.0077399492325,-29.6264965063399,
9.96399986488942));
#19271=CARTESIAN_POINT('Ctrl Pts',(-30.912990941281,-29.4923102887359,10.1252040678799));
#19272=CARTESIAN_POINT('Ctrl Pts',(-30.8148836521473,-29.360967411178,10.2868360245808));
#19273=CARTESIAN_POINT('Ctrl Pts',(-30.7134197505151,-29.2324872694338,
10.4489096280657));
#19274=CARTESIAN_POINT('',(-28.9934992272654,-32.428798968802,9.34999999999529));
#19275=CARTESIAN_POINT('Origin',(0.,0.,9.34999999999998));
#19276=CARTESIAN_POINT('',(-28.0536866918425,-31.7653999649279,10.4701702229111));
#19277=CARTESIAN_POINT('Ctrl Pts',(-28.0536866918425,-31.7653999649279,
10.4701702229111));
#19278=CARTESIAN_POINT('Ctrl Pts',(-28.2152546248138,-31.8950230534185,
10.2660612053112));
#19279=CARTESIAN_POINT('Ctrl Pts',(-28.3814435472657,-32.0194461227552,
10.0627475750071));
#19280=CARTESIAN_POINT('Ctrl Pts',(-28.5522181291298,-32.1386630459438,
9.86020040425125));
#19281=CARTESIAN_POINT('Ctrl Pts',(-28.6960593315701,-32.2390779050844,
9.68959756468124));
#19282=CARTESIAN_POINT('Ctrl Pts',(-28.8431545396677,-32.3357987744151,
9.51953800439734));
#19283=CARTESIAN_POINT('Ctrl Pts',(-28.9934992272654,-32.4287989688019,
9.34999999999529));
#19284=CARTESIAN_POINT('',(-26.2405847244738,-33.3059180634111,10.4489096280657));
#19285=CARTESIAN_POINT('Ctrl Pts',(-26.2405847244738,-33.3059180634111,
10.4489096280657));
#19286=CARTESIAN_POINT('Ctrl Pts',(-26.2959168974022,-33.136874959018,10.5474492452249));
#19287=CARTESIAN_POINT('Ctrl Pts',(-26.3800942293039,-32.9680700585877,
10.6271602259563));
#19288=CARTESIAN_POINT('Ctrl Pts',(-26.6135971436294,-32.6226154911157,
10.7492445866574));
#19289=CARTESIAN_POINT('Ctrl Pts',(-26.7680512262512,-32.4512772340281,
10.7838550844415));
#19290=CARTESIAN_POINT('Ctrl Pts',(-27.120239322233,-32.1519466367898,10.7881210903218));
#19291=CARTESIAN_POINT('Ctrl Pts',(-27.3146682909135,-32.0267513044625,
10.7577447440202));
#19292=CARTESIAN_POINT('Ctrl Pts',(-27.6950355733221,-31.8505366300091,
10.6429386483196));
#19293=CARTESIAN_POINT('Ctrl Pts',(-27.8764815899833,-31.7937443484396,
10.5662273743844));
#19294=CARTESIAN_POINT('Ctrl Pts',(-28.0536866918392,-31.7653999649236,
10.4701702229063));
#19295=CARTESIAN_POINT('',(-26.7430786153894,-34.3082751850266,9.34999999999529));
#19296=CARTESIAN_POINT('Ctrl Pts',(-26.7430786153894,-34.3082751850266,
9.3499999999953));
#19297=CARTESIAN_POINT('Ctrl Pts',(-26.6600694850412,-34.1143345515736,
9.55399283495525));
#19298=CARTESIAN_POINT('Ctrl Pts',(-26.5709771848575,-33.9241734417595,
9.7586494941307));
#19299=CARTESIAN_POINT('Ctrl Pts',(-26.4758358071583,-33.7378029859668,
9.96399986479476));
#19300=CARTESIAN_POINT('Ctrl Pts',(-26.4011478973347,-33.5914984008048,
10.1252040678166));
#19301=CARTESIAN_POINT('Ctrl Pts',(-26.3227312393088,-33.4475302813445,
10.286836024549));
#19302=CARTESIAN_POINT('Ctrl Pts',(-26.2405847244738,-33.3059180634111,
10.4489096280657));
#19303=CARTESIAN_POINT('',(-24.0832879296629,-36.2249257072707,9.34999999999623));
#19304=CARTESIAN_POINT('Origin',(0.,0.,9.34999999999998));
#19305=CARTESIAN_POINT('',(-23.2474528526981,-35.4345298797237,10.4701702229062));
#19306=CARTESIAN_POINT('Ctrl Pts',(-23.2474528526981,-35.4345298797237,
10.4701702229062));
#19307=CARTESIAN_POINT('Ctrl Pts',(-23.3889289681449,-35.5858271062694,
10.2660612053881));
#19308=CARTESIAN_POINT('Ctrl Pts',(-23.5357190779423,-35.732634877731,10.0627475751637));
#19309=CARTESIAN_POINT('Ctrl Pts',(-23.6877890835939,-35.8749421014862,
9.86020040448638));
#19310=CARTESIAN_POINT('Ctrl Pts',(-23.8158756656119,-35.9948056196677,
9.68959756483812));
#19311=CARTESIAN_POINT('Ctrl Pts',(-23.9477088417672,-36.1114758408148,
9.51953800447604));
#19312=CARTESIAN_POINT('Ctrl Pts',(-24.0832879296629,-36.2249257072707,
9.34999999999623));
#19313=CARTESIAN_POINT('',(-21.2335670650398,-36.7013364119537,10.4489096280657));
#19314=CARTESIAN_POINT('Ctrl Pts',(-21.2335670650398,-36.7013364119537,
10.4489096280657));
#19315=CARTESIAN_POINT('Ctrl Pts',(-21.3123933782931,-36.5418885118649,
10.547449245225));
#19316=CARTESIAN_POINT('Ctrl Pts',(-21.4197373484343,-36.3867814853002,
10.6271602259564));
#19317=CARTESIAN_POINT('Ctrl Pts',(-21.7000268506759,-36.0780740767093,
10.7492445866574));
#19318=CARTESIAN_POINT('Ctrl Pts',(-21.8772927897884,-35.9304609038185,
10.7838550844415));
#19319=CARTESIAN_POINT('Ctrl Pts',(-22.2684953043027,-35.6842986523824,
10.7881210903218));
#19320=CARTESIAN_POINT('Ctrl Pts',(-22.4787624198982,-35.5880477552548,
10.7577447440201));
#19321=CARTESIAN_POINT('Ctrl Pts',(-22.8803360747106,-35.4677586003878,
10.6429386483201));
#19322=CARTESIAN_POINT('Ctrl Pts',(-23.0680176169133,-35.4373668428729,
10.5662273743849));
#19323=CARTESIAN_POINT('Ctrl Pts',(-23.2474528526981,-35.4345298797237,
10.4701702229062));
#19324=CARTESIAN_POINT('',(-21.5882960010271,-37.7650033201689,9.34999999999623));
#19325=CARTESIAN_POINT('Ctrl Pts',(-21.5882960010271,-37.7650033201689,
9.34999999999623));
#19326=CARTESIAN_POINT('Ctrl Pts',(-21.5337324138217,-37.5612232917665,
9.55399283495411));
#19327=CARTESIAN_POINT('Ctrl Pts',(-21.4726096923831,-37.3603185915706,
9.75864949412748));
#19328=CARTESIAN_POINT('Ctrl Pts',(-21.4049599980022,-37.1623050885155,
9.96399986478943));
#19329=CARTESIAN_POINT('Ctrl Pts',(-21.351853616785,-37.0068604752673,10.125204067813));
#19330=CARTESIAN_POINT('Ctrl Pts',(-21.2947239269072,-36.8531978896717,
10.2868360245472));
#19331=CARTESIAN_POINT('Ctrl Pts',(-21.2335670650398,-36.7013364119537,
10.4489096280657));
#19332=CARTESIAN_POINT('',(-18.6828103402799,-39.2836174223986,9.34999999999716));
#19333=CARTESIAN_POINT('Origin',(0.,0.,9.34999999999998));
#19334=CARTESIAN_POINT('',(-17.9679679135938,-38.3823149509186,10.4701702229062));
#19335=CARTESIAN_POINT('Ctrl Pts',(-17.9679679135938,-38.3823149509186,
10.4701702229062));
#19336=CARTESIAN_POINT('Ctrl Pts',(-18.0864721658495,-38.5522063403393,
10.2660612053891));
#19337=CARTESIAN_POINT('Ctrl Pts',(-18.2108752397297,-38.7184102311019,
10.0627475751655));
#19338=CARTESIAN_POINT('Ctrl Pts',(-18.341144962456,-38.8809107907692,9.86020040448914));
#19339=CARTESIAN_POINT('Ctrl Pts',(-18.4508694505502,-39.0177828923699,
9.68959756484026));
#19340=CARTESIAN_POINT('Ctrl Pts',(-18.5647568514065,-39.1520273960344,
9.51953800447757));
#19341=CARTESIAN_POINT('Ctrl Pts',(-18.6828103402799,-39.2836174223986,
9.34999999999716));
#19342=CARTESIAN_POINT('',(-15.7942952127126,-39.3496213890633,10.4489096280657));
#19343=CARTESIAN_POINT('Ctrl Pts',(-15.7942952127126,-39.3496213890633,
10.4489096280657));
#19344=CARTESIAN_POINT('Ctrl Pts',(-15.8950109898693,-39.2030145927148,
10.547449245225));
#19345=CARTESIAN_POINT('Ctrl Pts',(-16.0233363845722,-39.064762971785,10.6271602259564));
#19346=CARTESIAN_POINT('Ctrl Pts',(-16.3447065887524,-38.7990871146754,
10.7492445866574));
#19347=CARTESIAN_POINT('Ctrl Pts',(-16.5411757610281,-38.6782040045002,
10.7838550844415));
#19348=CARTESIAN_POINT('Ctrl Pts',(-16.9634289390143,-38.4902212524323,
10.7881210903218));
#19349=CARTESIAN_POINT('Ctrl Pts',(-17.1852537694115,-38.4248741812053,
10.7577447440201));
#19350=CARTESIAN_POINT('Ctrl Pts',(-17.5998589150602,-38.3629592862316,
10.6429386483201));
#19351=CARTESIAN_POINT('Ctrl Pts',(-17.7899553278333,-38.3595867413123,
10.5662273743849));
#19352=CARTESIAN_POINT('Ctrl Pts',(-17.9679679135938,-38.3823149509187,
10.4701702229062));
#19353=CARTESIAN_POINT('',(-15.994037935589,-40.4529448929888,9.34999999999716));
#19354=CARTESIAN_POINT('Ctrl Pts',(-15.994037935589,-40.4529448929888,9.34999999999716));
#19355=CARTESIAN_POINT('Ctrl Pts',(-15.9690306488124,-40.2434738433598,
9.55399283495553));
#19356=CARTESIAN_POINT('Ctrl Pts',(-15.937121788463,-40.0359153931143,9.75864949412937));
#19357=CARTESIAN_POINT('Ctrl Pts',(-15.8983409300912,-39.8302898266929,
9.9639998647918));
#19358=CARTESIAN_POINT('Ctrl Pts',(-15.8678971702567,-39.6688695894216,
10.1252040678146));
#19359=CARTESIAN_POINT('Ctrl Pts',(-15.8332174442655,-39.5086406648094,
10.286836024548));
#19360=CARTESIAN_POINT('Ctrl Pts',(-15.7942952127126,-39.3496213890633,
10.4489096280657));
#19361=CARTESIAN_POINT('',(-12.902004609145,-41.5426079714041,9.3499999999981));
#19362=CARTESIAN_POINT('Origin',(0.,0.,9.34999999999998));
#19363=CARTESIAN_POINT('',(-12.3227069631095,-40.5487467751691,10.4701702229062));
#19364=CARTESIAN_POINT('Ctrl Pts',(-12.3227069631095,-40.5487467751691,
10.4701702229062));
#19365=CARTESIAN_POINT('Ctrl Pts',(-12.4158269473359,-40.7337738287013,
10.266061205391));
#19366=CARTESIAN_POINT('Ctrl Pts',(-12.5153104974631,-40.9159904068405,
10.0627475751694));
#19367=CARTESIAN_POINT('Ctrl Pts',(-12.6211280213761,-41.0953762596368,
9.86020040449486));
#19368=CARTESIAN_POINT('Ctrl Pts',(-12.7102567413884,-41.2464706233757,
9.68959756484438));
#19369=CARTESIAN_POINT('Ctrl Pts',(-12.8038799478888,-41.3955565785931,
9.5195380044801));
#19370=CARTESIAN_POINT('Ctrl Pts',(-12.902004609145,-41.5426079714041,9.3499999999981));
#19371=CARTESIAN_POINT('',(-10.0334970568407,-41.1968615496291,10.4489096280657));
#19372=CARTESIAN_POINT('Ctrl Pts',(-10.0334970568407,-41.1968615496291,
10.4489096280657));
#19373=CARTESIAN_POINT('Ctrl Pts',(-10.1540520151182,-41.0660803486156,
10.547449245225));
#19374=CARTESIAN_POINT('Ctrl Pts',(-10.3007464994067,-40.9474985376379,
10.6271602259564));
#19375=CARTESIAN_POINT('Ctrl Pts',(-10.6566552349236,-40.7302626263145,
10.7492445866574));
#19376=CARTESIAN_POINT('Ctrl Pts',(-10.8683280945852,-40.6385704103799,
10.7838550844415));
#19377=CARTESIAN_POINT('Ctrl Pts',(-11.313036079017,-40.5125939444148,10.7881210903218));
#19378=CARTESIAN_POINT('Ctrl Pts',(-11.5419029103591,-40.4794809770132,
10.7577447440201));
#19379=CARTESIAN_POINT('Ctrl Pts',(-11.9610993817012,-40.4772007506467,
10.6429386483201));
#19380=CARTESIAN_POINT('Ctrl Pts',(-12.1497408502734,-40.5009160736121,
10.5662273743849));
#19381=CARTESIAN_POINT('Ctrl Pts',(-12.3227069631095,-40.5487467751691,
10.4701702229062));
#19382=CARTESIAN_POINT('',(-10.0741873807793,-42.3173811644473,9.3499999999981));
#19383=CARTESIAN_POINT('Ctrl Pts',(-10.0741873807793,-42.3173811644473,
9.3499999999981));
#19384=CARTESIAN_POINT('Ctrl Pts',(-10.0792454706754,-42.1064833200987,
9.55399283495567));
#19385=CARTESIAN_POINT('Ctrl Pts',(-10.0772000437945,-41.8964964113029,
9.75864949412871));
#19386=CARTESIAN_POINT('Ctrl Pts',(-10.0680774878737,-41.6874447250736,
9.96399986479033));
#19387=CARTESIAN_POINT('Ctrl Pts',(-10.0609160965793,-41.5233349143112,
10.1252040678136));
#19388=CARTESIAN_POINT('Ctrl Pts',(-10.0493923136875,-41.3598014495242,
10.2868360245475));
#19389=CARTESIAN_POINT('Ctrl Pts',(-10.0334970568407,-41.1968615496291,
10.4489096280657));
#19390=CARTESIAN_POINT('',(-6.8585512704771,-42.9559108211003,9.34999999999904));
#19391=CARTESIAN_POINT('Origin',(0.,0.,9.34999999999998));
#19392=CARTESIAN_POINT('',(-6.42659123460866,-41.8897230480067,10.4701702229062));
#19393=CARTESIAN_POINT('Ctrl Pts',(-6.42659123460866,-41.8897230480067,
10.4701702229062));
#19394=CARTESIAN_POINT('Ctrl Pts',(-6.49243129646439,-42.0861191484173,
10.2660612053897));
#19395=CARTESIAN_POINT('Ctrl Pts',(-6.56497012464666,-42.2806390098741,
10.0627475751668));
#19396=CARTESIAN_POINT('Ctrl Pts',(-6.64418131011379,-42.4732583771454,
9.86020040449103));
#19397=CARTESIAN_POINT('Ctrl Pts',(-6.7108998583293,-42.635499157494,9.68959756484215));
#19398=CARTESIAN_POINT('Ctrl Pts',(-6.7823529719748,-42.7963916041418,9.51953800447945));
#19399=CARTESIAN_POINT('Ctrl Pts',(-6.85855127047709,-42.9559108211003,
9.34999999999904));
#19400=CARTESIAN_POINT('',(-4.06844583510776,-42.2054524109828,10.4489096280657));
#19401=CARTESIAN_POINT('Ctrl Pts',(-4.06844583510776,-42.2054524109828,
10.4489096280657));
#19402=CARTESIAN_POINT('Ctrl Pts',(-4.20638582320732,-42.093159133415,10.547449245225));
#19403=CARTESIAN_POINT('Ctrl Pts',(-4.36846312041316,-41.9966611160993,
10.6271602259564));
#19404=CARTESIAN_POINT('Ctrl Pts',(-4.75166511176766,-41.8322874472601,
10.7492445866574));
#19405=CARTESIAN_POINT('Ctrl Pts',(-4.97423260980666,-41.7716527146639,
10.7838550844415));
#19406=CARTESIAN_POINT('Ctrl Pts',(-5.4323424285529,-41.7102470523626,10.7881210903217));
#19407=CARTESIAN_POINT('Ctrl Pts',(-5.66359219215121,-41.7100422733127,
10.7577447440201));
#19408=CARTESIAN_POINT('Ctrl Pts',(-6.078846357893,-41.7674431343866,10.6429386483201));
#19409=CARTESIAN_POINT('Ctrl Pts',(-6.26219268596132,-41.8177635496503,
10.5662273743849));
#19410=CARTESIAN_POINT('Ctrl Pts',(-6.42659123460866,-41.8897230480067,
10.4701702229062));
#19411=CARTESIAN_POINT('',(-3.9492554224545,-43.3203575886476,9.34999999999904));
#19412=CARTESIAN_POINT('Ctrl Pts',(-3.9492554224545,-43.3203575886476,9.34999999999904));
#19413=CARTESIAN_POINT('Ctrl Pts',(-3.98427592089977,-43.1123262215076,
9.5539928349595));
#19414=CARTESIAN_POINT('Ctrl Pts',(-4.01213556648031,-42.9041855820685,
9.75864949413545));
#19415=CARTESIAN_POINT('Ctrl Pts',(-4.03285702194169,-42.6959634655039,
9.96399986480001));
#19416=CARTESIAN_POINT('Ctrl Pts',(-4.04912378446205,-42.5325048837476,
10.1252040678201));
#19417=CARTESIAN_POINT('Ctrl Pts',(-4.06099053565725,-42.3689959485411,
10.2868360245508));
#19418=CARTESIAN_POINT('Ctrl Pts',(-4.06844583510776,-42.2054524109828,
10.4489096280657));
#19419=CARTESIAN_POINT('',(-0.675477606371088,-43.4947552010963,9.34999999999998));
#19420=CARTESIAN_POINT('Origin',(0.,0.,9.34999999999998));
#19421=CARTESIAN_POINT('',(-0.399648641329914,-42.3779453595728,10.4701702229062));
#19422=CARTESIAN_POINT('Ctrl Pts',(-0.399648641329913,-42.3779453595728,
10.4701702229062));
#19423=CARTESIAN_POINT('Ctrl Pts',(-0.436868467022045,-42.581712448616,
10.2660612053897));
#19424=CARTESIAN_POINT('Ctrl Pts',(-0.48098589190162,-42.7845757299589,
10.0627475751667));
#19425=CARTESIAN_POINT('Ctrl Pts',(-0.53197822761229,-42.9865074368548,
9.86020040449092));
#19426=CARTESIAN_POINT('Ctrl Pts',(-0.57492840679043,-43.1565918793901,
9.68959756484239));
#19427=CARTESIAN_POINT('Ctrl Pts',(-0.622756848241735,-43.326015511231,
9.51953800448004));
#19428=CARTESIAN_POINT('Ctrl Pts',(-0.675477606371083,-43.4947552010963,
9.34999999999997));
#19429=CARTESIAN_POINT('',(1.97942721139903,-42.3548619717231,10.4489096280657));
#19430=CARTESIAN_POINT('Ctrl Pts',(1.97942721139902,-42.3548619717231,10.4489096280657));
#19431=CARTESIAN_POINT('Ctrl Pts',(1.82691025384907,-42.2633425849052,10.5474492452249));
#19432=CARTESIAN_POINT('Ctrl Pts',(1.65274957010464,-42.1908927826067,10.6271602259564));
#19433=CARTESIAN_POINT('Ctrl Pts',(1.25005521039315,-42.0827275301346,10.7492445866574));
#19434=CARTESIAN_POINT('Ctrl Pts',(1.02112390640523,-42.0543846291766,10.7838550844415));
#19435=CARTESIAN_POINT('Ctrl Pts',(0.558938048174549,-42.0587998127441,
10.7881210903218));
#19436=CARTESIAN_POINT('Ctrl Pts',(0.330012930637701,-42.0915073907569,
10.7577447440201));
#19437=CARTESIAN_POINT('Ctrl Pts',(-0.0728455521833925,-42.2074208232701,
10.6429386483201));
#19438=CARTESIAN_POINT('Ctrl Pts',(-0.247164337235464,-42.2833219522895,
10.5662273743849));
#19439=CARTESIAN_POINT('Ctrl Pts',(-0.399648641329906,-42.3779453595728,
10.4701702229062));
#19440=CARTESIAN_POINT('',(2.25607198755898,-43.4414564579384,9.34999999999998));
#19441=CARTESIAN_POINT('Ctrl Pts',(2.25607198755898,-43.4414564579384,9.34999999999998));
#19442=CARTESIAN_POINT('Ctrl Pts',(2.19180199691216,-43.2405264867004,9.55399283499235));
#19443=CARTESIAN_POINT('Ctrl Pts',(2.13460442090562,-43.0384692597801,9.75864949420051));
#19444=CARTESIAN_POINT('Ctrl Pts',(2.08446078313353,-42.8353155146812,9.96399986489744));
#19445=CARTESIAN_POINT('Ctrl Pts',(2.04509701118354,-42.6758357073085,10.1252040678853));
#19446=CARTESIAN_POINT('Ctrl Pts',(2.01008129874285,-42.5156798721113,10.2868360245835));
#19447=CARTESIAN_POINT('Ctrl Pts',(1.97942721139903,-42.3548619717231,10.4489096280657));
#19448=CARTESIAN_POINT('',(5.52134683388117,-43.148171793727,9.34999999998873));
#19449=CARTESIAN_POINT('Origin',(0.,0.,9.34999999999998));
#19450=CARTESIAN_POINT('',(5.63542964579419,-42.0034749115208,10.4701702229062));
#19451=CARTESIAN_POINT('Ctrl Pts',(5.6354296457942,-42.0034749115208,10.4701702229062));
#19452=CARTESIAN_POINT('Ctrl Pts',(5.62758774458367,-42.2104648788786,10.2660612053904));
#19453=CARTESIAN_POINT('Ctrl Pts',(5.61278982655329,-42.4175418687082,10.0627475751682));
#19454=CARTESIAN_POINT('Ctrl Pts',(5.59105439750453,-42.6246751679985,9.86020040449308));
#19455=CARTESIAN_POINT('Ctrl Pts',(5.57274692915316,-42.7991408439585,9.68959756484005));
#19456=CARTESIAN_POINT('Ctrl Pts',(5.54951680903731,-42.9736466844305,9.51953800447324));
#19457=CARTESIAN_POINT('Ctrl Pts',(5.52134683388117,-43.148171793727,9.34999999998873));
#19458=CARTESIAN_POINT('',(7.98700482807783,-41.6420486840549,10.4489096280657));
#19459=CARTESIAN_POINT('Ctrl Pts',(7.98700482807783,-41.6420486840549,10.4489096280657));
#19460=CARTESIAN_POINT('Ctrl Pts',(7.82301570651054,-41.5731662587824,10.547449245225));
#19461=CARTESIAN_POINT('Ctrl Pts',(7.64031704551066,-41.5262395405481,10.6271602259564));
#19462=CARTESIAN_POINT('Ctrl Pts',(7.22632801333144,-41.4764846370606,10.7492445866574));
#19463=CARTESIAN_POINT('Ctrl Pts',(6.99569328456037,-41.4810105474699,10.7838550844415));
#19464=CARTESIAN_POINT('Ctrl Pts',(6.53884015808481,-41.5511566965012,10.7881210903218));
#19465=CARTESIAN_POINT('Ctrl Pts',(6.31689994183693,-41.6161107996092,10.7577447440201));
#19466=CARTESIAN_POINT('Ctrl Pts',(5.93463817889873,-41.7881771403425,10.6429386483201));
#19467=CARTESIAN_POINT('Ctrl Pts',(5.77289556463275,-41.8881138550116,10.5662273743849));
#19468=CARTESIAN_POINT('Ctrl Pts',(5.63542964579419,-42.0034749115208,10.4701702229062));
#19469=CARTESIAN_POINT('',(8.41547227788475,-42.6782125485726,9.34999999998873));
#19470=CARTESIAN_POINT('Ctrl Pts',(8.41547227788475,-42.6782125485725,9.34999999998873));
#19471=CARTESIAN_POINT('Ctrl Pts',(8.32326114671144,-42.4884743280488,9.55399283498187));
#19472=CARTESIAN_POINT('Ctrl Pts',(8.23789001798488,-42.2966138161343,9.75864949419081));
#19473=CARTESIAN_POINT('Ctrl Pts',(8.15934497776531,-42.1026640669364,9.96399986488852));
#19474=CARTESIAN_POINT('Ctrl Pts',(8.09768552926051,-41.950409582888,10.1252040678793));
#19475=CARTESIAN_POINT('Ctrl Pts',(8.04023367449823,-41.7968671586176,10.2868360245805));
#19476=CARTESIAN_POINT('Ctrl Pts',(7.98700482807784,-41.642048684055,10.4489096280657));
#19477=CARTESIAN_POINT('',(11.6057725748491,-41.9232160376785,9.34999999998873));
#19478=CARTESIAN_POINT('Origin',(0.,0.,9.34999999999998));
#19479=CARTESIAN_POINT('',(11.5557868365676,-40.7739348422894,10.4701702229062));
#19480=CARTESIAN_POINT('Ctrl Pts',(11.5557868365676,-40.7739348422894,10.4701702229062));
#19481=CARTESIAN_POINT('Ctrl Pts',(11.577482498333,-40.9799339691365,10.2660612053909));
#19482=CARTESIAN_POINT('Ctrl Pts',(11.592305330089,-41.1870091771008,10.0627475751691));
#19483=CARTESIAN_POINT('Ctrl Pts',(11.6002692783576,-41.3951274321352,9.8602004044945));
#19484=CARTESIAN_POINT('Ctrl Pts',(11.6069772080954,-41.5704227234707,9.689597564841));
#19485=CARTESIAN_POINT('Ctrl Pts',(11.6088183075718,-41.7464583368912,9.51953800447371));
#19486=CARTESIAN_POINT('Ctrl Pts',(11.6057725748491,-41.9232160376785,9.34999999998873));
#19487=CARTESIAN_POINT('',(13.8319900590775,-40.0815233709314,10.4489096280657));
#19488=CARTESIAN_POINT('Ctrl Pts',(13.8319900590775,-40.0815233709314,10.4489096280657));
#19489=CARTESIAN_POINT('Ctrl Pts',(13.6598671191025,-40.0366801547423,10.547449245225));
#19490=CARTESIAN_POINT('Ctrl Pts',(13.4723496987256,-40.0162318132298,10.6271602259564));
#19491=CARTESIAN_POINT('Ctrl Pts',(13.0554936169279,-40.0259001250807,10.7492445866574));
#19492=CARTESIAN_POINT('Ctrl Pts',(12.8278505213559,-40.0632027123732,10.7838550844415));
#19493=CARTESIAN_POINT('Ctrl Pts',(12.385630338835,-40.1976518535586,10.7881210903218));
#19494=CARTESIAN_POINT('Ctrl Pts',(12.1751930866561,-40.2935302035348,10.7577447440201));
#19495=CARTESIAN_POINT('Ctrl Pts',(11.8213097907425,-40.5182466779892,10.6429386483201));
#19496=CARTESIAN_POINT('Ctrl Pts',(11.6754359604618,-40.640184554991,10.5662273743849));
#19497=CARTESIAN_POINT('Ctrl Pts',(11.5557868365676,-40.7739348422894,10.4701702229062));
#19498=CARTESIAN_POINT('',(14.4035578208479,-41.0461633055085,9.34999999998873));
#19499=CARTESIAN_POINT('Ctrl Pts',(14.4035578208479,-41.0461633055085,9.34999999998873));
#19500=CARTESIAN_POINT('Ctrl Pts',(14.2852827018644,-40.8714793587097,9.55399283498179));
#19501=CARTESIAN_POINT('Ctrl Pts',(14.1734759304092,-40.6937212885446,9.75864949419063));
#19502=CARTESIAN_POINT('Ctrl Pts',(14.0681284382562,-40.5129237928371,9.96399986488825));
#19503=CARTESIAN_POINT('Ctrl Pts',(13.9854285217579,-40.3709940943454,10.1252040678792));
#19504=CARTESIAN_POINT('Ctrl Pts',(13.9067100787601,-40.2271907619831,10.2868360245804));
#19505=CARTESIAN_POINT('Ctrl Pts',(13.8319900590775,-40.0815233709314,10.4489096280657));
#19506=CARTESIAN_POINT('',(17.4539382544776,-39.8448244996745,9.34999999998873));
#19507=CARTESIAN_POINT('Origin',(0.,0.,9.34999999999998));
#19508=CARTESIAN_POINT('',(17.240901531486,-38.7143550419874,10.4701702229062));
#19509=CARTESIAN_POINT('Ctrl Pts',(17.240901531486,-38.7143550419874,10.4701702229062));
#19510=CARTESIAN_POINT('Ctrl Pts',(17.291693095119,-38.9151697801545,10.2660612053903));
#19511=CARTESIAN_POINT('Ctrl Pts',(17.3358349265524,-39.1180277521759,10.0627475751681));
#19512=CARTESIAN_POINT('Ctrl Pts',(17.3733361291177,-39.3228942754465,9.86020040449296));
#19513=CARTESIAN_POINT('Ctrl Pts',(17.4049229028391,-39.4954506755349,9.68959756483997));
#19514=CARTESIAN_POINT('Ctrl Pts',(17.4317977424317,-39.6694324844584,9.5195380044732));
#19515=CARTESIAN_POINT('Ctrl Pts',(17.4539382544776,-39.8448244996745,9.34999999998873));
#19516=CARTESIAN_POINT('',(19.3953958606399,-37.7050538275443,10.4489096280657));
#19517=CARTESIAN_POINT('Ctrl Pts',(19.3953958606399,-37.7050538275443,10.4489096280657));
#19518=CARTESIAN_POINT('Ctrl Pts',(19.2186430289534,-37.6851626990031,10.5474492452249));
#19519=CARTESIAN_POINT('Ctrl Pts',(19.0301241631229,-37.6916090034775,10.6271602259564));
#19520=CARTESIAN_POINT('Ctrl Pts',(18.6188870194185,-37.7605037117185,10.7492445866574));
#19521=CARTESIAN_POINT('Ctrl Pts',(18.3988697140028,-37.8298236027886,10.7838550844415));
#19522=CARTESIAN_POINT('Ctrl Pts',(17.9802848030949,-38.0258387393331,10.7881210903218));
#19523=CARTESIAN_POINT('Ctrl Pts',(17.7856344105885,-38.1506895294622,10.7577447440201));
#19524=CARTESIAN_POINT('Ctrl Pts',(17.467333625089,-38.4234815582466,10.6429386483201));
#19525=CARTESIAN_POINT('Ctrl Pts',(17.3402981493128,-38.5649382940451,10.5662273743849));
#19526=CARTESIAN_POINT('Ctrl Pts',(17.240901531486,-38.7143550419874,10.4701702229062));
#19527=CARTESIAN_POINT('',(20.0984284630094,-38.5785325449048,9.34999999998873));
#19528=CARTESIAN_POINT('Ctrl Pts',(20.0984284630094,-38.5785325449048,9.34999999998873));
#19529=CARTESIAN_POINT('Ctrl Pts',(19.9564970965836,-38.4224589332658,9.55399283494912));
#19530=CARTESIAN_POINT('Ctrl Pts',(19.8205307458633,-38.2624219465728,9.75864949412501));
#19531=CARTESIAN_POINT('Ctrl Pts',(19.690525372939,-38.098457220019,9.9639998647895));
#19532=CARTESIAN_POINT('Ctrl Pts',(19.5884685202378,-37.9697415864286,10.1252040678131));
#19533=CARTESIAN_POINT('Ctrl Pts',(19.4900859694781,-37.8386047671006,10.2868360245473));
#19534=CARTESIAN_POINT('Ctrl Pts',(19.3953958606399,-37.7050538275443,10.4489096280657));
#19535=CARTESIAN_POINT('',(22.9467920842464,-36.9553072378427,9.34999999998873));
#19536=CARTESIAN_POINT('Origin',(0.,0.,9.34999999999998));
#19537=CARTESIAN_POINT('',(22.5750411898809,-35.8666626160155,10.4701702229111));
#19538=CARTESIAN_POINT('Ctrl Pts',(22.5750411898809,-35.8666626160155,10.4701702229111));
#19539=CARTESIAN_POINT('Ctrl Pts',(22.6538946856459,-36.0582049566081,10.2660612053122));
#19540=CARTESIAN_POINT('Ctrl Pts',(22.7264569163886,-36.2527160894467,10.0627475750089));
#19541=CARTESIAN_POINT('Ctrl Pts',(22.7927319569317,-36.450160389405,9.86020040425393));
#19542=CARTESIAN_POINT('Ctrl Pts',(22.848554558982,-36.6164651474763,9.68959756468081));
#19543=CARTESIAN_POINT('Ctrl Pts',(22.8999160444311,-36.7848513839179,9.51953800439383));
#19544=CARTESIAN_POINT('Ctrl Pts',(22.9467920842464,-36.9553072378427,9.34999999998873));
#19545=CARTESIAN_POINT('',(24.5639673341825,-34.5610181206248,10.4489096280657));
#19546=CARTESIAN_POINT('Ctrl Pts',(24.5639673341825,-34.5610181206248,10.4489096280657));
#19547=CARTESIAN_POINT('Ctrl Pts',(24.3861827887247,-34.5664840057473,10.5474492452249));
#19548=CARTESIAN_POINT('Ctrl Pts',(24.2005001779053,-34.5996937280391,10.6271602259563));
#19549=CARTESIAN_POINT('Ctrl Pts',(23.8032535746301,-34.7264123350864,10.7492445866574));
#19550=CARTESIAN_POINT('Ctrl Pts',(23.5953409772316,-34.826338376854,10.7838550844415));
#19551=CARTESIAN_POINT('Ctrl Pts',(23.2089125196235,-35.0799292058385,10.7881210903218));
#19552=CARTESIAN_POINT('Ctrl Pts',(23.0340115074557,-35.2312108340733,10.7577447440202));
#19553=CARTESIAN_POINT('Ctrl Pts',(22.7577729184581,-35.5465251581505,10.6429386483196));
#19554=CARTESIAN_POINT('Ctrl Pts',(22.652161873134,-35.7046211015317,10.5662273743844));
#19555=CARTESIAN_POINT('Ctrl Pts',(22.5750411898777,-35.8666626160111,10.4701702229063));
#19556=CARTESIAN_POINT('',(25.3841530607455,-35.3255541129878,9.34999999998873));
#19557=CARTESIAN_POINT('Ctrl Pts',(25.3841530607455,-35.3255541129878,9.34999999998873));
#19558=CARTESIAN_POINT('Ctrl Pts',(25.2214547601852,-35.1912680451366,9.55399283494599));
#19559=CARTESIAN_POINT('Ctrl Pts',(25.0640967129913,-35.0522100334294,9.75864949411873));
#19560=CARTESIAN_POINT('Ctrl Pts',(24.9120799937713,-34.908415924999,9.96399986478005));
#19561=CARTESIAN_POINT('Ctrl Pts',(24.7927437880966,-34.7955346354507,10.1252040678068));
#19562=CARTESIAN_POINT('Ctrl Pts',(24.676699914611,-34.6797338966578,10.2868360245441));
#19563=CARTESIAN_POINT('Ctrl Pts',(24.5639673341825,-34.5610181206248,10.4489096280657));
#19564=CARTESIAN_POINT('',(27.9725154002639,-33.3134864909541,9.34999999998873));
#19565=CARTESIAN_POINT('Origin',(0.,0.,9.34999999999998));
#19566=CARTESIAN_POINT('',(27.4496181106863,-32.288828370087,10.4701702229062));
#19567=CARTESIAN_POINT('Ctrl Pts',(27.4496181106863,-32.288828370087,10.4701702229062));
#19568=CARTESIAN_POINT('Ctrl Pts',(27.5549283087466,-32.4671990632689,10.2660612053897));
#19569=CARTESIAN_POINT('Ctrl Pts',(27.654433780983,-32.6494036710323,10.0627475751668));
#19570=CARTESIAN_POINT('Ctrl Pts',(27.748133490759,-32.8354063509565,9.86020040449105));
#19571=CARTESIAN_POINT('Ctrl Pts',(27.8270555339998,-32.99207398187,9.68959756483871));
#19572=CARTESIAN_POINT('Ctrl Pts',(27.9018580936275,-33.1514367877952,9.51953800447257));
#19573=CARTESIAN_POINT('Ctrl Pts',(27.9725154002639,-33.3134864909541,9.34999999998873));
#19574=CARTESIAN_POINT('',(29.2324872694335,-30.7134197505154,10.4489096280657));
#19575=CARTESIAN_POINT('Ctrl Pts',(29.2324872694335,-30.7134197505154,10.4489096280657));
#19576=CARTESIAN_POINT('Ctrl Pts',(29.0572901908615,-30.7441313796429,10.547449245225));
#19577=CARTESIAN_POINT('Ctrl Pts',(28.8782237975451,-30.8034284655751,10.6271602259564));
#19578=CARTESIAN_POINT('Ctrl Pts',(28.503054529977,-30.9853913460156,10.7492445866574));
#19579=CARTESIAN_POINT('Ctrl Pts',(28.3114791415082,-31.1138893324332,10.7838550844415));
#19580=CARTESIAN_POINT('Ctrl Pts',(27.9650737062293,-31.4198934758751,10.7881210903218));
#19581=CARTESIAN_POINT('Ctrl Pts',(27.8134825546349,-31.5945262845251,10.7577447440201));
#19582=CARTESIAN_POINT('Ctrl Pts',(27.5849295832075,-31.9459440135453,10.6429386483201));
#19583=CARTESIAN_POINT('Ctrl Pts',(27.5028929046594,-32.1174607870144,10.5662273743849));
#19584=CARTESIAN_POINT('Ctrl Pts',(27.4496181106863,-32.288828370087,10.4701702229062));
#19585=CARTESIAN_POINT('',(30.1531295040175,-31.3534492698161,9.34999999998873));
#19586=CARTESIAN_POINT('Ctrl Pts',(30.1531295040175,-31.3534492698161,9.34999999998873));
#19587=CARTESIAN_POINT('Ctrl Pts',(29.972976337535,-31.2436844228417,9.55399283494789));
#19588=CARTESIAN_POINT('Ctrl Pts',(29.7974299499217,-31.1284362062249,9.75864949412254));
#19589=CARTESIAN_POINT('Ctrl Pts',(29.6264965064259,-31.0077399492937,9.96399986478578));
#19590=CARTESIAN_POINT('Ctrl Pts',(29.4923102887919,-30.9129909413234,10.1252040678106));
#19591=CARTESIAN_POINT('Ctrl Pts',(29.3609674112053,-30.8148836521694,10.286836024546));
#19592=CARTESIAN_POINT('Ctrl Pts',(29.2324872694335,-30.7134197505154,10.4489096280657));
#19593=CARTESIAN_POINT('',(32.4287989688052,-28.9934992272716,9.34999999998873));
#19594=CARTESIAN_POINT('Origin',(0.,0.,9.34999999999998));
#19595=CARTESIAN_POINT('',(31.7653999649232,-28.0536866918398,10.4701702229062));
#19596=CARTESIAN_POINT('Ctrl Pts',(31.7653999649232,-28.0536866918398,10.4701702229062));
#19597=CARTESIAN_POINT('Ctrl Pts',(31.8950230533648,-28.2152546247487,10.2660612053899));
#19598=CARTESIAN_POINT('Ctrl Pts',(32.0194461226553,-28.3814435471337,10.0627475751671));
#19599=CARTESIAN_POINT('Ctrl Pts',(32.1386630458013,-28.5522181289268,9.86020040449154));
#19600=CARTESIAN_POINT('Ctrl Pts',(32.2390779049944,-28.6960593314338,9.68959756483903));
#19601=CARTESIAN_POINT('Ctrl Pts',(32.3357987743735,-28.8431545396011,9.51953800447273));
#19602=CARTESIAN_POINT('Ctrl Pts',(32.4287989688052,-28.9934992272716,9.34999999998873));
#19603=CARTESIAN_POINT('',(33.3059180634108,-26.2405847244742,10.4489096280657));
#19604=CARTESIAN_POINT('Ctrl Pts',(33.3059180634108,-26.2405847244742,10.4489096280657));
#19605=CARTESIAN_POINT('Ctrl Pts',(33.1368749590177,-26.2959168974026,10.5474492452249));
#19606=CARTESIAN_POINT('Ctrl Pts',(32.9680700585873,-26.3800942293043,10.6271602259564));
#19607=CARTESIAN_POINT('Ctrl Pts',(32.6226154911153,-26.6135971436299,10.7492445866574));
#19608=CARTESIAN_POINT('Ctrl Pts',(32.4512772340277,-26.7680512262516,10.7838550844415));
#19609=CARTESIAN_POINT('Ctrl Pts',(32.1519466367895,-27.1202393222335,10.7881210903218));
#19610=CARTESIAN_POINT('Ctrl Pts',(32.0267513044621,-27.314668290914,10.7577447440201));
#19611=CARTESIAN_POINT('Ctrl Pts',(31.8505366300096,-27.6950355733208,10.6429386483201));
#19612=CARTESIAN_POINT('Ctrl Pts',(31.7937443484394,-27.8764815899828,10.5662273743849));
#19613=CARTESIAN_POINT('Ctrl Pts',(31.7653999649232,-28.0536866918397,10.4701702229062));
#19614=CARTESIAN_POINT('',(34.3082751850326,-26.7430786153924,9.34999999998873));
#19615=CARTESIAN_POINT('Ctrl Pts',(34.3082751850326,-26.7430786153924,9.34999999998873));
#19616=CARTESIAN_POINT('Ctrl Pts',(34.1143345515806,-26.6600694850449,9.55399283494758));
#19617=CARTESIAN_POINT('Ctrl Pts',(33.9241734417673,-26.5709771848618,9.75864949412193));
#19618=CARTESIAN_POINT('Ctrl Pts',(33.7378029859755,-26.4758358071633,9.96399986478487));
#19619=CARTESIAN_POINT('Ctrl Pts',(33.5914984008104,-26.4011478973383,10.12520406781));
#19620=CARTESIAN_POINT('Ctrl Pts',(33.4475302813471,-26.3227312393108,10.2868360245457));
#19621=CARTESIAN_POINT('Ctrl Pts',(33.3059180634108,-26.2405847244742,10.4489096280657));
#19622=CARTESIAN_POINT('',(36.2249257072755,-24.0832879296693,9.34999999998873));
#19623=CARTESIAN_POINT('Origin',(0.,0.,9.34999999999998));
#19624=CARTESIAN_POINT('',(35.4345298797235,-23.2474528526985,10.4701702229062));
#19625=CARTESIAN_POINT('Ctrl Pts',(35.4345298797235,-23.2474528526985,10.4701702229062));
#19626=CARTESIAN_POINT('Ctrl Pts',(35.5858271062678,-23.3889289681439,10.26606120539));
#19627=CARTESIAN_POINT('Ctrl Pts',(35.7326348777281,-23.53571907794,10.0627475751674));
#19628=CARTESIAN_POINT('Ctrl Pts',(35.874942101482,-23.68778908359,9.86020040449197));
#19629=CARTESIAN_POINT('Ctrl Pts',(35.9948056196667,-23.8158756656113,9.68959756483931));
#19630=CARTESIAN_POINT('Ctrl Pts',(36.1114758408168,-23.94770884177,9.51953800447287));
#19631=CARTESIAN_POINT('Ctrl Pts',(36.2249257072755,-24.0832879296692,9.34999999998873));
#19632=CARTESIAN_POINT('',(36.7013364119534,-21.2335670650402,10.4489096280657));
#19633=CARTESIAN_POINT('Ctrl Pts',(36.7013364119534,-21.2335670650402,10.4489096280657));
#19634=CARTESIAN_POINT('Ctrl Pts',(36.5418885288435,-21.3123933698997,10.547449234732));
#19635=CARTESIAN_POINT('Ctrl Pts',(36.3867815182114,-21.4197373256359,10.6271602090589));
#19636=CARTESIAN_POINT('Ctrl Pts',(36.0780741043059,-21.7000268175684,10.7492445801565));
#19637=CARTESIAN_POINT('Ctrl Pts',(35.9304609153722,-21.8772927714271,10.7838550842413));
#19638=CARTESIAN_POINT('Ctrl Pts',(35.6842986623995,-22.2684952883836,10.7881210901482));
#19639=CARTESIAN_POINT('Ctrl Pts',(35.5880477708337,-22.4787623858218,10.7577447489718));
#19640=CARTESIAN_POINT('Ctrl Pts',(35.4677586059889,-22.8803360402157,10.6429386624017));
#19641=CARTESIAN_POINT('Ctrl Pts',(35.4373668431343,-23.068017600367,10.5662273832428));
#19642=CARTESIAN_POINT('Ctrl Pts',(35.4345298797234,-23.2474528526985,10.4701702229062));
#19643=CARTESIAN_POINT('',(37.7650033201761,-21.5882960010295,9.34999999998873));
#19644=CARTESIAN_POINT('Ctrl Pts',(37.7650033201761,-21.5882960010295,9.34999999998873));
#19645=CARTESIAN_POINT('Ctrl Pts',(37.561223291772,-21.5337324138238,9.55399283494828));
#19646=CARTESIAN_POINT('Ctrl Pts',(37.3603185915744,-21.4726096923848,9.75864949412332));
#19647=CARTESIAN_POINT('Ctrl Pts',(37.1623050885176,-21.4049599980034,9.96399986478697));
#19648=CARTESIAN_POINT('Ctrl Pts',(37.0068604752686,-21.351853616786,10.1252040678114));
#19649=CARTESIAN_POINT('Ctrl Pts',(36.8531978896722,-21.2947239269079,10.2868360245464));
#19650=CARTESIAN_POINT('Ctrl Pts',(36.7013364119534,-21.2335670650402,10.4489096280657));
#19651=CARTESIAN_POINT('',(39.2836174224049,-18.6828103402862,9.34999999998873));
#19652=CARTESIAN_POINT('Origin',(0.,0.,9.34999999999998));
#19653=CARTESIAN_POINT('',(38.3823149509235,-17.967967913596,10.4701702229111));
#19654=CARTESIAN_POINT('Ctrl Pts',(38.3823149509235,-17.9679679135961,10.4701702229111));
#19655=CARTESIAN_POINT('Ctrl Pts',(38.5522063404067,-18.0864721658963,10.2660612053129));
#19656=CARTESIAN_POINT('Ctrl Pts',(38.7184102312306,-18.2108752398261,10.0627475750103));
#19657=CARTESIAN_POINT('Ctrl Pts',(38.8809107909569,-18.3411449626069,9.86020040425606));
#19658=CARTESIAN_POINT('Ctrl Pts',(39.0177828924946,-18.4508694506564,9.68959756468223));
#19659=CARTESIAN_POINT('Ctrl Pts',(39.1520273960987,-18.5647568514646,9.51953800439454));
#19660=CARTESIAN_POINT('Ctrl Pts',(39.2836174224049,-18.6828103402862,9.34999999998873));
#19661=CARTESIAN_POINT('',(39.3496213890631,-15.794295212713,10.4489096280657));
#19662=CARTESIAN_POINT('Ctrl Pts',(39.3496213890631,-15.794295212713,10.4489096280657));
#19663=CARTESIAN_POINT('Ctrl Pts',(39.2030145927147,-15.8950109898697,10.5474492452249));
#19664=CARTESIAN_POINT('Ctrl Pts',(39.0647629717849,-16.0233363845726,10.6271602259564));
#19665=CARTESIAN_POINT('Ctrl Pts',(38.7990871146753,-16.3447065887528,10.7492445866574));
#19666=CARTESIAN_POINT('Ctrl Pts',(38.6782040045,-16.5411757610285,10.7838550844415));
#19667=CARTESIAN_POINT('Ctrl Pts',(38.4902212524321,-16.9634289390146,10.7881210903218));
#19668=CARTESIAN_POINT('Ctrl Pts',(38.4248741812051,-17.1852537694119,10.7577447440202));
#19669=CARTESIAN_POINT('Ctrl Pts',(38.3629592862311,-17.5998589150624,10.6429386483196));
#19670=CARTESIAN_POINT('Ctrl Pts',(38.3595867413122,-17.7899553278346,10.5662273743845));
#19671=CARTESIAN_POINT('Ctrl Pts',(38.3823149509184,-17.9679679135941,10.4701702229063));
#19672=CARTESIAN_POINT('',(40.4529448929973,-15.9940379355905,9.34999999998873));
#19673=CARTESIAN_POINT('Ctrl Pts',(40.4529448929973,-15.9940379355905,9.34999999998873));
#19674=CARTESIAN_POINT('Ctrl Pts',(40.2434738433687,-15.9690306488142,9.5539928349466));
#19675=CARTESIAN_POINT('Ctrl Pts',(40.0359153931237,-15.937121788465,9.75864949411995));
#19676=CARTESIAN_POINT('Ctrl Pts',(39.8302898267027,-15.8983409300935,9.96399986478188));
#19677=CARTESIAN_POINT('Ctrl Pts',(39.668869589428,-15.8678971702586,10.125204067808));
#19678=CARTESIAN_POINT('Ctrl Pts',(39.5086406648125,-15.8332174442667,10.2868360245447));
#19679=CARTESIAN_POINT('Ctrl Pts',(39.3496213890631,-15.794295212713,10.4489096280657));
#19680=CARTESIAN_POINT('',(41.5426079714121,-12.9020046091509,9.34999999998873));
#19681=CARTESIAN_POINT('Origin',(0.,0.,9.34999999999998));
#19682=CARTESIAN_POINT('',(40.5487467751689,-12.3227069631099,10.4701702229062));
#19683=CARTESIAN_POINT('Ctrl Pts',(40.5487467751689,-12.3227069631099,10.4701702229062));
#19684=CARTESIAN_POINT('Ctrl Pts',(40.7337738287019,-12.4158269473367,10.2660612053901));
#19685=CARTESIAN_POINT('Ctrl Pts',(40.9159904068419,-12.5153104974644,10.0627475751677));
#19686=CARTESIAN_POINT('Ctrl Pts',(41.0953762596389,-12.6211280213779,9.86020040449231));
#19687=CARTESIAN_POINT('Ctrl Pts',(41.2464706233799,-12.7102567413914,9.68959756483955));
#19688=CARTESIAN_POINT('Ctrl Pts',(41.3955565785992,-12.8038799478931,9.51953800447299));
#19689=CARTESIAN_POINT('Ctrl Pts',(41.5426079714121,-12.9020046091509,9.34999999998874));
#19690=CARTESIAN_POINT('',(41.196861549629,-10.0334970568411,10.4489096280657));
#19691=CARTESIAN_POINT('Ctrl Pts',(41.196861549629,-10.0334970568411,10.4489096280657));
#19692=CARTESIAN_POINT('Ctrl Pts',(41.0660803486155,-10.1540520151186,10.5474492452249));
#19693=CARTESIAN_POINT('Ctrl Pts',(40.9474985376378,-10.3007464994071,10.6271602259564));
#19694=CARTESIAN_POINT('Ctrl Pts',(40.7302626263144,-10.6566552349241,10.7492445866574));
#19695=CARTESIAN_POINT('Ctrl Pts',(40.6385704103798,-10.8683280945857,10.7838550844415));
#19696=CARTESIAN_POINT('Ctrl Pts',(40.5125939444147,-11.3130360790174,10.7881210903218));
#19697=CARTESIAN_POINT('Ctrl Pts',(40.4794809770131,-11.5419029103595,10.7577447440201));
#19698=CARTESIAN_POINT('Ctrl Pts',(40.4772007506466,-11.9610993817016,10.6429386483201));
#19699=CARTESIAN_POINT('Ctrl Pts',(40.5009160736119,-12.1497408502739,10.5662273743849));
#19700=CARTESIAN_POINT('Ctrl Pts',(40.5487467751689,-12.3227069631099,10.4701702229062));
#19701=CARTESIAN_POINT('',(42.3173811644568,-10.0741873807795,9.34999999998873));
#19702=CARTESIAN_POINT('Ctrl Pts',(42.3173811644568,-10.0741873807795,9.34999999998873));
#19703=CARTESIAN_POINT('Ctrl Pts',(42.1064833201074,-10.0792454706758,9.55399283494713));
#19704=CARTESIAN_POINT('Ctrl Pts',(41.8964964113107,-10.0772000437951,9.75864949412103));
#19705=CARTESIAN_POINT('Ctrl Pts',(41.6874447250805,-10.0680774878744,9.96399986478351));
#19706=CARTESIAN_POINT('Ctrl Pts',(41.5233349143157,-10.0609160965801,10.1252040678091));
#19707=CARTESIAN_POINT('Ctrl Pts',(41.3598014495264,-10.0493923136882,10.2868360245452));
#19708=CARTESIAN_POINT('Ctrl Pts',(41.196861549629,-10.0334970568411,10.4489096280657));
#19709=CARTESIAN_POINT('',(42.9559108211099,-6.85855127048217,9.34999999998873));
#19710=CARTESIAN_POINT('Origin',(0.,0.,9.34999999999998));
#19711=CARTESIAN_POINT('',(41.8897230480066,-6.42659123460911,10.4701702229062));
#19712=CARTESIAN_POINT('Ctrl Pts',(41.8897230480066,-6.42659123460911,10.4701702229062));
#19713=CARTESIAN_POINT('Ctrl Pts',(42.0861191484164,-6.49243129646455,10.2660612053906));
#19714=CARTESIAN_POINT('Ctrl Pts',(42.2806390098723,-6.56497012464645,10.0627475751687));
#19715=CARTESIAN_POINT('Ctrl Pts',(42.4732583771426,-6.64418131011315,9.86020040449385));
#19716=CARTESIAN_POINT('Ctrl Pts',(42.6354991574955,-6.71089985833033,9.68959756484057));
#19717=CARTESIAN_POINT('Ctrl Pts',(42.7963916041473,-6.78235297197774,9.5195380044735));
#19718=CARTESIAN_POINT('Ctrl Pts',(42.9559108211099,-6.85855127048219,9.34999999998874));
#19719=CARTESIAN_POINT('',(42.2054524109828,-4.06844583510822,10.4489096280657));
#19720=CARTESIAN_POINT('Ctrl Pts',(42.2054524109828,-4.06844583510822,10.4489096280657));
#19721=CARTESIAN_POINT('Ctrl Pts',(42.0931591334149,-4.20638582320779,10.547449245225));
#19722=CARTESIAN_POINT('Ctrl Pts',(41.9966611160993,-4.36846312041362,10.6271602259564));
#19723=CARTESIAN_POINT('Ctrl Pts',(41.83228744726,-4.7516651117681,10.7492445866574));
#19724=CARTESIAN_POINT('Ctrl Pts',(41.7716527146639,-4.9742326098071,10.7838550844415));
#19725=CARTESIAN_POINT('Ctrl Pts',(41.7102470523625,-5.43234242855341,10.7881210903218));
#19726=CARTESIAN_POINT('Ctrl Pts',(41.7100422733126,-5.66359219215167,10.7577447440201));
#19727=CARTESIAN_POINT('Ctrl Pts',(41.7674431343865,-6.07884635789341,10.6429386483201));
#19728=CARTESIAN_POINT('Ctrl Pts',(41.8177635496502,-6.26219268596175,10.5662273743849));
#19729=CARTESIAN_POINT('Ctrl Pts',(41.8897230480066,-6.42659123460911,10.4701702229062));
#19730=CARTESIAN_POINT('',(43.3203575886581,-3.94925542245321,9.34999999998874));
#19731=CARTESIAN_POINT('Ctrl Pts',(43.3203575886581,-3.94925542245321,9.34999999998874));
#19732=CARTESIAN_POINT('Ctrl Pts',(43.1123262215187,-3.98427592089861,9.55399283494855));
#19733=CARTESIAN_POINT('Ctrl Pts',(42.9041855820802,-4.01213556647932,9.75864949412385));
#19734=CARTESIAN_POINT('Ctrl Pts',(42.6959634655163,-4.03285702194092,9.96399986478776));
#19735=CARTESIAN_POINT('Ctrl Pts',(42.5325048837559,-4.04912378446192,10.1252040678119));
#19736=CARTESIAN_POINT('Ctrl Pts',(42.3689959485452,-4.06099053565752,10.2868360245467));
#19737=CARTESIAN_POINT('Ctrl Pts',(42.2054524109828,-4.06844583510822,10.4489096280657));
#19738=CARTESIAN_POINT('',(43.4947552011075,-0.675477606375033,9.34999999998873));
#19739=CARTESIAN_POINT('Origin',(0.,0.,9.34999999999998));
#19740=CARTESIAN_POINT('',(42.3779453595727,-0.399648641330356,10.4701702229062));
#19741=CARTESIAN_POINT('Ctrl Pts',(42.3779453595728,-0.399648641330362,
10.4701702229062));
#19742=CARTESIAN_POINT('Ctrl Pts',(42.5817124486174,-0.436868467022762,
10.2660612053882));
#19743=CARTESIAN_POINT('Ctrl Pts',(42.7845757299618,-0.480985891902701,
10.0627475751638));
#19744=CARTESIAN_POINT('Ctrl Pts',(42.9865074368591,-0.531978227613834,
9.8602004044866));
#19745=CARTESIAN_POINT('Ctrl Pts',(43.1565918793968,-0.574928406792644,
9.68959756483575));
#19746=CARTESIAN_POINT('Ctrl Pts',(43.3260155112399,-0.622756848244752,
9.5195380044711));
#19747=CARTESIAN_POINT('Ctrl Pts',(43.4947552011075,-0.675477606375036,
9.34999999998873));
#19748=CARTESIAN_POINT('',(42.1897980655053,1.5002221180317E-9,10.6602019344947));
#19749=CARTESIAN_POINT('Ctrl Pts',(42.3779453595728,-0.399648641330344,
10.4701702229062));
#19750=CARTESIAN_POINT('Ctrl Pts',(42.3148062568321,-0.29790085588298,10.5342660162233));
#19751=CARTESIAN_POINT('Ctrl Pts',(42.2599040956416,-0.186267410922431,
10.5898537840787));
#19752=CARTESIAN_POINT('Ctrl Pts',(42.2057277134261,-0.0448313813822705,
10.6442542383995));
#19753=CARTESIAN_POINT('Ctrl Pts',(42.1975989914554,-0.0225266414925362,
10.6524010085462));
#19754=CARTESIAN_POINT('Ctrl Pts',(42.1897980655053,3.00045025180458E-9,
10.6602019344947));
#19755=CARTESIAN_POINT('',(41.5,-6.81700769243921E-15,11.35));
#19756=CARTESIAN_POINT('',(41.5,-6.81700769243921E-15,11.35));
#19757=CARTESIAN_POINT('Origin',(-1.73472347597681E-15,-1.73472347597681E-15,
11.35));
#19758=CARTESIAN_POINT('',(42.3548619717231,1.97942721139859,10.4489096280657));
#19759=CARTESIAN_POINT('Ctrl Pts',(42.1897980655053,3.00045276818706E-9,
10.6602019344947));
#19760=CARTESIAN_POINT('Ctrl Pts',(42.1528402486422,0.106722667340138,10.6971597513502));
#19761=CARTESIAN_POINT('Ctrl Pts',(42.1232380522063,0.21842602329369,10.7263532092198));
#19762=CARTESIAN_POINT('Ctrl Pts',(42.0584163598968,0.559888029352808,10.7884683253291));
#19763=CARTESIAN_POINT('Ctrl Pts',(42.0461300361259,0.795750669329838,10.796977768321));
#19764=CARTESIAN_POINT('Ctrl Pts',(42.0800217201965,1.20911028675496,10.7529995432141));
#19765=CARTESIAN_POINT('Ctrl Pts',(42.1138228892831,1.38567030932342,10.7137049327916));
#19766=CARTESIAN_POINT('Ctrl Pts',(42.2140016405932,1.70669242726629,10.6017906159603));
#19767=CARTESIAN_POINT('Ctrl Pts',(42.277687969919,1.8508168222083,10.5320034604965));
#19768=CARTESIAN_POINT('Ctrl Pts',(42.3548619717231,1.97942721139858,10.4489096280657));
#19769=CARTESIAN_POINT('',(43.4414564579495,2.25607198756208,9.34999999998873));
#19770=CARTESIAN_POINT('Ctrl Pts',(43.4414564579495,2.25607198756207,9.34999999998873));
#19771=CARTESIAN_POINT('Ctrl Pts',(43.2405264867429,2.19180199692502,9.55399283494924));
#19772=CARTESIAN_POINT('Ctrl Pts',(43.0384692598544,2.13460442092607,9.75864949412525));
#19773=CARTESIAN_POINT('Ctrl Pts',(42.8353155147877,2.08446078315935,9.96399986478986));
#19774=CARTESIAN_POINT('Ctrl Pts',(42.6758357073799,2.04509701119868,10.1252040678133));
#19775=CARTESIAN_POINT('Ctrl Pts',(42.5156798721472,2.01008129874923,10.2868360245474));
#19776=CARTESIAN_POINT('Ctrl Pts',(42.3548619717231,1.97942721139858,10.4489096280657));
#19777=CARTESIAN_POINT('',(43.1481717937269,5.52134683388133,9.34999999998873));
#19778=CARTESIAN_POINT('Origin',(0.,0.,9.34999999999998));
#19779=CARTESIAN_POINT('',(42.0034749115207,5.63542964579432,10.4701702229062));
#19780=CARTESIAN_POINT('Ctrl Pts',(42.0034749115207,5.63542964579433,10.4701702229062));
#19781=CARTESIAN_POINT('Ctrl Pts',(42.2104648788808,5.62758774458373,10.2660612053881));
#19782=CARTESIAN_POINT('Ctrl Pts',(42.4175418687127,5.6127898265531,10.0627475751637));
#19783=CARTESIAN_POINT('Ctrl Pts',(42.6246751680052,5.59105439750396,9.86020040448641));
#19784=CARTESIAN_POINT('Ctrl Pts',(42.799140843963,5.5727469291527,9.68959756483562));
#19785=CARTESIAN_POINT('Ctrl Pts',(42.9736466844327,5.54951680903709,9.51953800447104));
#19786=CARTESIAN_POINT('Ctrl Pts',(43.1481717937269,5.52134683388132,9.34999999998873));
#19787=CARTESIAN_POINT('',(41.6420486840549,7.98700482807798,10.4489096280657));
#19788=CARTESIAN_POINT('Ctrl Pts',(41.6420486840549,7.98700482807798,10.4489096280657));
#19789=CARTESIAN_POINT('Ctrl Pts',(41.5731662587824,7.82301570651073,10.547449245225));
#19790=CARTESIAN_POINT('Ctrl Pts',(41.526239540548,7.64031704551083,10.6271602259564));
#19791=CARTESIAN_POINT('Ctrl Pts',(41.4764846370605,7.22632801333153,10.7492445866574));
#19792=CARTESIAN_POINT('Ctrl Pts',(41.4810105474699,6.99569328456048,10.7838550844415));
#19793=CARTESIAN_POINT('Ctrl Pts',(41.5511566965011,6.53884015808498,10.7881210903218));
#19794=CARTESIAN_POINT('Ctrl Pts',(41.6161107996091,6.31689994183708,10.7577447440201));
#19795=CARTESIAN_POINT('Ctrl Pts',(41.7881771403425,5.93463817889894,10.6429386483201));
#19796=CARTESIAN_POINT('Ctrl Pts',(41.8881138550115,5.77289556463294,10.5662273743849));
#19797=CARTESIAN_POINT('Ctrl Pts',(42.0034749115207,5.63542964579435,10.4701702229062));
#19798=CARTESIAN_POINT('',(42.6782125485725,8.4154722778849,9.34999999998873));
#19799=CARTESIAN_POINT('Ctrl Pts',(42.6782125485725,8.41547227788491,9.34999999998874));
#19800=CARTESIAN_POINT('Ctrl Pts',(42.4884743280791,8.32326114672637,9.55399283494921));
#19801=CARTESIAN_POINT('Ctrl Pts',(42.2966138161958,8.23789001801242,9.75864949412517));
#19802=CARTESIAN_POINT('Ctrl Pts',(42.1026640670296,8.15934497780325,9.96399986478974));
#19803=CARTESIAN_POINT('Ctrl Pts',(41.9504095829507,8.09768552928415,10.1252040678132));
#19804=CARTESIAN_POINT('Ctrl Pts',(41.7968671586493,8.04023367450927,10.2868360245473));
#19805=CARTESIAN_POINT('Ctrl Pts',(41.6420486840549,7.98700482807799,10.4489096280657));
#19806=CARTESIAN_POINT('',(41.9232160376784,11.6057725748493,9.34999999998873));
#19807=CARTESIAN_POINT('Origin',(0.,0.,9.34999999999998));
#19808=CARTESIAN_POINT('',(40.7739348422944,11.5557868365697,10.4701702229111));
#19809=CARTESIAN_POINT('Ctrl Pts',(40.7739348422944,11.5557868365697,10.4701702229111));
#19810=CARTESIAN_POINT('Ctrl Pts',(40.9799339692217,11.5774824983428,10.2660612053109));
#19811=CARTESIAN_POINT('Ctrl Pts',(41.1870091772687,11.5923053301016,10.0627475750063));
#19812=CARTESIAN_POINT('Ctrl Pts',(41.3951274323872,11.6002692783676,9.86020040425015));
#19813=CARTESIAN_POINT('Ctrl Pts',(41.5704227236392,11.6069772080973,9.6895975646783));
#19814=CARTESIAN_POINT('Ctrl Pts',(41.7464583369758,11.6088183075705,9.51953800439259));
#19815=CARTESIAN_POINT('Ctrl Pts',(41.9232160376784,11.6057725748493,9.34999999998873));
#19816=CARTESIAN_POINT('',(40.0815233709314,13.8319900590777,10.4489096280657));
#19817=CARTESIAN_POINT('Ctrl Pts',(40.0815233709314,13.8319900590777,10.4489096280657));
#19818=CARTESIAN_POINT('Ctrl Pts',(40.0366801547423,13.6598671191027,10.5474492452249));
#19819=CARTESIAN_POINT('Ctrl Pts',(40.0162318132298,13.4723496987259,10.6271602259563));
#19820=CARTESIAN_POINT('Ctrl Pts',(40.0259001250806,13.0554936169282,10.7492445866574));
#19821=CARTESIAN_POINT('Ctrl Pts',(40.0632027123731,12.8278505213561,10.7838550844415));
#19822=CARTESIAN_POINT('Ctrl Pts',(40.1976518535586,12.3856303388352,10.7881210903218));
#19823=CARTESIAN_POINT('Ctrl Pts',(40.2935302035347,12.1751930866563,10.7577447440202));
#19824=CARTESIAN_POINT('Ctrl Pts',(40.5182466779901,11.8213097907411,10.6429386483196));
#19825=CARTESIAN_POINT('Ctrl Pts',(40.6401845549916,11.6754359604614,10.5662273743844));
#19826=CARTESIAN_POINT('Ctrl Pts',(40.7739348422892,11.5557868365679,10.4701702229063));
#19827=CARTESIAN_POINT('',(41.0461633055085,14.403557820848,9.34999999998873));
#19828=CARTESIAN_POINT('Ctrl Pts',(41.0461633055085,14.403557820848,9.34999999998873));
#19829=CARTESIAN_POINT('Ctrl Pts',(40.8714793587102,14.2852827018649,9.55399283498124));
#19830=CARTESIAN_POINT('Ctrl Pts',(40.6937212885455,14.1734759304099,9.75864949418953));
#19831=CARTESIAN_POINT('Ctrl Pts',(40.5129237928385,14.0681284382572,9.9639998648866));
#19832=CARTESIAN_POINT('Ctrl Pts',(40.3709940943463,13.9854285217585,10.125204067878));
#19833=CARTESIAN_POINT('Ctrl Pts',(40.2271907619836,13.9067100787605,10.2868360245799));
#19834=CARTESIAN_POINT('Ctrl Pts',(40.0815233709314,13.8319900590777,10.4489096280657));
#19835=CARTESIAN_POINT('',(39.8448244996745,17.4539382544778,9.34999999998873));
#19836=CARTESIAN_POINT('Origin',(0.,0.,9.34999999999998));
#19837=CARTESIAN_POINT('',(38.714355041992,17.2409015314888,10.4701702229111));
#19838=CARTESIAN_POINT('Ctrl Pts',(38.714355041992,17.2409015314888,10.4701702229111));
#19839=CARTESIAN_POINT('Ctrl Pts',(38.9151697802342,17.29169309514,10.2660612053137));
#19840=CARTESIAN_POINT('Ctrl Pts',(39.1180277523337,17.3358349265873,10.062747575012));
#19841=CARTESIAN_POINT('Ctrl Pts',(39.3228942756845,17.3733361291616,9.86020040425854));
#19842=CARTESIAN_POINT('Ctrl Pts',(39.4954506756946,17.404922902864,9.68959756468387));
#19843=CARTESIAN_POINT('Ctrl Pts',(39.6694324845389,17.431797742442,9.51953800439536));
#19844=CARTESIAN_POINT('Ctrl Pts',(39.8448244996745,17.4539382544777,9.34999999998873));
#19845=CARTESIAN_POINT('',(37.7050538275442,19.39539586064,10.4489096280657));
#19846=CARTESIAN_POINT('Ctrl Pts',(37.7050538275442,19.39539586064,10.4489096280657));
#19847=CARTESIAN_POINT('Ctrl Pts',(37.6851626990031,19.2186430289535,10.547449245225));
#19848=CARTESIAN_POINT('Ctrl Pts',(37.6916090034774,19.0301241631231,10.6271602259564));
#19849=CARTESIAN_POINT('Ctrl Pts',(37.7605037117184,18.6188870194187,10.7492445866574));
#19850=CARTESIAN_POINT('Ctrl Pts',(37.8298236027886,18.3988697140031,10.7838550844415));
#19851=CARTESIAN_POINT('Ctrl Pts',(38.0258387393331,17.9802848030951,10.7881210903218));
#19852=CARTESIAN_POINT('Ctrl Pts',(38.1506895294621,17.7856344105887,10.7577447440202));
#19853=CARTESIAN_POINT('Ctrl Pts',(38.4234815582478,17.4673336250877,10.6429386483196));
#19854=CARTESIAN_POINT('Ctrl Pts',(38.5649382940458,17.3402981493125,10.5662273743844));
#19855=CARTESIAN_POINT('Ctrl Pts',(38.7143550419872,17.2409015314862,10.4701702229063));
#19856=CARTESIAN_POINT('',(38.5785325449047,20.0984284630095,9.34999999998873));
#19857=CARTESIAN_POINT('Ctrl Pts',(38.5785325449047,20.0984284630095,9.34999999998873));
#19858=CARTESIAN_POINT('Ctrl Pts',(38.4224589332413,19.9564970965615,9.55399283498114));
#19859=CARTESIAN_POINT('Ctrl Pts',(38.2624219465224,19.8205307458207,9.75864949418933));
#19860=CARTESIAN_POINT('Ctrl Pts',(38.0984572199416,19.6905253728779,9.96399986488629));
#19861=CARTESIAN_POINT('Ctrl Pts',(37.969741586376,19.5884685201986,10.1252040678778));
#19862=CARTESIAN_POINT('Ctrl Pts',(37.8386047670737,19.4900859694592,10.2868360245798));
#19863=CARTESIAN_POINT('Ctrl Pts',(37.7050538275442,19.39539586064,10.4489096280657));
#19864=CARTESIAN_POINT('',(36.9553072378426,22.9467920842465,9.34999999998873));
#19865=CARTESIAN_POINT('Origin',(0.,0.,9.34999999999998));
#19866=CARTESIAN_POINT('',(35.8666626160154,22.575041189881,10.4701702229111));
#19867=CARTESIAN_POINT('Ctrl Pts',(35.8666626160154,22.575041189881,10.4701702229111));
#19868=CARTESIAN_POINT('Ctrl Pts',(36.0582049566091,22.6538946856465,10.266061205311));
#19869=CARTESIAN_POINT('Ctrl Pts',(36.2527160894488,22.7264569163896,10.0627475750066));
#19870=CARTESIAN_POINT('Ctrl Pts',(36.4501603894082,22.792731956933,9.86020040425056));
#19871=CARTESIAN_POINT('Ctrl Pts',(36.6164651474784,22.8485545589829,9.68959756467857));
#19872=CARTESIAN_POINT('Ctrl Pts',(36.784851383919,22.8999160444316,9.51953800439272));
#19873=CARTESIAN_POINT('Ctrl Pts',(36.9553072378426,22.9467920842465,9.34999999998873));
#19874=CARTESIAN_POINT('',(34.5610181206247,24.5639673341826,10.4489096280657));
#19875=CARTESIAN_POINT('Ctrl Pts',(34.5610181206247,24.5639673341826,10.4489096280657));
#19876=CARTESIAN_POINT('Ctrl Pts',(34.5664840057472,24.3861827887248,10.547449245225));
#19877=CARTESIAN_POINT('Ctrl Pts',(34.599693728039,24.2005001779054,10.6271602259563));
#19878=CARTESIAN_POINT('Ctrl Pts',(34.7264123350863,23.8032535746302,10.7492445866574));
#19879=CARTESIAN_POINT('Ctrl Pts',(34.8263383768539,23.5953409772317,10.7838550844415));
#19880=CARTESIAN_POINT('Ctrl Pts',(35.0799292058384,23.2089125196236,10.7881210903218));
#19881=CARTESIAN_POINT('Ctrl Pts',(35.2312108340732,23.0340115074558,10.7577447440202));
#19882=CARTESIAN_POINT('Ctrl Pts',(35.5465251581503,22.7577729184583,10.6429386483196));
#19883=CARTESIAN_POINT('Ctrl Pts',(35.7046211015316,22.6521618731341,10.5662273743845));
#19884=CARTESIAN_POINT('Ctrl Pts',(35.866662616011,22.5750411898778,10.4701702229063));
#19885=CARTESIAN_POINT('',(35.3255541129877,25.3841530607456,9.34999999998873));
#19886=CARTESIAN_POINT('Ctrl Pts',(35.3255541129877,25.3841530607456,9.34999999998873));
#19887=CARTESIAN_POINT('Ctrl Pts',(35.1912680451137,25.2214547601577,9.55399283498059));
#19888=CARTESIAN_POINT('Ctrl Pts',(35.0522100333821,25.064096712938,9.75864949418821));
#19889=CARTESIAN_POINT('Ctrl Pts',(34.9084159249257,24.912079993694,9.96399986488461));
#19890=CARTESIAN_POINT('Ctrl Pts',(34.7955346354005,24.7927437880465,10.1252040678767));
#19891=CARTESIAN_POINT('Ctrl Pts',(34.679733896632,24.6766999145867,10.2868360245792));
#19892=CARTESIAN_POINT('Ctrl Pts',(34.5610181206247,24.5639673341826,10.4489096280657));
#19893=CARTESIAN_POINT('',(33.313486490954,27.972515400264,9.34999999998873));
#19894=CARTESIAN_POINT('Origin',(0.,0.,9.34999999999998));
#19895=CARTESIAN_POINT('',(32.2888283700906,27.4496181106902,10.4701702229111));
#19896=CARTESIAN_POINT('Ctrl Pts',(32.2888283700906,27.4496181106902,10.4701702229111));
#19897=CARTESIAN_POINT('Ctrl Pts',(32.4671990633379,27.5549283087883,10.2660612053147));
#19898=CARTESIAN_POINT('Ctrl Pts',(32.6494036711709,27.6544337810593,10.062747575014));
#19899=CARTESIAN_POINT('Ctrl Pts',(32.835406351168,27.7481334908659,9.86020040426154));
#19900=CARTESIAN_POINT('Ctrl Pts',(32.9920739820132,27.8270555340672,9.68959756468587));
#19901=CARTESIAN_POINT('Ctrl Pts',(33.1514367878679,27.9018580936594,9.51953800439635));
#19902=CARTESIAN_POINT('Ctrl Pts',(33.313486490954,27.972515400264,9.34999999998873));
#19903=CARTESIAN_POINT('',(30.7134197505153,29.2324872694336,10.4489096280657));
#19904=CARTESIAN_POINT('Ctrl Pts',(30.7134197505153,29.2324872694336,10.4489096280657));
#19905=CARTESIAN_POINT('Ctrl Pts',(30.7441313796428,29.0572901908616,10.5474492452249));
#19906=CARTESIAN_POINT('Ctrl Pts',(30.803428465575,28.8782237975452,10.6271602259564));
#19907=CARTESIAN_POINT('Ctrl Pts',(30.9853913460155,28.5030545299772,10.7492445866574));
#19908=CARTESIAN_POINT('Ctrl Pts',(31.113889332433,28.3114791415084,10.7838550844415));
#19909=CARTESIAN_POINT('Ctrl Pts',(31.4198934758749,27.9650737062295,10.7881210903218));
#19910=CARTESIAN_POINT('Ctrl Pts',(31.5945262845249,27.813482554635,10.7577447440202));
#19911=CARTESIAN_POINT('Ctrl Pts',(31.9459440135467,27.5849295832066,10.6429386483196));
#19912=CARTESIAN_POINT('Ctrl Pts',(32.1174607870151,27.5028929046593,10.5662273743844));
#19913=CARTESIAN_POINT('Ctrl Pts',(32.2888283700867,27.4496181106864,10.4701702229063));
#19914=CARTESIAN_POINT('',(31.353449269816,30.1531295040176,9.34999999998873));
#19915=CARTESIAN_POINT('Ctrl Pts',(31.353449269816,30.1531295040176,9.34999999998873));
#19916=CARTESIAN_POINT('Ctrl Pts',(31.2436844228239,29.972976337506,9.55399283498083));
#19917=CARTESIAN_POINT('Ctrl Pts',(31.1284362061875,29.797429949865,9.75864949418871));
#19918=CARTESIAN_POINT('Ctrl Pts',(31.0077399492351,29.6264965063431,9.96399986488537));
#19919=CARTESIAN_POINT('Ctrl Pts',(30.9129909412829,29.4923102887379,10.1252040678772));
#19920=CARTESIAN_POINT('Ctrl Pts',(30.8148836521484,29.3609674111789,10.2868360245795));
#19921=CARTESIAN_POINT('Ctrl Pts',(30.7134197505153,29.2324872694336,10.4489096280657));
#19922=CARTESIAN_POINT('',(28.9934992272715,32.4287989688053,9.34999999998873));
#19923=CARTESIAN_POINT('Origin',(0.,0.,9.34999999999998));
#19924=CARTESIAN_POINT('',(28.0536866918396,31.7653999649234,10.4701702229062));
#19925=CARTESIAN_POINT('Ctrl Pts',(28.0536866918396,31.7653999649233,10.4701702229062));
#19926=CARTESIAN_POINT('Ctrl Pts',(28.2152546247496,31.8950230533658,10.2660612053885));
#19927=CARTESIAN_POINT('Ctrl Pts',(28.3814435471357,32.0194461226571,10.0627475751645));
#19928=CARTESIAN_POINT('Ctrl Pts',(28.55221812893,32.1386630458038,9.86020040448756));
#19929=CARTESIAN_POINT('Ctrl Pts',(28.696059331436,32.239077904996,9.68959756483639));
#19930=CARTESIAN_POINT('Ctrl Pts',(28.8431545396022,32.3357987743744,9.51953800447141));
#19931=CARTESIAN_POINT('Ctrl Pts',(28.9934992272715,32.4287989688053,9.34999999998873));
#19932=CARTESIAN_POINT('',(26.240584724474,33.3059180634109,10.4489096280657));
#19933=CARTESIAN_POINT('Ctrl Pts',(26.2405847244741,33.3059180634109,10.4489096280657));
#19934=CARTESIAN_POINT('Ctrl Pts',(26.2959168974024,33.1368749590178,10.547449245225));
#19935=CARTESIAN_POINT('Ctrl Pts',(26.3800942293042,32.9680700585874,10.6271602259564));
#19936=CARTESIAN_POINT('Ctrl Pts',(26.6135971436297,32.6226154911154,10.7492445866574));
#19937=CARTESIAN_POINT('Ctrl Pts',(26.7680512262515,32.4512772340278,10.7838550844415));
#19938=CARTESIAN_POINT('Ctrl Pts',(27.1202393222333,32.1519466367896,10.7881210903218));
#19939=CARTESIAN_POINT('Ctrl Pts',(27.3146682909138,32.0267513044622,10.7577447440201));
#19940=CARTESIAN_POINT('Ctrl Pts',(27.6950355733207,31.8505366300097,10.6429386483201));
#19941=CARTESIAN_POINT('Ctrl Pts',(27.8764815899826,31.7937443484395,10.5662273743849));
#19942=CARTESIAN_POINT('Ctrl Pts',(28.0536866918396,31.7653999649233,10.4701702229062));
#19943=CARTESIAN_POINT('',(26.7430786153922,34.3082751850327,9.34999999998873));
#19944=CARTESIAN_POINT('Ctrl Pts',(26.7430786153922,34.3082751850326,9.34999999998873));
#19945=CARTESIAN_POINT('Ctrl Pts',(26.6600694850447,34.1143345515807,9.55399283494745));
#19946=CARTESIAN_POINT('Ctrl Pts',(26.5709771848617,33.9241734417676,9.75864949412165));
#19947=CARTESIAN_POINT('Ctrl Pts',(26.4758358071633,33.737802985976,9.96399986478445));
#19948=CARTESIAN_POINT('Ctrl Pts',(26.4011478973383,33.5914984008107,10.1252040678097));
#19949=CARTESIAN_POINT('Ctrl Pts',(26.3227312393107,33.4475302813474,10.2868360245456));
#19950=CARTESIAN_POINT('Ctrl Pts',(26.2405847244741,33.3059180634109,10.4489096280657));
#19951=CARTESIAN_POINT('',(24.0832879296691,36.2249257072756,9.34999999998873));
#19952=CARTESIAN_POINT('Origin',(0.,0.,9.34999999999998));
#19953=CARTESIAN_POINT('',(23.2474528526983,35.4345298797235,10.4701702229062));
#19954=CARTESIAN_POINT('Ctrl Pts',(23.2474528526983,35.4345298797235,10.4701702229062));
#19955=CARTESIAN_POINT('Ctrl Pts',(23.3889289681428,35.5858271062667,10.2660612053916));
#19956=CARTESIAN_POINT('Ctrl Pts',(23.5357190779377,35.7326348777259,10.0627475751705));
#19957=CARTESIAN_POINT('Ctrl Pts',(23.6877890835865,35.8749421014788,9.86020040449658));
#19958=CARTESIAN_POINT('Ctrl Pts',(23.8158756656088,35.9948056196646,9.68959756484237));
#19959=CARTESIAN_POINT('Ctrl Pts',(23.9477088417686,36.1114758408158,9.51953800447439));
#19960=CARTESIAN_POINT('Ctrl Pts',(24.0832879296691,36.2249257072756,9.34999999998873));
#19961=CARTESIAN_POINT('',(21.2335670650401,36.7013364119535,10.4489096280657));
#19962=CARTESIAN_POINT('Ctrl Pts',(21.2335670650401,36.7013364119535,10.4489096280657));
#19963=CARTESIAN_POINT('Ctrl Pts',(21.3123933782934,36.5418885118648,10.547449245225));
#19964=CARTESIAN_POINT('Ctrl Pts',(21.4197373484345,36.3867814853001,10.6271602259564));
#19965=CARTESIAN_POINT('Ctrl Pts',(21.7000268506762,36.0780740767091,10.7492445866574));
#19966=CARTESIAN_POINT('Ctrl Pts',(21.8772927897887,35.9304609038183,10.7838550844415));
#19967=CARTESIAN_POINT('Ctrl Pts',(22.2684953043029,35.6842986523823,10.7881210903218));
#19968=CARTESIAN_POINT('Ctrl Pts',(22.4787624198984,35.5880477552547,10.7577447440202));
#19969=CARTESIAN_POINT('Ctrl Pts',(22.8803360747108,35.4677586003877,10.6429386483201));
#19970=CARTESIAN_POINT('Ctrl Pts',(23.0680176169135,35.4373668428728,10.5662273743849));
#19971=CARTESIAN_POINT('Ctrl Pts',(23.2474528526983,35.4345298797235,10.4701702229062));
#19972=CARTESIAN_POINT('',(21.5882960010294,37.7650033201762,9.34999999998873));
#19973=CARTESIAN_POINT('Ctrl Pts',(21.5882960010294,37.7650033201762,9.34999999998873));
#19974=CARTESIAN_POINT('Ctrl Pts',(21.533732413815,37.5612232917399,9.55399283498049));
#19975=CARTESIAN_POINT('Ctrl Pts',(21.4726096923653,37.3603185915109,9.75864949418803));
#19976=CARTESIAN_POINT('Ctrl Pts',(21.4049599979712,37.1623050884238,9.96399986488434));
#19977=CARTESIAN_POINT('Ctrl Pts',(21.3518536167628,37.0068604752068,10.1252040678765));
#19978=CARTESIAN_POINT('Ctrl Pts',(21.2947239268954,36.8531978896416,10.2868360245791));
#19979=CARTESIAN_POINT('Ctrl Pts',(21.2335670650401,36.7013364119535,10.4489096280657));
#19980=CARTESIAN_POINT('',(18.682810340286,39.283617422405,9.34999999998873));
#19981=CARTESIAN_POINT('Origin',(0.,0.,9.34999999999998));
#19982=CARTESIAN_POINT('',(17.9679679135941,38.3823149509186,10.4701702229062));
#19983=CARTESIAN_POINT('Ctrl Pts',(17.9679679135941,38.3823149509186,10.4701702229062));
#19984=CARTESIAN_POINT('Ctrl Pts',(18.0864721658495,38.5522063403388,10.2660612053895));
#19985=CARTESIAN_POINT('Ctrl Pts',(18.2108752397294,38.7184102311011,10.0627475751664));
#19986=CARTESIAN_POINT('Ctrl Pts',(18.3411449624555,38.880910790768,9.8602004044904));
#19987=CARTESIAN_POINT('Ctrl Pts',(18.4508694505517,39.0177828923714,9.68959756483827));
#19988=CARTESIAN_POINT('Ctrl Pts',(18.5647568514102,39.1520273960384,9.51953800447235));
#19989=CARTESIAN_POINT('Ctrl Pts',(18.6828103402861,39.283617422405,9.34999999998874));
#19990=CARTESIAN_POINT('',(15.7942952127128,39.3496213890631,10.4489096280657));
#19991=CARTESIAN_POINT('Ctrl Pts',(15.7942952127128,39.3496213890631,10.4489096280657));
#19992=CARTESIAN_POINT('Ctrl Pts',(15.8950109898695,39.2030145927147,10.547449245225));
#19993=CARTESIAN_POINT('Ctrl Pts',(16.0233363845725,39.0647629717849,10.6271602259564));
#19994=CARTESIAN_POINT('Ctrl Pts',(16.3447065887528,38.7990871146753,10.7492445866574));
#19995=CARTESIAN_POINT('Ctrl Pts',(16.5411757610284,38.6782040045,10.7838550844415));
#19996=CARTESIAN_POINT('Ctrl Pts',(16.9634289390145,38.4902212524321,10.7881210903218));
#19997=CARTESIAN_POINT('Ctrl Pts',(17.1852537694118,38.4248741812051,10.7577447440202));
#19998=CARTESIAN_POINT('Ctrl Pts',(17.5998589150605,38.3629592862315,10.6429386483201));
#19999=CARTESIAN_POINT('Ctrl Pts',(17.7899553278336,38.3595867413122,10.5662273743849));
#20000=CARTESIAN_POINT('Ctrl Pts',(17.9679679135941,38.3823149509185,10.4701702229062));
#20001=CARTESIAN_POINT('',(15.9940379355904,40.4529448929973,9.34999999998873));
#20002=CARTESIAN_POINT('Ctrl Pts',(15.9940379355903,40.4529448929973,9.34999999998873));
#20003=CARTESIAN_POINT('Ctrl Pts',(15.9690306488096,40.2434738433319,9.55399283498242));
#20004=CARTESIAN_POINT('Ctrl Pts',(15.9371217884536,40.0359153930508,9.7586494941919));
#20005=CARTESIAN_POINT('Ctrl Pts',(15.8983409300729,39.8302898265943,9.96399986489017));
#20006=CARTESIAN_POINT('Ctrl Pts',(15.8678971702429,39.6688695893563,10.1252040678804));
#20007=CARTESIAN_POINT('Ctrl Pts',(15.8332174442578,39.5086406647769,10.2868360245811));
#20008=CARTESIAN_POINT('Ctrl Pts',(15.7942952127128,39.3496213890631,10.4489096280657));
#20009=CARTESIAN_POINT('',(12.9020046091508,41.5426079714121,9.34999999998873));
#20010=CARTESIAN_POINT('Origin',(0.,0.,9.34999999999998));
#20011=CARTESIAN_POINT('',(12.3227069631098,40.548746775169,10.4701702229062));
#20012=CARTESIAN_POINT('Ctrl Pts',(12.3227069631098,40.548746775169,10.4701702229062));
#20013=CARTESIAN_POINT('Ctrl Pts',(12.4158269473365,40.7337738287018,10.2660612053903));
#20014=CARTESIAN_POINT('Ctrl Pts',(12.5153104974641,40.9159904068415,10.0627475751681));
#20015=CARTESIAN_POINT('Ctrl Pts',(12.6211280213774,41.0953762596384,9.86020040449293));
#20016=CARTESIAN_POINT('Ctrl Pts',(12.710256741391,41.2464706233796,9.68959756483996));
#20017=CARTESIAN_POINT('Ctrl Pts',(12.8038799478929,41.3955565785991,9.51953800447319));
#20018=CARTESIAN_POINT('Ctrl Pts',(12.9020046091508,41.5426079714121,9.34999999998873));
#20019=CARTESIAN_POINT('',(10.033497056841,41.196861549629,10.4489096280657));
#20020=CARTESIAN_POINT('Ctrl Pts',(10.033497056841,41.196861549629,10.4489096280657));
#20021=CARTESIAN_POINT('Ctrl Pts',(10.1540520151185,41.0660803486155,10.547449245225));
#20022=CARTESIAN_POINT('Ctrl Pts',(10.300746499407,40.9474985376379,10.6271602259564));
#20023=CARTESIAN_POINT('Ctrl Pts',(10.6566552349239,40.7302626263144,10.7492445866574));
#20024=CARTESIAN_POINT('Ctrl Pts',(10.8683280945855,40.6385704103798,10.7838550844415));
#20025=CARTESIAN_POINT('Ctrl Pts',(11.3130360790173,40.5125939444147,10.7881210903218));
#20026=CARTESIAN_POINT('Ctrl Pts',(11.5419029103594,40.4794809770131,10.7577447440201));
#20027=CARTESIAN_POINT('Ctrl Pts',(11.9610993817015,40.4772007506466,10.6429386483201));
#20028=CARTESIAN_POINT('Ctrl Pts',(12.1497408502737,40.500916073612,10.5662273743849));
#20029=CARTESIAN_POINT('Ctrl Pts',(12.3227069631098,40.548746775169,10.4701702229062));
#20030=CARTESIAN_POINT('',(10.0741873807793,42.3173811644569,9.34999999998873));
#20031=CARTESIAN_POINT('Ctrl Pts',(10.0741873807793,42.3173811644569,9.34999999998873));
#20032=CARTESIAN_POINT('Ctrl Pts',(10.0792454706757,42.1064833201057,9.55399283494883));
#20033=CARTESIAN_POINT('Ctrl Pts',(10.0772000437949,41.8964964113072,9.75864949412443));
#20034=CARTESIAN_POINT('Ctrl Pts',(10.068077487874,41.6874447250753,9.96399986478863));
#20035=CARTESIAN_POINT('Ctrl Pts',(10.0609160965797,41.5233349143123,10.1252040678125));
#20036=CARTESIAN_POINT('Ctrl Pts',(10.0493923136879,41.3598014495247,10.286836024547));
#20037=CARTESIAN_POINT('Ctrl Pts',(10.033497056841,41.196861549629,10.4489096280657));
#20038=CARTESIAN_POINT('',(6.85855127048205,42.9559108211099,9.34999999998873));
#20039=CARTESIAN_POINT('Origin',(0.,0.,9.34999999999998));
#20040=CARTESIAN_POINT('',(6.42659123460896,41.8897230480066,10.4701702229062));
#20041=CARTESIAN_POINT('Ctrl Pts',(6.42659123460897,41.8897230480066,10.4701702229062));
#20042=CARTESIAN_POINT('Ctrl Pts',(6.49243129646502,42.0861191484182,10.2660612053887));
#20043=CARTESIAN_POINT('Ctrl Pts',(6.56497012464767,42.2806390098759,10.0627475751649));
#20044=CARTESIAN_POINT('Ctrl Pts',(6.64418131011524,42.4732583771481,9.86020040448811));
#20045=CARTESIAN_POINT('Ctrl Pts',(6.71089985833178,42.6354991574991,9.68959756483675));
#20046=CARTESIAN_POINT('Ctrl Pts',(6.78235297197845,42.7963916041491,9.51953800447159));
#20047=CARTESIAN_POINT('Ctrl Pts',(6.85855127048204,42.95591082111,9.34999999998873));
#20048=CARTESIAN_POINT('',(4.06844583510807,42.2054524109828,10.4489096280657));
#20049=CARTESIAN_POINT('Ctrl Pts',(4.06844583510807,42.2054524109828,10.4489096280657));
#20050=CARTESIAN_POINT('Ctrl Pts',(4.2063858232076,42.0931591334149,10.547449245225));
#20051=CARTESIAN_POINT('Ctrl Pts',(4.36846312041344,41.9966611160993,10.6271602259564));
#20052=CARTESIAN_POINT('Ctrl Pts',(4.751665111768,41.83228744726,10.7492445866574));
#20053=CARTESIAN_POINT('Ctrl Pts',(4.97423260980699,41.7716527146639,10.7838550844415));
#20054=CARTESIAN_POINT('Ctrl Pts',(5.43234242855323,41.7102470523625,10.7881210903218));
#20055=CARTESIAN_POINT('Ctrl Pts',(5.66359219215152,41.7100422733126,10.7577447440201));
#20056=CARTESIAN_POINT('Ctrl Pts',(6.07884635789332,41.7674431343865,10.6429386483201));
#20057=CARTESIAN_POINT('Ctrl Pts',(6.26219268596163,41.8177635496503,10.5662273743849));
#20058=CARTESIAN_POINT('Ctrl Pts',(6.42659123460897,41.8897230480066,10.4701702229062));
#20059=CARTESIAN_POINT('',(3.94925542245304,43.3203575886581,9.34999999998873));
#20060=CARTESIAN_POINT('Ctrl Pts',(3.94925542245304,43.3203575886581,9.34999999998873));
#20061=CARTESIAN_POINT('Ctrl Pts',(3.98427592090395,43.112326221486,9.55399283498063));
#20062=CARTESIAN_POINT('Ctrl Pts',(4.01213556648794,42.9041855820147,9.75864949418831));
#20063=CARTESIAN_POINT('Ctrl Pts',(4.03285702195055,42.6959634654179,9.96399986488476));
#20064=CARTESIAN_POINT('Ctrl Pts',(4.04912378446653,42.5325048836902,10.1252040678768));
#20065=CARTESIAN_POINT('Ctrl Pts',(4.06099053565887,42.3689959485124,10.2868360245792));
#20066=CARTESIAN_POINT('Ctrl Pts',(4.06844583510807,42.2054524109828,10.4489096280657));
#20067=CARTESIAN_POINT('',(0.675477606374581,43.4947552011075,9.34999999998873));
#20068=CARTESIAN_POINT('Origin',(0.,0.,9.34999999999998));
#20069=CARTESIAN_POINT('',(0.399648641329917,42.3779453595728,10.4701702229062));
#20070=CARTESIAN_POINT('Ctrl Pts',(0.399648641329911,42.3779453595728,10.4701702229062));
#20071=CARTESIAN_POINT('Ctrl Pts',(0.436868467021998,42.5817124486157,10.2660612053899));
#20072=CARTESIAN_POINT('Ctrl Pts',(0.48098589190151,42.7845757299584,10.0627475751672));
#20073=CARTESIAN_POINT('Ctrl Pts',(0.531978227612102,42.9865074368541,9.86020040449165));
#20074=CARTESIAN_POINT('Ctrl Pts',(0.574928406791237,43.1565918793934,9.6895975648391));
#20075=CARTESIAN_POINT('Ctrl Pts',(0.622756848243766,43.3260155112382,9.51953800447277));
#20076=CARTESIAN_POINT('Ctrl Pts',(0.675477606374568,43.4947552011075,9.34999999998873));
#20077=CARTESIAN_POINT('',(-1.97942721139903,42.3548619717231,10.4489096280657));
#20078=CARTESIAN_POINT('Ctrl Pts',(-1.97942721139904,42.3548619717231,10.4489096280657));
#20079=CARTESIAN_POINT('Ctrl Pts',(-1.82691025384904,42.2633425849051,10.547449245225));
#20080=CARTESIAN_POINT('Ctrl Pts',(-1.65274957010463,42.1908927826067,10.6271602259564));
#20081=CARTESIAN_POINT('Ctrl Pts',(-1.25005521039323,42.0827275301346,10.7492445866574));
#20082=CARTESIAN_POINT('Ctrl Pts',(-1.02112390640528,42.0543846291766,10.7838550844415));
#20083=CARTESIAN_POINT('Ctrl Pts',(-0.558938048174559,42.058799812744,10.7881210903218));
#20084=CARTESIAN_POINT('Ctrl Pts',(-0.330012930637709,42.0915073907568,
10.7577447440201));
#20085=CARTESIAN_POINT('Ctrl Pts',(0.072845552183429,42.2074208232701,10.6429386483201));
#20086=CARTESIAN_POINT('Ctrl Pts',(0.247164337235477,42.2833219522895,10.5662273743849));
#20087=CARTESIAN_POINT('Ctrl Pts',(0.399648641329905,42.3779453595727,10.4701702229062));
#20088=CARTESIAN_POINT('',(-2.25607198756253,43.4414564579495,9.34999999998873));
#20089=CARTESIAN_POINT('Ctrl Pts',(-2.25607198756253,43.4414564579494,9.34999999998873));
#20090=CARTESIAN_POINT('Ctrl Pts',(-2.19180199691532,43.2405264867111,9.55399283498151));
#20091=CARTESIAN_POINT('Ctrl Pts',(-2.13460442090842,43.0384692597904,9.75864949419006));
#20092=CARTESIAN_POINT('Ctrl Pts',(-2.084460783136,42.8353155146912,9.9639998648874));
#20093=CARTESIAN_POINT('Ctrl Pts',(-2.04509701118501,42.6758357073152,10.1252040678786));
#20094=CARTESIAN_POINT('Ctrl Pts',(-2.0100812987435,42.5156798721146,10.2868360245801));
#20095=CARTESIAN_POINT('Ctrl Pts',(-1.97942721139904,42.3548619717231,10.4489096280657));
#20096=CARTESIAN_POINT('',(-5.52134683388147,43.1481717937269,9.34999999998873));
#20097=CARTESIAN_POINT('Origin',(0.,0.,9.34999999999998));
#20098=CARTESIAN_POINT('',(-5.63542964579448,42.0034749115207,10.4701702229062));
#20099=CARTESIAN_POINT('Ctrl Pts',(-5.63542964579449,42.0034749115207,10.4701702229062));
#20100=CARTESIAN_POINT('Ctrl Pts',(-5.62758774458395,42.2104648788792,10.2660612053897));
#20101=CARTESIAN_POINT('Ctrl Pts',(-5.61278982655349,42.4175418687094,10.0627475751669));
#20102=CARTESIAN_POINT('Ctrl Pts',(-5.59105439750463,42.6246751680003,9.86020040449119));
#20103=CARTESIAN_POINT('Ctrl Pts',(-5.57274692915329,42.7991408439597,9.6895975648388));
#20104=CARTESIAN_POINT('Ctrl Pts',(-5.54951680903751,42.9736466844311,9.51953800447262));
#20105=CARTESIAN_POINT('Ctrl Pts',(-5.52134683388148,43.1481717937269,9.34999999998873));
#20106=CARTESIAN_POINT('',(-7.98700482807813,41.6420486840549,10.4489096280657));
#20107=CARTESIAN_POINT('Ctrl Pts',(-7.98700482807813,41.6420486840549,10.4489096280657));
#20108=CARTESIAN_POINT('Ctrl Pts',(-7.82301570651087,41.5731662587824,10.547449245225));
#20109=CARTESIAN_POINT('Ctrl Pts',(-7.64031704551097,41.526239540548,10.6271602259564));
#20110=CARTESIAN_POINT('Ctrl Pts',(-7.22632801333171,41.4764846370605,10.7492445866574));
#20111=CARTESIAN_POINT('Ctrl Pts',(-6.99569328456065,41.4810105474699,10.7838550844415));
#20112=CARTESIAN_POINT('Ctrl Pts',(-6.53884015808512,41.5511566965011,10.7881210903218));
#20113=CARTESIAN_POINT('Ctrl Pts',(-6.31689994183723,41.6161107996091,10.7577447440201));
#20114=CARTESIAN_POINT('Ctrl Pts',(-5.93463817889906,41.7881771403424,10.6429386483201));
#20115=CARTESIAN_POINT('Ctrl Pts',(-5.77289556463307,41.8881138550115,10.5662273743849));
#20116=CARTESIAN_POINT('Ctrl Pts',(-5.6354296457945,42.0034749115207,10.4701702229062));
#20117=CARTESIAN_POINT('',(-8.41547227788506,42.6782125485725,9.34999999998873));
#20118=CARTESIAN_POINT('Ctrl Pts',(-8.41547227788505,42.6782125485725,9.34999999998873));
#20119=CARTESIAN_POINT('Ctrl Pts',(-8.32326114672774,42.4884743280816,9.55399283494648));
#20120=CARTESIAN_POINT('Ctrl Pts',(-8.23789001801484,42.2966138162009,9.75864949411971));
#20121=CARTESIAN_POINT('Ctrl Pts',(-8.15934497780653,42.1026640670373,9.96399986478153));
#20122=CARTESIAN_POINT('Ctrl Pts',(-8.09768552928625,41.9504095829559,10.1252040678078));
#20123=CARTESIAN_POINT('Ctrl Pts',(-8.04023367451032,41.7968671586518,10.2868360245446));
#20124=CARTESIAN_POINT('Ctrl Pts',(-7.98700482807813,41.6420486840549,10.4489096280657));
#20125=CARTESIAN_POINT('',(-11.6057725748495,41.9232160376784,9.34999999998873));
#20126=CARTESIAN_POINT('Origin',(0.,0.,9.34999999999998));
#20127=CARTESIAN_POINT('',(-11.5557868365679,40.7739348422893,10.4701702229062));
#20128=CARTESIAN_POINT('Ctrl Pts',(-11.5557868365679,40.7739348422893,10.4701702229062));
#20129=CARTESIAN_POINT('Ctrl Pts',(-11.5774824983335,40.9799339691383,10.266061205389));
#20130=CARTESIAN_POINT('Ctrl Pts',(-11.5923053300896,41.1870091771045,10.0627475751654));
#20131=CARTESIAN_POINT('Ctrl Pts',(-11.6002692783581,41.3951274321408,9.86020040448896));
#20132=CARTESIAN_POINT('Ctrl Pts',(-11.6069772080958,41.5704227234745,9.68959756483732));
#20133=CARTESIAN_POINT('Ctrl Pts',(-11.6088183075721,41.746458336893,9.51953800447188));
#20134=CARTESIAN_POINT('Ctrl Pts',(-11.6057725748495,41.9232160376784,9.34999999998873));
#20135=CARTESIAN_POINT('',(-13.8319900590778,40.0815233709313,10.4489096280657));
#20136=CARTESIAN_POINT('Ctrl Pts',(-13.8319900590778,40.0815233709313,10.4489096280657));
#20137=CARTESIAN_POINT('Ctrl Pts',(-13.6598671191028,40.0366801547422,10.5474492452249));
#20138=CARTESIAN_POINT('Ctrl Pts',(-13.4723496987259,40.0162318132297,10.6271602259564));
#20139=CARTESIAN_POINT('Ctrl Pts',(-13.0554936169282,40.0259001250806,10.7492445866574));
#20140=CARTESIAN_POINT('Ctrl Pts',(-12.8278505213562,40.0632027123731,10.7838550844415));
#20141=CARTESIAN_POINT('Ctrl Pts',(-12.3856303388352,40.1976518535586,10.7881210903218));
#20142=CARTESIAN_POINT('Ctrl Pts',(-12.1751930866564,40.2935302035347,10.7577447440201));
#20143=CARTESIAN_POINT('Ctrl Pts',(-11.8213097907427,40.5182466779891,10.6429386483201));
#20144=CARTESIAN_POINT('Ctrl Pts',(-11.6754359604621,40.6401845549909,10.5662273743849));
#20145=CARTESIAN_POINT('Ctrl Pts',(-11.5557868365679,40.7739348422893,10.4701702229062));
#20146=CARTESIAN_POINT('',(-14.4035578208482,41.0461633055084,9.34999999998873));
#20147=CARTESIAN_POINT('Ctrl Pts',(-14.4035578208482,41.0461633055084,9.34999999998873));
#20148=CARTESIAN_POINT('Ctrl Pts',(-14.2852827018843,40.8714793587385,9.55399283494804));
#20149=CARTESIAN_POINT('Ctrl Pts',(-14.1734759304465,40.6937212886033,9.75864949412283));
#20150=CARTESIAN_POINT('Ctrl Pts',(-14.0681284383089,40.5129237929268,9.96399986478622));
#20151=CARTESIAN_POINT('Ctrl Pts',(-13.9854285217914,40.370994094406,10.1252040678109));
#20152=CARTESIAN_POINT('Ctrl Pts',(-13.9067100787762,40.2271907620138,10.2868360245461));
#20153=CARTESIAN_POINT('Ctrl Pts',(-13.8319900590778,40.0815233709313,10.4489096280657));
#20154=CARTESIAN_POINT('',(-17.4539382544779,39.8448244996744,9.34999999998873));
#20155=CARTESIAN_POINT('Origin',(0.,0.,9.34999999999998));
#20156=CARTESIAN_POINT('',(-17.2409015314889,38.7143550419919,10.4701702229111));
#20157=CARTESIAN_POINT('Ctrl Pts',(-17.2409015314889,38.7143550419919,10.4701702229111));
#20158=CARTESIAN_POINT('Ctrl Pts',(-17.2916930951406,38.9151697802362,10.2660612053116));
#20159=CARTESIAN_POINT('Ctrl Pts',(-17.3358349265883,39.1180277523379,10.0627475750077));
#20160=CARTESIAN_POINT('Ctrl Pts',(-17.3733361291629,39.3228942756909,9.86020040425219));
#20161=CARTESIAN_POINT('Ctrl Pts',(-17.4049229028648,39.4954506756989,9.68959756467966));
#20162=CARTESIAN_POINT('Ctrl Pts',(-17.4317977424424,39.669432484541,9.51953800439327));
#20163=CARTESIAN_POINT('Ctrl Pts',(-17.4539382544779,39.8448244996744,9.34999999998873));
#20164=CARTESIAN_POINT('',(-19.3953958606401,37.7050538275442,10.4489096280657));
#20165=CARTESIAN_POINT('Ctrl Pts',(-19.3953958606401,37.7050538275442,10.4489096280657));
#20166=CARTESIAN_POINT('Ctrl Pts',(-19.2186430289537,37.685162699003,10.547449245225));
#20167=CARTESIAN_POINT('Ctrl Pts',(-19.0301241631232,37.6916090034774,10.6271602259564));
#20168=CARTESIAN_POINT('Ctrl Pts',(-18.6188870194189,37.7605037117184,10.7492445866574));
#20169=CARTESIAN_POINT('Ctrl Pts',(-18.3988697140032,37.8298236027885,10.7838550844415));
#20170=CARTESIAN_POINT('Ctrl Pts',(-17.9802848030952,38.025838739333,10.7881210903218));
#20171=CARTESIAN_POINT('Ctrl Pts',(-17.7856344105889,38.150689529462,10.7577447440202));
#20172=CARTESIAN_POINT('Ctrl Pts',(-17.4673336250879,38.4234815582477,10.6429386483196));
#20173=CARTESIAN_POINT('Ctrl Pts',(-17.3402981493126,38.5649382940457,10.5662273743844));
#20174=CARTESIAN_POINT('Ctrl Pts',(-17.2409015314864,38.7143550419871,10.4701702229063));
#20175=CARTESIAN_POINT('',(-20.0984284630096,38.5785325449046,9.34999999998873));
#20176=CARTESIAN_POINT('Ctrl Pts',(-20.0984284630096,38.5785325449046,9.34999999998873));
#20177=CARTESIAN_POINT('Ctrl Pts',(-19.9564970965613,38.4224589332409,9.55399283498155));
#20178=CARTESIAN_POINT('Ctrl Pts',(-19.8205307458203,38.2624219465217,9.75864949419015));
#20179=CARTESIAN_POINT('Ctrl Pts',(-19.6905253728772,38.0984572199405,9.96399986488752));
#20180=CARTESIAN_POINT('Ctrl Pts',(-19.5884685201982,37.9697415863752,10.1252040678787));
#20181=CARTESIAN_POINT('Ctrl Pts',(-19.4900859694591,37.8386047670733,10.2868360245802));
#20182=CARTESIAN_POINT('Ctrl Pts',(-19.3953958606401,37.7050538275442,10.4489096280657));
#20183=CARTESIAN_POINT('',(-22.9467920842467,36.9553072378425,9.34999999998873));
#20184=CARTESIAN_POINT('Origin',(0.,0.,9.34999999999998));
#20185=CARTESIAN_POINT('',(-22.5750411898779,35.8666626160111,10.4701702229062));
#20186=CARTESIAN_POINT('Ctrl Pts',(-22.5750411898779,35.8666626160111,10.4701702229062));
#20187=CARTESIAN_POINT('Ctrl Pts',(-22.6538946856141,36.0582049565317,10.2660612053891));
#20188=CARTESIAN_POINT('Ctrl Pts',(-22.7264569163319,36.2527160892947,10.0627475751656));
#20189=CARTESIAN_POINT('Ctrl Pts',(-22.7927319568545,36.4501603891746,9.8602004044892));
#20190=CARTESIAN_POINT('Ctrl Pts',(-22.848554558935,36.616465147321,9.68959756483748));
#20191=CARTESIAN_POINT('Ctrl Pts',(-22.8999160444098,36.7848513838393,9.51953800447196));
#20192=CARTESIAN_POINT('Ctrl Pts',(-22.9467920842467,36.9553072378425,9.34999999998873));
#20193=CARTESIAN_POINT('',(-24.5639673341827,34.5610181206246,10.4489096280657));
#20194=CARTESIAN_POINT('Ctrl Pts',(-24.5639673341828,34.5610181206246,10.4489096280657));
#20195=CARTESIAN_POINT('Ctrl Pts',(-24.3861827887249,34.5664840057471,10.547449245225));
#20196=CARTESIAN_POINT('Ctrl Pts',(-24.2005001779055,34.5996937280389,10.6271602259564));
#20197=CARTESIAN_POINT('Ctrl Pts',(-23.8032535746302,34.7264123350863,10.7492445866574));
#20198=CARTESIAN_POINT('Ctrl Pts',(-23.5953409772317,34.8263383768539,10.7838550844415));
#20199=CARTESIAN_POINT('Ctrl Pts',(-23.2089125196236,35.0799292058384,10.7881210903218));
#20200=CARTESIAN_POINT('Ctrl Pts',(-23.0340115074558,35.2312108340732,10.7577447440201));
#20201=CARTESIAN_POINT('Ctrl Pts',(-22.7577729184596,35.5465251581489,10.6429386483201));
#20202=CARTESIAN_POINT('Ctrl Pts',(-22.6521618731346,35.7046211015308,10.5662273743849));
#20203=CARTESIAN_POINT('Ctrl Pts',(-22.5750411898779,35.8666626160111,10.4701702229062));
#20204=CARTESIAN_POINT('',(-25.3841530607458,35.3255541129876,9.34999999998873));
#20205=CARTESIAN_POINT('Ctrl Pts',(-25.3841530607458,35.3255541129876,9.34999999998873));
#20206=CARTESIAN_POINT('Ctrl Pts',(-25.2214547601583,35.191268045114,9.55399283498005));
#20207=CARTESIAN_POINT('Ctrl Pts',(-25.064096712939,35.0522100333827,9.75864949418713));
#20208=CARTESIAN_POINT('Ctrl Pts',(-24.9120799936953,34.9084159249267,9.96399986488299));
#20209=CARTESIAN_POINT('Ctrl Pts',(-24.7927437880474,34.7955346354012,10.1252040678756));
#20210=CARTESIAN_POINT('Ctrl Pts',(-24.6766999145872,34.6797338966323,10.2868360245787));
#20211=CARTESIAN_POINT('Ctrl Pts',(-24.5639673341828,34.5610181206246,10.4489096280657));
#20212=CARTESIAN_POINT('',(-27.9725154002642,33.3134864909539,9.34999999998873));
#20213=CARTESIAN_POINT('Origin',(0.,0.,9.34999999999998));
#20214=CARTESIAN_POINT('',(-27.4496181106865,32.2888283700868,10.4701702229062));
#20215=CARTESIAN_POINT('Ctrl Pts',(-27.4496181106865,32.2888283700868,10.4701702229062));
#20216=CARTESIAN_POINT('Ctrl Pts',(-27.5549283087472,32.4671990632694,10.2660612053888));
#20217=CARTESIAN_POINT('Ctrl Pts',(-27.654433780984,32.6494036710336,10.0627475751651));
#20218=CARTESIAN_POINT('Ctrl Pts',(-27.7481334907604,32.8354063509586,9.86020040448855));
#20219=CARTESIAN_POINT('Ctrl Pts',(-27.8270555340008,32.9920739818714,9.68959756483705));
#20220=CARTESIAN_POINT('Ctrl Pts',(-27.9018580936281,33.1514367877958,9.51953800447174));
#20221=CARTESIAN_POINT('Ctrl Pts',(-27.9725154002642,33.3134864909539,9.34999999998874));
#20222=CARTESIAN_POINT('',(-29.2324872694337,30.7134197505152,10.4489096280657));
#20223=CARTESIAN_POINT('Ctrl Pts',(-29.2324872694337,30.7134197505152,10.4489096280657));
#20224=CARTESIAN_POINT('Ctrl Pts',(-29.0572901908617,30.7441313796427,10.547449245225));
#20225=CARTESIAN_POINT('Ctrl Pts',(-28.8782237975453,30.8034284655749,10.6271602259564));
#20226=CARTESIAN_POINT('Ctrl Pts',(-28.5030545299772,30.9853913460154,10.7492445866574));
#20227=CARTESIAN_POINT('Ctrl Pts',(-28.3114791415084,31.113889332433,10.7838550844415));
#20228=CARTESIAN_POINT('Ctrl Pts',(-27.9650737062295,31.4198934758749,10.7881210903218));
#20229=CARTESIAN_POINT('Ctrl Pts',(-27.8134825546351,31.5945262845249,10.7577447440201));
#20230=CARTESIAN_POINT('Ctrl Pts',(-27.5849295832077,31.9459440135451,10.6429386483201));
#20231=CARTESIAN_POINT('Ctrl Pts',(-27.5028929046597,32.1174607870142,10.5662273743849));
#20232=CARTESIAN_POINT('Ctrl Pts',(-27.4496181106865,32.2888283700868,10.4701702229062));
#20233=CARTESIAN_POINT('',(-30.1531295040177,31.3534492698159,9.34999999998873));
#20234=CARTESIAN_POINT('Ctrl Pts',(-30.1531295040177,31.3534492698159,9.34999999998873));
#20235=CARTESIAN_POINT('Ctrl Pts',(-29.9729763375347,31.2436844228412,9.5539928349485));
#20236=CARTESIAN_POINT('Ctrl Pts',(-29.7974299499209,31.128436206224,9.75864949412376));
#20237=CARTESIAN_POINT('Ctrl Pts',(-29.6264965064245,31.0077399492924,9.96399986478763));
#20238=CARTESIAN_POINT('Ctrl Pts',(-29.4923102887911,30.9129909413225,10.1252040678118));
#20239=CARTESIAN_POINT('Ctrl Pts',(-29.360967411205,30.8148836521688,10.2868360245466));
#20240=CARTESIAN_POINT('Ctrl Pts',(-29.2324872694337,30.7134197505152,10.4489096280657));
#20241=CARTESIAN_POINT('',(-32.4287989688054,28.9934992272714,9.34999999998873));
#20242=CARTESIAN_POINT('Origin',(0.,0.,9.34999999999998));
#20243=CARTESIAN_POINT('',(-31.7653999649278,28.0536866918426,10.4701702229111));
#20244=CARTESIAN_POINT('Ctrl Pts',(-31.7653999649278,28.0536866918426,10.4701702229111));
#20245=CARTESIAN_POINT('Ctrl Pts',(-31.8950230534163,28.2152546248113,10.2660612053145));
#20246=CARTESIAN_POINT('Ctrl Pts',(-32.0194461227511,28.3814435472605,10.0627475750136));
#20247=CARTESIAN_POINT('Ctrl Pts',(-32.138663045938,28.5522181291217,9.86020040426097));
#20248=CARTESIAN_POINT('Ctrl Pts',(-32.239077905082,28.6960593315664,9.68959756468549));
#20249=CARTESIAN_POINT('Ctrl Pts',(-32.3357987744158,28.8431545396688,9.51953800439617));
#20250=CARTESIAN_POINT('Ctrl Pts',(-32.4287989688055,28.9934992272714,9.34999999998873));
#20251=CARTESIAN_POINT('',(-33.305918063411,26.2405847244739,10.4489096280657));
#20252=CARTESIAN_POINT('Ctrl Pts',(-33.305918063411,26.2405847244739,10.4489096280657));
#20253=CARTESIAN_POINT('Ctrl Pts',(-33.1368749590179,26.2959168974023,10.5474492452249));
#20254=CARTESIAN_POINT('Ctrl Pts',(-32.9680700585876,26.380094229304,10.6271602259563));
#20255=CARTESIAN_POINT('Ctrl Pts',(-32.6226154911156,26.6135971436295,10.7492445866574));
#20256=CARTESIAN_POINT('Ctrl Pts',(-32.451277234028,26.7680512262512,10.7838550844415));
#20257=CARTESIAN_POINT('Ctrl Pts',(-32.1519466367897,27.1202393222332,10.7881210903218));
#20258=CARTESIAN_POINT('Ctrl Pts',(-32.0267513044624,27.3146682909137,10.7577447440202));
#20259=CARTESIAN_POINT('Ctrl Pts',(-31.850536630009,27.6950355733222,10.6429386483196));
#20260=CARTESIAN_POINT('Ctrl Pts',(-31.7937443484395,27.8764815899834,10.5662273743844));
#20261=CARTESIAN_POINT('Ctrl Pts',(-31.7653999649235,28.0536866918393,10.4701702229063));
#20262=CARTESIAN_POINT('',(-34.3082751850328,26.7430786153922,9.34999999998873));
#20263=CARTESIAN_POINT('Ctrl Pts',(-34.3082751850328,26.7430786153922,9.34999999998873));
#20264=CARTESIAN_POINT('Ctrl Pts',(-34.1143345515816,26.660069485045,9.55399283494663));
#20265=CARTESIAN_POINT('Ctrl Pts',(-33.9241734417693,26.5709771848624,9.75864949412001));
#20266=CARTESIAN_POINT('Ctrl Pts',(-33.7378029859783,26.4758358071644,9.96399986478199));
#20267=CARTESIAN_POINT('Ctrl Pts',(-33.5914984008123,26.401147897339,10.1252040678081));
#20268=CARTESIAN_POINT('Ctrl Pts',(-33.4475302813482,26.3227312393111,10.2868360245447));
#20269=CARTESIAN_POINT('Ctrl Pts',(-33.305918063411,26.2405847244739,10.4489096280657));
#20270=CARTESIAN_POINT('',(-36.2249257072757,24.083287929669,9.34999999998873));
#20271=CARTESIAN_POINT('Origin',(0.,0.,9.34999999999998));
#20272=CARTESIAN_POINT('',(-35.4345298797236,23.2474528526982,10.4701702229062));
#20273=CARTESIAN_POINT('Ctrl Pts',(-35.4345298797236,23.2474528526982,10.4701702229062));
#20274=CARTESIAN_POINT('Ctrl Pts',(-35.585827106268,23.3889289681438,10.2660612053899));
#20275=CARTESIAN_POINT('Ctrl Pts',(-35.7326348777284,23.5357190779399,10.0627475751672));
#20276=CARTESIAN_POINT('Ctrl Pts',(-35.8749421014824,23.68778908359,9.86020040449166));
#20277=CARTESIAN_POINT('Ctrl Pts',(-35.994805619667,23.8158756656112,9.68959756483911));
#20278=CARTESIAN_POINT('Ctrl Pts',(-36.111475840817,23.9477088417698,9.51953800447277));
#20279=CARTESIAN_POINT('Ctrl Pts',(-36.2249257072757,24.083287929669,9.34999999998873));
#20280=CARTESIAN_POINT('',(-36.7013364119536,21.2335670650399,10.4489096280657));
#20281=CARTESIAN_POINT('Ctrl Pts',(-36.7013364119536,21.2335670650399,10.4489096280657));
#20282=CARTESIAN_POINT('Ctrl Pts',(-36.5418885288437,21.3123933698994,10.547449234732));
#20283=CARTESIAN_POINT('Ctrl Pts',(-36.3867815182115,21.4197373256356,10.6271602090589));
#20284=CARTESIAN_POINT('Ctrl Pts',(-36.0780741043061,21.7000268175682,10.7492445801565));
#20285=CARTESIAN_POINT('Ctrl Pts',(-35.9304609153724,21.8772927714269,10.7838550842413));
#20286=CARTESIAN_POINT('Ctrl Pts',(-35.6842986623997,22.2684952883833,10.7881210901482));
#20287=CARTESIAN_POINT('Ctrl Pts',(-35.5880477708339,22.4787623858216,10.7577447489718));
#20288=CARTESIAN_POINT('Ctrl Pts',(-35.4677586059891,22.8803360402155,10.6429386624017));
#20289=CARTESIAN_POINT('Ctrl Pts',(-35.4373668431344,23.0680176003667,10.5662273832428));
#20290=CARTESIAN_POINT('Ctrl Pts',(-35.4345298797236,23.2474528526982,10.4701702229062));
#20291=CARTESIAN_POINT('',(-37.7650033201763,21.5882960010293,9.34999999998873));
#20292=CARTESIAN_POINT('Ctrl Pts',(-37.7650033201763,21.5882960010293,9.34999999998873));
#20293=CARTESIAN_POINT('Ctrl Pts',(-37.5612232917734,21.5337324138239,9.55399283494698));
#20294=CARTESIAN_POINT('Ctrl Pts',(-37.3603185915771,21.4726096923853,9.75864949412072));
#20295=CARTESIAN_POINT('Ctrl Pts',(-37.1623050885215,21.4049599980044,9.96399986478304));
#20296=CARTESIAN_POINT('Ctrl Pts',(-37.0068604752713,21.3518536167866,10.1252040678088));
#20297=CARTESIAN_POINT('Ctrl Pts',(-36.8531978896736,21.2947239269081,10.2868360245451));
#20298=CARTESIAN_POINT('Ctrl Pts',(-36.7013364119536,21.2335670650399,10.4489096280657));
#20299=CARTESIAN_POINT('',(-39.2836174224051,18.6828103402859,9.34999999998873));
#20300=CARTESIAN_POINT('Origin',(0.,0.,9.34999999999998));
#20301=CARTESIAN_POINT('',(-38.3823149509186,17.967967913594,10.4701702229062));
#20302=CARTESIAN_POINT('Ctrl Pts',(-38.3823149509186,17.967967913594,10.4701702229062));
#20303=CARTESIAN_POINT('Ctrl Pts',(-38.5522063403375,18.0864721658485,10.2660612053911));
#20304=CARTESIAN_POINT('Ctrl Pts',(-38.7184102310986,18.2108752397274,10.0627475751696));
#20305=CARTESIAN_POINT('Ctrl Pts',(-38.8809107907643,18.3411449624523,9.86020040449518));
#20306=CARTESIAN_POINT('Ctrl Pts',(-39.017782892369,18.4508694505494,9.68959756484145));
#20307=CARTESIAN_POINT('Ctrl Pts',(-39.1520273960372,18.564756851409,9.51953800447394));
#20308=CARTESIAN_POINT('Ctrl Pts',(-39.2836174224051,18.6828103402859,9.34999999998873));
#20309=CARTESIAN_POINT('',(-39.3496213890632,15.7942952127127,10.4489096280657));
#20310=CARTESIAN_POINT('Ctrl Pts',(-39.3496213890632,15.7942952127127,10.4489096280657));
#20311=CARTESIAN_POINT('Ctrl Pts',(-39.2030145927148,15.8950109898694,10.547449245225));
#20312=CARTESIAN_POINT('Ctrl Pts',(-39.0647629717849,16.0233363845724,10.6271602259564));
#20313=CARTESIAN_POINT('Ctrl Pts',(-38.7990871146753,16.3447065887526,10.7492445866574));
#20314=CARTESIAN_POINT('Ctrl Pts',(-38.6782040045001,16.5411757610283,10.7838550844415));
#20315=CARTESIAN_POINT('Ctrl Pts',(-38.4902212524322,16.9634289390144,10.7881210903218));
#20316=CARTESIAN_POINT('Ctrl Pts',(-38.4248741812052,17.1852537694117,10.7577447440201));
#20317=CARTESIAN_POINT('Ctrl Pts',(-38.3629592862315,17.5998589150603,10.6429386483201));
#20318=CARTESIAN_POINT('Ctrl Pts',(-38.3595867413123,17.7899553278335,10.5662273743849));
#20319=CARTESIAN_POINT('Ctrl Pts',(-38.3823149509186,17.967967913594,10.4701702229062));
#20320=CARTESIAN_POINT('',(-40.4529448929974,15.9940379355902,9.34999999998873));
#20321=CARTESIAN_POINT('Ctrl Pts',(-40.4529448929974,15.9940379355902,9.34999999998873));
#20322=CARTESIAN_POINT('Ctrl Pts',(-40.2434738433334,15.9690306488097,9.55399283498108));
#20323=CARTESIAN_POINT('Ctrl Pts',(-40.0359153930536,15.9371217884539,9.75864949418921));
#20324=CARTESIAN_POINT('Ctrl Pts',(-39.8302898265985,15.8983409300735,9.96399986488612));
#20325=CARTESIAN_POINT('Ctrl Pts',(-39.668869589359,15.8678971702433,10.1252040678777));
#20326=CARTESIAN_POINT('Ctrl Pts',(-39.5086406647783,15.833217444258,10.2868360245797));
#20327=CARTESIAN_POINT('Ctrl Pts',(-39.3496213890632,15.7942952127127,10.4489096280657));
#20328=CARTESIAN_POINT('',(-41.5426079714122,12.9020046091506,9.34999999998873));
#20329=CARTESIAN_POINT('Origin',(0.,0.,9.34999999999998));
#20330=CARTESIAN_POINT('',(-40.548746775169,12.3227069631096,10.4701702229062));
#20331=CARTESIAN_POINT('Ctrl Pts',(-40.548746775169,12.3227069631096,10.4701702229062));
#20332=CARTESIAN_POINT('Ctrl Pts',(-40.7337738287004,12.4158269473356,10.2660612053919));
#20333=CARTESIAN_POINT('Ctrl Pts',(-40.9159904068387,12.5153104974624,10.0627475751713));
#20334=CARTESIAN_POINT('Ctrl Pts',(-41.0953762596343,12.6211280213747,9.8602004044977));
#20335=CARTESIAN_POINT('Ctrl Pts',(-41.2464706233768,12.7102567413891,9.68959756484312));
#20336=CARTESIAN_POINT('Ctrl Pts',(-41.3955565785978,12.8038799478918,9.51953800447477));
#20337=CARTESIAN_POINT('Ctrl Pts',(-41.5426079714122,12.9020046091506,9.34999999998873));
#20338=CARTESIAN_POINT('',(-41.1968615496291,10.0334970568409,10.4489096280657));
#20339=CARTESIAN_POINT('Ctrl Pts',(-41.1968615496291,10.0334970568408,10.4489096280657));
#20340=CARTESIAN_POINT('Ctrl Pts',(-41.0660803486155,10.1540520151183,10.547449245225));
#20341=CARTESIAN_POINT('Ctrl Pts',(-40.9474985376379,10.3007464994068,10.6271602259564));
#20342=CARTESIAN_POINT('Ctrl Pts',(-40.7302626263145,10.6566552349238,10.7492445866574));
#20343=CARTESIAN_POINT('Ctrl Pts',(-40.6385704103799,10.8683280945854,10.7838550844415));
#20344=CARTESIAN_POINT('Ctrl Pts',(-40.5125939444148,11.3130360790171,10.7881210903218));
#20345=CARTESIAN_POINT('Ctrl Pts',(-40.4794809770131,11.5419029103592,10.7577447440201));
#20346=CARTESIAN_POINT('Ctrl Pts',(-40.4772007506467,11.9610993817013,10.6429386483201));
#20347=CARTESIAN_POINT('Ctrl Pts',(-40.500916073612,12.1497408502736,10.5662273743849));
#20348=CARTESIAN_POINT('Ctrl Pts',(-40.548746775169,12.3227069631096,10.4701702229062));
#20349=CARTESIAN_POINT('',(-42.3173811644569,10.0741873807792,9.34999999998873));
#20350=CARTESIAN_POINT('Ctrl Pts',(-42.3173811644569,10.0741873807792,9.34999999998873));
#20351=CARTESIAN_POINT('Ctrl Pts',(-42.1064833200743,10.0792454706763,9.55399283497921));
#20352=CARTESIAN_POINT('Ctrl Pts',(-41.8964964112446,10.0772000437942,9.75864949418546));
#20353=CARTESIAN_POINT('Ctrl Pts',(-41.6874447249818,10.0680774878698,9.96399986488047));
#20354=CARTESIAN_POINT('Ctrl Pts',(-41.5233349142502,10.0609160965752,10.125204067874));
#20355=CARTESIAN_POINT('Ctrl Pts',(-41.3598014494938,10.0493923136847,10.2868360245778));
#20356=CARTESIAN_POINT('Ctrl Pts',(-41.1968615496291,10.0334970568408,10.4489096280657));
#20357=CARTESIAN_POINT('',(-42.95591082111,6.85855127048189,9.34999999998873));
#20358=CARTESIAN_POINT('Origin',(0.,0.,9.34999999999998));
#20359=CARTESIAN_POINT('',(-41.8897230480067,6.4265912346088,10.4701702229062));
#20360=CARTESIAN_POINT('Ctrl Pts',(-41.8897230480067,6.4265912346088,10.4701702229062));
#20361=CARTESIAN_POINT('Ctrl Pts',(-42.0861191484169,6.49243129646439,10.2660612053901));
#20362=CARTESIAN_POINT('Ctrl Pts',(-42.2806390098733,6.56497012464649,10.0627475751677));
#20363=CARTESIAN_POINT('Ctrl Pts',(-42.4732583771441,6.64418131011342,9.86020040449235));
#20364=CARTESIAN_POINT('Ctrl Pts',(-42.6354991574965,6.71089985833043,9.68959756483957));
#20365=CARTESIAN_POINT('Ctrl Pts',(-42.7963916041478,6.78235297197764,9.519538004473));
#20366=CARTESIAN_POINT('Ctrl Pts',(-42.95591082111,6.85855127048187,9.34999999998873));
#20367=CARTESIAN_POINT('',(-42.2054524109828,4.06844583510791,10.4489096280657));
#20368=CARTESIAN_POINT('Ctrl Pts',(-42.2054524109828,4.06844583510792,10.4489096280657));
#20369=CARTESIAN_POINT('Ctrl Pts',(-42.093159133415,4.20638582320746,10.547449245225));
#20370=CARTESIAN_POINT('Ctrl Pts',(-41.9966611160993,4.3684631204133,10.6271602259564));
#20371=CARTESIAN_POINT('Ctrl Pts',(-41.83228744726,4.75166511176785,10.7492445866574));
#20372=CARTESIAN_POINT('Ctrl Pts',(-41.7716527146639,4.97423260980683,10.7838550844415));
#20373=CARTESIAN_POINT('Ctrl Pts',(-41.7102470523625,5.43234242855308,10.7881210903218));
#20374=CARTESIAN_POINT('Ctrl Pts',(-41.7100422733127,5.66359219215136,10.7577447440201));
#20375=CARTESIAN_POINT('Ctrl Pts',(-41.7674431343866,6.07884635789314,10.6429386483201));
#20376=CARTESIAN_POINT('Ctrl Pts',(-41.8177635496503,6.26219268596147,10.5662273743849));
#20377=CARTESIAN_POINT('Ctrl Pts',(-41.8897230480067,6.42659123460881,10.4701702229062));
#20378=CARTESIAN_POINT('',(-43.3203575886581,3.94925542245288,9.34999999998873));
#20379=CARTESIAN_POINT('Ctrl Pts',(-43.3203575886581,3.94925542245288,9.34999999998873));
#20380=CARTESIAN_POINT('Ctrl Pts',(-43.1123262214859,3.98427592090381,9.55399283498075));
#20381=CARTESIAN_POINT('Ctrl Pts',(-42.9041855820145,4.01213556648781,9.75864949418855));
#20382=CARTESIAN_POINT('Ctrl Pts',(-42.6959634654176,4.03285702195043,9.96399986488512));
#20383=CARTESIAN_POINT('Ctrl Pts',(-42.53250488369,4.04912378446638,10.1252040678771));
#20384=CARTESIAN_POINT('Ctrl Pts',(-42.3689959485123,4.06099053565872,10.2868360245794));
#20385=CARTESIAN_POINT('Ctrl Pts',(-42.2054524109828,4.06844583510791,10.4489096280657));
#20386=CARTESIAN_POINT('',(-43.4947552011066,0.675477606374448,9.34999999998968));
#20387=CARTESIAN_POINT('Origin',(0.,0.,9.34999999999998));
#20388=CARTESIAN_POINT('Ctrl Pts',(-42.3779453595728,0.399648641330075,
10.4701702229062));
#20389=CARTESIAN_POINT('Ctrl Pts',(-42.5817124486134,0.436868467021733,
10.2660612053923));
#20390=CARTESIAN_POINT('Ctrl Pts',(-42.7845757299537,0.480985891900656,
10.0627475751719));
#20391=CARTESIAN_POINT('Ctrl Pts',(-42.986507436847,0.531978227610498,9.86020040449869));
#20392=CARTESIAN_POINT('Ctrl Pts',(-43.1565918793884,0.574928406790011,
9.6895975648441));
#20393=CARTESIAN_POINT('Ctrl Pts',(-43.3260155112353,0.622756848243033,
9.51953800447573));
#20394=CARTESIAN_POINT('Ctrl Pts',(-43.4947552011066,0.675477606374445,
9.34999999998968));
#20395=CARTESIAN_POINT('Origin',(-1.73472347597681E-15,-1.73472347597681E-15,
11.35));
#20396=CARTESIAN_POINT('',(-5.00000000000001,14.142135623731,11.35));
#20397=CARTESIAN_POINT('',(5.,14.142135623731,11.35));
#20398=CARTESIAN_POINT('Origin',(-1.73472347597681E-15,-1.73472347597681E-15,
11.35));
#20399=CARTESIAN_POINT('',(5.,14.142135623731,-11.35));
#20400=CARTESIAN_POINT('',(5.,14.142135623731,11.35));
#20401=CARTESIAN_POINT('',(-5.00000000000001,14.142135623731,-11.35));
#20402=CARTESIAN_POINT('Origin',(-3.46944695195361E-15,1.73472347597681E-15,
-11.35));
#20403=CARTESIAN_POINT('',(-5.00000000000001,14.142135623731,11.35));
#20404=CARTESIAN_POINT('Origin',(-3.46944695195361E-15,3.46944695195361E-15,
-9.34999999999999));
#20405=CARTESIAN_POINT('',(42.3549304887758,1.97901608230145,-10.4488603766003));
#20406=CARTESIAN_POINT('',(42.3778559173176,-0.400053103664774,-10.4702558451011));
#20407=CARTESIAN_POINT('Ctrl Pts',(42.3778559173178,-0.400053103664613,
-10.470255845101));
#20408=CARTESIAN_POINT('Ctrl Pts',(42.3147058279902,-0.298272918361279,
-10.5343638976599));
#20409=CARTESIAN_POINT('Ctrl Pts',(42.2597977418668,-0.186602611546638,
-10.589958769092));
#20410=CARTESIAN_POINT('Ctrl Pts',(42.165574364121,0.0594627592708472,-10.6845737030941));
#20411=CARTESIAN_POINT('Ctrl Pts',(42.1277472101709,0.193934008724945,-10.7220376404442));
#20412=CARTESIAN_POINT('Ctrl Pts',(42.0583624188826,0.559734595935365,-10.788524357582));
#20413=CARTESIAN_POINT('Ctrl Pts',(42.046111502818,0.795598132314873,-10.7969991342825));
#20414=CARTESIAN_POINT('Ctrl Pts',(42.080062787682,1.20890695925822,-10.7529641474054));
#20415=CARTESIAN_POINT('Ctrl Pts',(42.1138804087149,1.38542074401615,-10.7136554733273));
#20416=CARTESIAN_POINT('Ctrl Pts',(42.2140750286918,1.70635615105641,-10.6017307219916));
#20417=CARTESIAN_POINT('Ctrl Pts',(42.2777622816001,1.85044081093512,-10.5319455628));
#20418=CARTESIAN_POINT('Ctrl Pts',(42.3549304887758,1.97901608230144,-10.4488603766003));
#20419=CARTESIAN_POINT('',(43.4947470521204,-0.676002124309743,-9.34999999999999));
#20420=CARTESIAN_POINT('Ctrl Pts',(42.3778559173176,-0.400053103664769,
-10.4702558451011));
#20421=CARTESIAN_POINT('Ctrl Pts',(42.581680861761,-0.437302204766713,-10.2660883608697));
#20422=CARTESIAN_POINT('Ctrl Pts',(42.7846012120674,-0.481452073895284,
-10.0627168613337));
#20423=CARTESIAN_POINT('Ctrl Pts',(42.9865892255721,-0.5324797140179,-9.86011239009894));
#20424=CARTESIAN_POINT('Ctrl Pts',(43.1566436205362,-0.575440057638944,
-9.68953899727716));
#20425=CARTESIAN_POINT('Ctrl Pts',(43.3260372643517,-0.623276250889277,
-9.51950878957767));
#20426=CARTESIAN_POINT('Ctrl Pts',(43.4947470521204,-0.676002124309744,
-9.35));
#20427=CARTESIAN_POINT('',(43.3203086503666,-3.94979220174698,-9.34999999999999));
#20428=CARTESIAN_POINT('Origin',(-3.46944695195361E-15,3.46944695195361E-15,
-9.34999999999999));
#20429=CARTESIAN_POINT('',(42.2054617208597,-4.06886253050386,-10.4488603765996));
#20430=CARTESIAN_POINT('Ctrl Pts',(43.3203086503666,-3.94979220174697,-9.34999999999999));
#20431=CARTESIAN_POINT('Ctrl Pts',(43.1122825236194,-3.98478982701022,-9.55398902691224));
#20432=CARTESIAN_POINT('Ctrl Pts',(42.9041475658189,-4.01262695712675,-9.75864153760776));
#20433=CARTESIAN_POINT('Ctrl Pts',(42.6959315890968,-4.03332628397407,-9.96398744092348));
#20434=CARTESIAN_POINT('Ctrl Pts',(42.5324864596819,-4.04957481690908,-10.1251796235343));
#20435=CARTESIAN_POINT('Ctrl Pts',(42.3689912631274,-4.06142404123509,-10.2867993162798));
#20436=CARTESIAN_POINT('Ctrl Pts',(42.2054617208598,-4.06886253050386,-10.4488603765996));
#20437=CARTESIAN_POINT('',(41.8895769551558,-6.42697885114752,-10.4702558450972));
#20438=CARTESIAN_POINT('Ctrl Pts',(42.2054617208598,-4.06886253050389,-10.4488603765996));
#20439=CARTESIAN_POINT('Ctrl Pts',(42.0931565705379,-4.20679248947824,-10.5474113287244));
#20440=CARTESIAN_POINT('Ctrl Pts',(41.996645286846,-4.36886244651051,-10.6271346454319));
#20441=CARTESIAN_POINT('Ctrl Pts',(41.8322466693354,-4.75204677305466,-10.7492419669034));
#20442=CARTESIAN_POINT('Ctrl Pts',(41.7715980988903,-4.97460297984299,-10.7838654920941));
#20443=CARTESIAN_POINT('Ctrl Pts',(41.7101624561659,-5.43269747180814,-10.788159089135));
#20444=CARTESIAN_POINT('Ctrl Pts',(41.7099416343871,-5.6639427088267,-10.7577973127672));
#20445=CARTESIAN_POINT('Ctrl Pts',(41.7673137310951,-6.07920795450595,-10.6430146790632));
#20446=CARTESIAN_POINT('Ctrl Pts',(41.8176243487664,-6.26256709540618,-10.5663096368479));
#20447=CARTESIAN_POINT('Ctrl Pts',(41.8895769551558,-6.42697885114752,-10.4702558450972));
#20448=CARTESIAN_POINT('',(42.9558281083822,-6.85906928986172,-9.34999999999999));
#20449=CARTESIAN_POINT('Ctrl Pts',(41.8895769551558,-6.42697885114752,-10.4702558450972));
#20450=CARTESIAN_POINT('Ctrl Pts',(42.0860261557596,-6.49285612411399,-10.266088360863));
#20451=CARTESIAN_POINT('Ctrl Pts',(42.2805978880048,-6.56543518807053,-10.0627168613241));
#20452=CARTESIAN_POINT('Ctrl Pts',(42.4732679644259,-6.64468933186833,-9.86011239008662));
#20453=CARTESIAN_POINT('Ctrl Pts',(42.635477556489,-6.7114136648501,-9.68953899726898));
#20454=CARTESIAN_POINT('Ctrl Pts',(42.796339217146,-6.78287018364921,-9.51950878957359));
#20455=CARTESIAN_POINT('Ctrl Pts',(42.9558281083822,-6.85906928986171,-9.34999999999999));
#20456=CARTESIAN_POINT('',(42.31725633263,-10.0747117317813,-9.34999999999999));
#20457=CARTESIAN_POINT('Origin',(-3.46944695195361E-15,3.46944695195361E-15,
-9.34999999999999));
#20458=CARTESIAN_POINT('',(41.1968114628114,-10.0339108357988,-10.4488603765985));
#20459=CARTESIAN_POINT('Ctrl Pts',(42.31725633263,-10.0747117317813,-9.34999999999999));
#20460=CARTESIAN_POINT('Ctrl Pts',(42.1063669305224,-10.079747927096,-9.55398902691493));
#20461=CARTESIAN_POINT('Ctrl Pts',(41.8963888498135,-10.0776810225061,-9.75864153761314));
#20462=CARTESIAN_POINT('Ctrl Pts',(41.6873463901567,-10.0685374369976,-9.96398744093155));
#20463=CARTESIAN_POINT('Ctrl Pts',(41.5232524891573,-10.0613599161357,-10.1251796235393));
#20464=CARTESIAN_POINT('Ctrl Pts',(41.3597351175228,-10.0498207399865,-10.2867993162818));
#20465=CARTESIAN_POINT('Ctrl Pts',(41.1968114628114,-10.0339108357988,-10.4488603765985));
#20466=CARTESIAN_POINT('',(40.548547005747,-12.3230698430749,-10.4702558451024));
#20467=CARTESIAN_POINT('Ctrl Pts',(41.1968114628111,-10.0339108357987,-10.4488603765988));
#20468=CARTESIAN_POINT('Ctrl Pts',(41.0660199366633,-10.1544541778436,-10.5474113291164));
#20469=CARTESIAN_POINT('Ctrl Pts',(40.9474260385374,-10.3011395093532,-10.6271346460638));
#20470=CARTESIAN_POINT('Ctrl Pts',(40.7301679463267,-10.6570272102986,-10.7492419673839));
#20471=CARTESIAN_POINT('Ctrl Pts',(40.6384636404816,-10.868686924454,-10.7838654923527));
#20472=CARTESIAN_POINT('Ctrl Pts',(40.5124596809018,-11.3133754715734,-10.7881590889262));
#20473=CARTESIAN_POINT('Ctrl Pts',(40.479331478489,-11.5422355392621,-10.7577973123347));
#20474=CARTESIAN_POINT('Ctrl Pts',(40.4770212041179,-11.9614388832522,-10.6430146784606));
#20475=CARTESIAN_POINT('Ctrl Pts',(40.5007250057626,-12.1500916390904,-10.566309636471));
#20476=CARTESIAN_POINT('Ctrl Pts',(40.5485470057468,-12.3230698430748,-10.4702558451027));
#20477=CARTESIAN_POINT('',(41.5424523787385,-12.9025055845851,-9.34999999999999));
#20478=CARTESIAN_POINT('Ctrl Pts',(40.548547005747,-12.3230698430749,-10.4702558451024));
#20479=CARTESIAN_POINT('Ctrl Pts',(40.7336213240881,-12.416234217002,-10.2660883599951));
#20480=CARTESIAN_POINT('Ctrl Pts',(40.9158835196664,-12.5157649757987,-10.0627168595901));
#20481=CARTESIAN_POINT('Ctrl Pts',(41.0953134525996,-12.6216322379599,-9.860112387496));
#20482=CARTESIAN_POINT('Ctrl Pts',(41.2463761214623,-12.7107622448981,-9.68953899554443));
#20483=CARTESIAN_POINT('Ctrl Pts',(41.395431118676,-12.8043844401388,-9.51950878871185));
#20484=CARTESIAN_POINT('Ctrl Pts',(41.5424523787385,-12.9025055845851,-9.34999999999999));
#20485=CARTESIAN_POINT('',(40.4527467088507,-15.9945391840333,-9.34999999999999));
#20486=CARTESIAN_POINT('Origin',(-3.46944695195361E-15,3.46944695195361E-15,
-9.34999999999999));
#20487=CARTESIAN_POINT('',(39.3495129251698,-15.7946976519001,-10.4488603766002));
#20488=CARTESIAN_POINT('Ctrl Pts',(40.4527467088507,-15.9945391840333,-9.34999999999999));
#20489=CARTESIAN_POINT('Ctrl Pts',(40.2432871314601,-15.9695114269873,-9.55398902691222));
#20490=CARTESIAN_POINT('Ctrl Pts',(40.0357404760446,-15.9375825639096,-9.7586415376077));
#20491=CARTESIAN_POINT('Ctrl Pts',(39.8301270351082,-15.8987822030802,-9.96398744092336));
#20492=CARTESIAN_POINT('Ctrl Pts',(39.6687248411344,-15.8683247420489,-10.1251796235344));
#20493=CARTESIAN_POINT('Ctrl Pts',(39.5085140365547,-15.8336320697752,-10.2867993162802));
#20494=CARTESIAN_POINT('Ctrl Pts',(39.3495129251698,-15.7946976519002,-10.4488603766002));
#20495=CARTESIAN_POINT('',(38.3820655716558,-17.9682986698111,-10.4702558451043));
#20496=CARTESIAN_POINT('Ctrl Pts',(39.3495129251697,-15.7946976518998,-10.4488603766004));
#20497=CARTESIAN_POINT('Ctrl Pts',(39.2028975619447,-15.8954004616404,-10.5474113291176));
#20498=CARTESIAN_POINT('Ctrl Pts',(39.064635279473,-16.0237150765457,-10.6271346460648));
#20499=CARTESIAN_POINT('Ctrl Pts',(38.7989404607774,-16.3450613035865,-10.7492419673849));
#20500=CARTESIAN_POINT('Ctrl Pts',(38.6780472545499,-16.5415157435849,-10.7838654923536));
#20501=CARTESIAN_POINT('Ctrl Pts',(38.4900400549303,-16.9637457693538,-10.7881590889271));
#20502=CARTESIAN_POINT('Ctrl Pts',(38.4246788663307,-17.185561736774,-10.7577973123357));
#20503=CARTESIAN_POINT('Ctrl Pts',(38.3627332511181,-17.60016940884,-10.6430146784615));
#20504=CARTESIAN_POINT('Ctrl Pts',(38.3593476958032,-17.7902753543356,-10.5663096364721));
#20505=CARTESIAN_POINT('Ctrl Pts',(38.3820655716563,-17.9682986698106,-10.470255845104));
#20506=CARTESIAN_POINT('',(39.2833921172024,-18.6832840733669,-9.34999999999999));
#20507=CARTESIAN_POINT('Ctrl Pts',(38.3820655716558,-17.9682986698111,-10.4702558451043));
#20508=CARTESIAN_POINT('Ctrl Pts',(38.5519974274795,-18.0868535864241,-10.2660883600012));
#20509=CARTESIAN_POINT('Ctrl Pts',(38.7182397528624,-18.211309880492,-10.0627168596004));
#20510=CARTESIAN_POINT('Ctrl Pts',(38.8807768654989,-18.341635108456,-9.86011238751062));
#20511=CARTESIAN_POINT('Ctrl Pts',(39.0176174116884,-18.4513563597297,-9.68953899555414));
#20512=CARTESIAN_POINT('Ctrl Pts',(39.1518314163795,-18.5652383538402,-9.51950878871669));
#20513=CARTESIAN_POINT('Ctrl Pts',(39.2833921172024,-18.6832840733669,-9.35));
#20514=CARTESIAN_POINT('',(37.7647358181625,-21.5887639429495,-9.34999999999999));
#20515=CARTESIAN_POINT('Origin',(-3.46944695195361E-15,3.46944695195361E-15,
-9.34999999999999));
#20516=CARTESIAN_POINT('',(36.7011717789887,-21.233949971968,-10.4488603766022));
#20517=CARTESIAN_POINT('Ctrl Pts',(37.7647358181625,-21.5887639429495,-9.34999999999999));
#20518=CARTESIAN_POINT('Ctrl Pts',(37.5609700584511,-21.5341817265036,-9.55398902691086));
#20519=CARTESIAN_POINT('Ctrl Pts',(37.3600798797159,-21.4730408845162,-9.75864153760501));
#20520=CARTESIAN_POINT('Ctrl Pts',(37.1620811542153,-21.4053736118224,-9.96398744091935));
#20521=CARTESIAN_POINT('Ctrl Pts',(37.0066563504919,-21.3522562366961,-10.1251796235324));
#20522=CARTESIAN_POINT('Ctrl Pts',(36.8530135429395,-21.2951163110601,-10.2867993162802));
#20523=CARTESIAN_POINT('Ctrl Pts',(36.7011717789887,-21.233949971968,-10.4488603766022));
#20524=CARTESIAN_POINT('',(35.4342359672589,-23.2477447519415,-10.4702558450997));
#20525=CARTESIAN_POINT('Ctrl Pts',(36.7011717789887,-21.233949971968,-10.4488603766022));
#20526=CARTESIAN_POINT('Ctrl Pts',(36.5417172446773,-21.3127622306018,-10.5474113291192));
#20527=CARTESIAN_POINT('Ctrl Pts',(36.386601199215,-21.4200940133731,-10.6271346460661));
#20528=CARTESIAN_POINT('Ctrl Pts',(36.0778784343425,-21.7003570840141,-10.7492419673852));
#20529=CARTESIAN_POINT('Ctrl Pts',(35.9302573647846,-21.8776070039851,-10.7838654923534));
#20530=CARTESIAN_POINT('Ctrl Pts',(35.6840742095426,-22.2687831226896,-10.7881590889257));
#20531=CARTESIAN_POINT('Ctrl Pts',(35.5878106000705,-22.479039456409,-10.7577973123336));
#20532=CARTESIAN_POINT('Ctrl Pts',(35.4674906781066,-22.8806112399779,-10.6430146784584));
#20533=CARTESIAN_POINT('Ctrl Pts',(35.4370846859756,-23.0683003663016,-10.5663096364684));
#20534=CARTESIAN_POINT('Ctrl Pts',(35.4342359672589,-23.2477447519415,-10.4702558450997));
#20535=CARTESIAN_POINT('',(36.2246352761032,-24.0837247765644,-9.34999999999999));
#20536=CARTESIAN_POINT('Ctrl Pts',(35.4342359672589,-23.2477447519415,-10.4702558450997));
#20537=CARTESIAN_POINT('Ctrl Pts',(35.585566038032,-23.3892767750272,-10.2660883599914));
#20538=CARTESIAN_POINT('Ctrl Pts',(35.7324042788861,-23.5361250331267,-10.0627168595854));
#20539=CARTESIAN_POINT('Ctrl Pts',(35.8747397843386,-23.6882551810849,-9.86011238749032));
#20540=CARTESIAN_POINT('Ctrl Pts',(35.9945725289411,-23.81633406842,-9.68953899554068));
#20541=CARTESIAN_POINT('Ctrl Pts',(36.1112133310069,-23.9481575524003,-9.51950878870999));
#20542=CARTESIAN_POINT('Ctrl Pts',(36.2246352761032,-24.0837247765644,-9.34999999999999));
#20543=CARTESIAN_POINT('',(34.3079438107283,-26.7435037248284,-9.34999999999999));
#20544=CARTESIAN_POINT('Origin',(-3.46944695195361E-15,3.46944695195361E-15,
-9.34999999999999));
#20545=CARTESIAN_POINT('',(33.3057006128401,-26.240940304242,-10.4488603766015));
#20546=CARTESIAN_POINT('Ctrl Pts',(34.3079438107283,-26.7435037248284,-9.34999999999999));
#20547=CARTESIAN_POINT('Ctrl Pts',(34.1140199519477,-26.6604781855038,-9.55398902691468));
#20548=CARTESIAN_POINT('Ctrl Pts',(33.9238757946085,-26.5713700158305,-9.75864153761266));
#20549=CARTESIAN_POINT('Ctrl Pts',(33.7375224676096,-26.4762133418042,-9.96398744093084));
#20550=CARTESIAN_POINT('Ctrl Pts',(33.5912390549387,-26.4015173691637,-10.1251796235398));
#20551=CARTESIAN_POINT('Ctrl Pts',(33.4472919689122,-26.3230933942746,-10.2867993162836));
#20552=CARTESIAN_POINT('Ctrl Pts',(33.3057006128402,-26.240940304242,-10.4488603766015));
#20553=CARTESIAN_POINT('',(31.7650675024754,-28.0539337918554,-10.4702558451018));
#20554=CARTESIAN_POINT('Ctrl Pts',(33.3057006128397,-26.2409403042424,-10.4488603766016));
#20555=CARTESIAN_POINT('Ctrl Pts',(33.1366529419318,-26.2962576214585,-10.5474113291188));
#20556=CARTESIAN_POINT('Ctrl Pts',(32.9678408488468,-26.380421606517,-10.6271346460658));
#20557=CARTESIAN_POINT('Ctrl Pts',(32.6223748430073,-26.6138961728501,-10.7492419673852));
#20558=CARTESIAN_POINT('Ctrl Pts',(32.4510310493911,-26.7683332755687,-10.7838654923535));
#20559=CARTESIAN_POINT('Ctrl Pts',(32.1516835176331,-27.1204922694895,-10.7881590889263));
#20560=CARTESIAN_POINT('Ctrl Pts',(32.0264771367756,-27.3149087568822,-10.7577973123345));
#20561=CARTESIAN_POINT('Ctrl Pts',(31.8502322746963,-27.6952698084771,-10.6430146784599));
#20562=CARTESIAN_POINT('Ctrl Pts',(31.7934248240649,-27.8767213062674,-10.5663096364702));
#20563=CARTESIAN_POINT('Ctrl Pts',(31.7650675024754,-28.0539337918554,-10.4702558451019));
#20564=CARTESIAN_POINT('',(32.428449324012,-28.9938902950258,-9.34999999999999));
#20565=CARTESIAN_POINT('Ctrl Pts',(31.7650675024754,-28.0539337918554,-10.4702558451018));
#20566=CARTESIAN_POINT('Ctrl Pts',(31.8947151443511,-28.2155617375662,-10.2660883599943));
#20567=CARTESIAN_POINT('Ctrl Pts',(32.0191600975335,-28.3818125526352,-10.0627168595892));
#20568=CARTESIAN_POINT('Ctrl Pts',(32.1383964553672,-28.5526506894797,-9.86011238749498));
#20569=CARTESIAN_POINT('Ctrl Pts',(32.2387819492775,-28.6964798960859,-9.68953899554376));
#20570=CARTESIAN_POINT('Ctrl Pts',(32.3354750783575,-28.843561323957,-9.51950878871151));
#20571=CARTESIAN_POINT('Ctrl Pts',(32.428449324012,-28.9938902950258,-9.35));
#20572=CARTESIAN_POINT('',(30.15274100324,-31.3538228927755,-9.34999999999999));
#20573=CARTESIAN_POINT('Origin',(-3.46944695195361E-15,3.46944695195361E-15,
-9.34999999999999));
#20574=CARTESIAN_POINT('',(29.2322214279089,-30.7137407645584,-10.4488603766032));
#20575=CARTESIAN_POINT('Ctrl Pts',(30.15274100324,-31.3538228927755,-9.34999999999999));
#20576=CARTESIAN_POINT('Ctrl Pts',(29.9726067759282,-31.2440441911298,-9.55398902691379));
#20577=CARTESIAN_POINT('Ctrl Pts',(29.7970794267014,-31.1287826791412,-9.75864153761091));
#20578=CARTESIAN_POINT('Ctrl Pts',(29.6261651145468,-31.0080737192595,-9.96398744092823));
#20579=CARTESIAN_POINT('Ctrl Pts',(29.4920010013578,-30.9133197437011,-10.1251796235386));
#20580=CARTESIAN_POINT('Ctrl Pts',(29.360679984414,-30.8152082055302,-10.2867993162838));
#20581=CARTESIAN_POINT('Ctrl Pts',(29.232221427909,-30.7137407645584,-10.4488603766032));
#20582=CARTESIAN_POINT('',(27.4492538662204,-32.2890256406531,-10.4702558450977));
#20583=CARTESIAN_POINT('Ctrl Pts',(29.232221427909,-30.7137407645579,-10.4488603766035));
#20584=CARTESIAN_POINT('Ctrl Pts',(29.0570219434909,-30.7444370393004,-10.5474113291203));
#20585=CARTESIAN_POINT('Ctrl Pts',(28.8779503301844,-30.8037198906201,-10.627134646067));
#20586=CARTESIAN_POINT('Ctrl Pts',(28.5027737750148,-30.9856530837616,-10.7492419673855));
#20587=CARTESIAN_POINT('Ctrl Pts',(28.3111953228635,-31.1141334751775,-10.7838654923533));
#20588=CARTESIAN_POINT('Ctrl Pts',(27.9647772670893,-31.4201064027429,-10.7881590889249));
#20589=CARTESIAN_POINT('Ctrl Pts',(27.8131769556956,-31.5947252847772,-10.7577973123325));
#20590=CARTESIAN_POINT('Ctrl Pts',(27.5845949906459,-31.9461325502595,-10.6430146784567));
#20591=CARTESIAN_POINT('Ctrl Pts',(27.5025425173903,-32.1176525902846,-10.5663096364665));
#20592=CARTESIAN_POINT('Ctrl Pts',(27.4492538662209,-32.2890256406529,-10.4702558450976));
#20593=CARTESIAN_POINT('',(27.9721136596011,-33.3138238185646,-9.34999999999999));
#20594=CARTESIAN_POINT('Ctrl Pts',(27.4492538662204,-32.2890256406531,-10.4702558450977));
#20595=CARTESIAN_POINT('Ctrl Pts',(27.5545798270844,-32.46745923011,-10.2660883599907));
#20596=CARTESIAN_POINT('Ctrl Pts',(27.6540981522194,-32.6497282149806,-10.062716859586));
#20597=CARTESIAN_POINT('Ctrl Pts',(27.7478080540396,-32.8357965689006,-9.86011238749213));
#20598=CARTESIAN_POINT('Ctrl Pts',(27.8267027380888,-32.9924481468975,-9.68953899554188));
#20599=CARTESIAN_POINT('Ctrl Pts',(27.9014798009146,-33.1517933649324,-9.51950878871058));
#20600=CARTESIAN_POINT('Ctrl Pts',(27.9721136596011,-33.3138238185646,-9.34999999999999));
#20601=CARTESIAN_POINT('',(25.3837153422573,-35.325868643577,-9.34999999999999));
#20602=CARTESIAN_POINT('Origin',(-3.46944695195361E-15,3.46944695195361E-15,
-9.34999999999999));
#20603=CARTESIAN_POINT('',(24.5636585134848,-34.5612980340113,-10.4488603766026));
#20604=CARTESIAN_POINT('Ctrl Pts',(25.3837153422573,-35.325868643577,-9.34999999999999));
#20605=CARTESIAN_POINT('Ctrl Pts',(25.2210377598187,-35.1915715573989,-9.55398902691333));
#20606=CARTESIAN_POINT('Ctrl Pts',(25.063700449356,-35.0525030950913,-9.75864153760996));
#20607=CARTESIAN_POINT('Ctrl Pts',(24.9117044745655,-34.9086991356805,-9.9639874409268));
#20608=CARTESIAN_POINT('Ctrl Pts',(24.7923908553075,-34.7958160748984,-10.1251796235375));
#20609=CARTESIAN_POINT('Ctrl Pts',(24.6763692246546,-34.6800142414323,-10.2867993162829));
#20610=CARTESIAN_POINT('Ctrl Pts',(24.5636585134848,-34.5612980340113,-10.4488603766026));
#20611=CARTESIAN_POINT('',(22.5746525783699,-35.8668060412517,-10.470255845099));
#20612=CARTESIAN_POINT('Ctrl Pts',(24.563658513485,-34.5612980340106,-10.448860376603));
#20613=CARTESIAN_POINT('Ctrl Pts',(24.3858737718256,-34.566748378646,-10.5474113291201));
#20614=CARTESIAN_POINT('Ctrl Pts',(24.2001880199446,-34.5999432683309,-10.6271346460669));
#20615=CARTESIAN_POINT('Ctrl Pts',(23.802938428188,-34.7266314531191,-10.7492419673858));
#20616=CARTESIAN_POINT('Ctrl Pts',(23.5950253023206,-34.8265396429691,-10.7838654923538));
#20617=CARTESIAN_POINT('Ctrl Pts',(23.2085887951579,-35.0800977777257,-10.7881590889258));
#20618=CARTESIAN_POINT('Ctrl Pts',(23.0336806983883,-35.2313643175223,-10.7577973123335));
#20619=CARTESIAN_POINT('Ctrl Pts',(22.7574148999991,-35.5466641583413,-10.643014678458));
#20620=CARTESIAN_POINT('Ctrl Pts',(22.6517877558542,-35.7047610872093,-10.5663096364679));
#20621=CARTESIAN_POINT('Ctrl Pts',(22.5746525783699,-35.8668060412516,-10.470255845099));
#20622=CARTESIAN_POINT('',(22.9463464260018,-36.9555839582859,-9.34999999999999));
#20623=CARTESIAN_POINT('Ctrl Pts',(22.5746525783699,-35.8668060412517,-10.4702558450989));
#20624=CARTESIAN_POINT('Ctrl Pts',(22.6535127253941,-36.0584128811362,-10.26608835999));
#20625=CARTESIAN_POINT('Ctrl Pts',(22.7260785163689,-36.2529895648998,-10.0627168595834));
#20626=CARTESIAN_POINT('Ctrl Pts',(22.7923542988114,-36.4505003207895,-9.86011238748777));
#20627=CARTESIAN_POINT('Ctrl Pts',(22.848152104745,-36.6167852957953,-9.68953899553898));
#20628=CARTESIAN_POINT('Ctrl Pts',(22.8994908559558,-36.7851504948688,-9.51950878870914));
#20629=CARTESIAN_POINT('Ctrl Pts',(22.9463464260018,-36.9555839582859,-9.34999999999999));
#20630=CARTESIAN_POINT('',(20.0979504375088,-38.5787815801827,-9.34999999999999));
#20631=CARTESIAN_POINT('Origin',(-3.46944695195361E-15,3.46944695195361E-15,
-9.34999999999999));
#20632=CARTESIAN_POINT('',(19.3950503474966,-37.7052869420423,-10.4488603765928));
#20633=CARTESIAN_POINT('Ctrl Pts',(20.0979504375088,-38.5787815801827,-9.34999999999999));
#20634=CARTESIAN_POINT('Ctrl Pts',(19.9560411463964,-38.4227000108602,-9.55398902691918));
#20635=CARTESIAN_POINT('Ctrl Pts',(19.8200968086136,-38.2626556310799,-9.75864153762166));
#20636=CARTESIAN_POINT('Ctrl Pts',(19.690113370912,-38.0986841060511,-9.96398744094433));
#20637=CARTESIAN_POINT('Ctrl Pts',(19.588079126809,-37.9699699336414,-10.125179623546));
#20638=CARTESIAN_POINT('Ctrl Pts',(19.4897187482756,-37.8388351962714,-10.2867993162823));
#20639=CARTESIAN_POINT('Ctrl Pts',(19.3950503474966,-37.7052869420423,-10.4488603765928));
#20640=CARTESIAN_POINT('',(17.2404964639731,-38.7144417021608,-10.470255845106));
#20641=CARTESIAN_POINT('Ctrl Pts',(19.3950503474966,-37.7052869420422,-10.4488603765929));
#20642=CARTESIAN_POINT('Ctrl Pts',(19.2182995332483,-37.6853804032696,-10.5474113291113));
#20643=CARTESIAN_POINT('Ctrl Pts',(19.029779669228,-37.6918115790903,-10.6271346460595));
#20644=CARTESIAN_POINT('Ctrl Pts',(18.6185438970004,-37.7606757494185,-10.7492419673812));
#20645=CARTESIAN_POINT('Ctrl Pts',(18.398528609088,-37.8299778950671,-10.7838654923508));
#20646=CARTESIAN_POINT('Ctrl Pts',(17.9799403834319,-38.0259595245895,-10.7881590889263));
#20647=CARTESIAN_POINT('Ctrl Pts',(17.7852851257429,-38.1507943716133,-10.7577973123358));
#20648=CARTESIAN_POINT('Ctrl Pts',(17.4669594689832,-38.4235681922572,-10.6430146784635));
#20649=CARTESIAN_POINT('Ctrl Pts',(17.3399079179993,-38.5650236124094,-10.5663096364746));
#20650=CARTESIAN_POINT('Ctrl Pts',(17.2404964639731,-38.7144417021598,-10.4702558451068));
#20651=CARTESIAN_POINT('',(17.4534577509835,-39.8450349797141,-9.34999999999999));
#20652=CARTESIAN_POINT('Ctrl Pts',(17.2404964639731,-38.7144417021608,-10.470255845106));
#20653=CARTESIAN_POINT('Ctrl Pts',(17.2912854319751,-38.9153212297603,-10.2660883599972));
#20654=CARTESIAN_POINT('Ctrl Pts',(17.3354214585452,-39.1182445922472,-10.0627168595908));
#20655=CARTESIAN_POINT('Ctrl Pts',(17.3729139378,-39.3231770006896,-9.86011238749544));
#20656=CARTESIAN_POINT('Ctrl Pts',(17.4044789831962,-39.4957102901439,-9.68953899554403));
#20657=CARTESIAN_POINT('Ctrl Pts',(17.4313343138652,-39.6696680403328,-9.51950878871163));
#20658=CARTESIAN_POINT('Ctrl Pts',(17.4534577509835,-39.8450349797141,-9.34999999999999));
#20659=CARTESIAN_POINT('',(14.4030492195297,-41.046341775849,-9.34999999999999));
#20660=CARTESIAN_POINT('Origin',(-3.46944695195361E-15,3.46944695195361E-15,
-9.34999999999999));
#20661=CARTESIAN_POINT('',(13.8316148870825,-40.0817049410147,-10.4488603765993));
#20662=CARTESIAN_POINT('Ctrl Pts',(14.4030492195297,-41.046341775849,-9.34999999999999));
#20663=CARTESIAN_POINT('Ctrl Pts',(14.2847970836793,-40.8716530940395,-9.55398902691715));
#20664=CARTESIAN_POINT('Ctrl Pts',(14.1730131532637,-40.6938908388371,-9.75864153761761));
#20665=CARTESIAN_POINT('Ctrl Pts',(14.0676883406023,-40.5130897355934,-9.96398744093829));
#20666=CARTESIAN_POINT('Ctrl Pts',(13.9850105946094,-40.3711647009173,-10.125179623544));
#20667=CARTESIAN_POINT('Ctrl Pts',(13.906313801843,-40.2273665847263,-10.2867993162846));
#20668=CARTESIAN_POINT('Ctrl Pts',(13.8316148870826,-40.0817049410147,-10.4488603765992));
#20669=CARTESIAN_POINT('',(11.5553735590042,-40.7739629732828,-10.4702558451002));
#20670=CARTESIAN_POINT('Ctrl Pts',(13.8316148870824,-40.0817049410149,-10.4488603765991));
#20671=CARTESIAN_POINT('Ctrl Pts',(13.6594961371153,-40.036846758561,-10.5474113291163));
#20672=CARTESIAN_POINT('Ctrl Pts',(13.4719798817408,-40.0163833003267,-10.6271346460633));
#20673=CARTESIAN_POINT('Ctrl Pts',(13.0551295034576,-40.0260215802802,-10.749241967383));
#20674=CARTESIAN_POINT('Ctrl Pts',(12.8274909302894,-40.0633068898959,-10.7838654923515));
#20675=CARTESIAN_POINT('Ctrl Pts',(12.385272235305,-40.1977223933772,-10.7881590889245));
#20676=CARTESIAN_POINT('Ctrl Pts',(12.1748324364042,-40.2935842701396,-10.7577973123327));
#20677=CARTESIAN_POINT('Ctrl Pts',(11.8209271136738,-40.5182791822383,-10.6430146784582));
#20678=CARTESIAN_POINT('Ctrl Pts',(11.6750375590451,-40.6402134692447,-10.5663096364687));
#20679=CARTESIAN_POINT('Ctrl Pts',(11.5553735590047,-40.7739629732822,-10.4702558451006));
#20680=CARTESIAN_POINT('',(11.6052670077404,-41.9233559925617,-9.34999999999999));
#20681=CARTESIAN_POINT('Ctrl Pts',(11.5553735590042,-40.7739629732828,-10.4702558451002));
#20682=CARTESIAN_POINT('Ctrl Pts',(11.5770574310621,-40.980025860697,-10.2660883599968));
#20683=CARTESIAN_POINT('Ctrl Pts',(11.5918652110079,-41.1871649674224,-10.0627168595958));
#20684=CARTESIAN_POINT('Ctrl Pts',(11.5998111483213,-41.3953471955505,-9.86011238750566));
#20685=CARTESIAN_POINT('Ctrl Pts',(11.6065008598849,-41.5706165192242,-9.68953899555085));
#20686=CARTESIAN_POINT('Ctrl Pts',(11.6083260729273,-41.7466255423864,-9.51950878871505));
#20687=CARTESIAN_POINT('Ctrl Pts',(11.6052670077404,-41.9233559925616,-9.34999999999999));
#20688=CARTESIAN_POINT('',(8.41494345441915,-42.6783168208275,-9.34999999999999));
#20689=CARTESIAN_POINT('Origin',(-3.46944695195361E-15,3.46944695195361E-15,
-9.34999999999999));
#20690=CARTESIAN_POINT('',(7.98660763467823,-41.642175013475,-10.4488603765986));
#20691=CARTESIAN_POINT('Ctrl Pts',(8.41494345441915,-42.6783168208275,-9.34999999999999));
#20692=CARTESIAN_POINT('Ctrl Pts',(8.3227557463064,-42.4885771843301,-9.55398902691651));
#20693=CARTESIAN_POINT('Ctrl Pts',(8.23740782172385,-42.2967157805956,-9.75864153761634));
#20694=CARTESIAN_POINT('Ctrl Pts',(8.15888574355747,-42.1027656882098,-9.96398744093637));
#20695=CARTESIAN_POINT('Ctrl Pts',(8.09724757616397,-41.9505189756976,-10.1251796235425));
#20696=CARTESIAN_POINT('Ctrl Pts',(8.03981640892606,-41.7969847956541,-10.2867993162835));
#20697=CARTESIAN_POINT('Ctrl Pts',(7.98660763467823,-41.642175013475,-10.4488603765986));
#20698=CARTESIAN_POINT('',(5.63501657134564,-42.0034439406514,-10.4702558450999));
#20699=CARTESIAN_POINT('Ctrl Pts',(7.98660763467821,-41.6421750134749,-10.4488603765987));
#20700=CARTESIAN_POINT('Ctrl Pts',(7.8226247910452,-41.5732783708473,-10.5474113287234));
#20701=CARTESIAN_POINT('Ctrl Pts',(7.63992943532065,-41.5263368556522,-10.6271346454309));
#20702=CARTESIAN_POINT('Ctrl Pts',(7.22595032355027,-41.4765530373371,-10.749241966903));
#20703=CARTESIAN_POINT('Ctrl Pts',(6.99532253008204,-41.4810624893143,-10.7838654920941));
#20704=CARTESIAN_POINT('Ctrl Pts',(6.53847566308335,-41.5511755542865,-10.7881590891358));
#20705=CARTESIAN_POINT('Ctrl Pts',(6.31653527029745,-41.6161129892238,-10.7577973127683));
#20706=CARTESIAN_POINT('Ctrl Pts',(5.93425477237866,-41.7881548523286,-10.643014679065));
#20707=CARTESIAN_POINT('Ctrl Pts',(5.7724971039899,-41.888085776068,-10.5663096368503));
#20708=CARTESIAN_POINT('Ctrl Pts',(5.6350165713459,-42.0034439406511,-10.4702558451003));
#20709=CARTESIAN_POINT('',(5.52082649506268,-43.1482383743695,-9.34999999999999));
#20710=CARTESIAN_POINT('Ctrl Pts',(5.63501657134564,-42.0034439406514,-10.4702558450999));
#20711=CARTESIAN_POINT('Ctrl Pts',(5.62715392638841,-42.2104953408534,-10.2660883608659));
#20712=CARTESIAN_POINT('Ctrl Pts',(5.61233201610448,-42.4176334360682,-10.0627168613273));
#20713=CARTESIAN_POINT('Ctrl Pts',(5.59056965525696,-42.6248274931923,-9.86011239009003));
#20714=CARTESIAN_POINT('Ctrl Pts',(5.57224784970726,-42.7992648739654,-9.68953899727123));
#20715=CARTESIAN_POINT('Ctrl Pts',(5.5490057889544,-42.9737421348353,-9.5195087895747));
#20716=CARTESIAN_POINT('Ctrl Pts',(5.52082649506267,-43.1482383743695,-9.34999999999999));
#20717=CARTESIAN_POINT('',(2.25553370726644,-43.4414844094374,-9.34999999999999));
#20718=CARTESIAN_POINT('Origin',(-3.46944695195361E-15,3.46944695195361E-15,
-9.34999999999999));
#20719=CARTESIAN_POINT('',(1.97901608230067,-42.3549304887752,-10.4488603766009));
#20720=CARTESIAN_POINT('Ctrl Pts',(2.25553370726645,-43.4414844094374,-9.34999999999999));
#20721=CARTESIAN_POINT('Ctrl Pts',(2.19128710278197,-43.2405563700915,-9.55398902691157));
#20722=CARTESIAN_POINT('Ctrl Pts',(2.13411262165437,-43.0385015627268,-9.75864153760641));
#20723=CARTESIAN_POINT('Ctrl Pts',(2.08399176105578,-42.8353507457784,-9.96398744092143));
#20724=CARTESIAN_POINT('Ctrl Pts',(2.04464794759835,-42.6758816594482,-10.1251796235333));
#20725=CARTESIAN_POINT('Ctrl Pts',(2.00965153883474,-42.5157369286965,-10.28679931628));
#20726=CARTESIAN_POINT('Ctrl Pts',(1.97901608230068,-42.3549304887753,-10.4488603766009));
#20727=CARTESIAN_POINT('',(-0.400053103665653,-42.3778559173192,-10.4702558450996));
#20728=CARTESIAN_POINT('Ctrl Pts',(1.97901608230066,-42.3549304887753,-10.4488603766009));
#20729=CARTESIAN_POINT('Ctrl Pts',(1.82650736151775,-42.2633979223932,-10.5474113291179));
#20730=CARTESIAN_POINT('Ctrl Pts',(1.65235205445741,-42.1909339439257,-10.6271346460647));
#20731=CARTESIAN_POINT('Ctrl Pts',(1.24967162819108,-42.0827414829252,-10.749241967384));
#20732=CARTESIAN_POINT('Ctrl Pts',(1.02074953110195,-42.0543832782663,-10.7838654923523));
#20733=CARTESIAN_POINT('Ctrl Pts',(0.558574576988531,-42.0587666057809,
-10.7881590889248));
#20734=CARTESIAN_POINT('Ctrl Pts',(0.329651656930575,-42.0914576603666,
-10.7577973123328));
#20735=CARTESIAN_POINT('Ctrl Pts',(-0.0732218856486514,-42.2073441982801,
-10.6430146784578));
#20736=CARTESIAN_POINT('Ctrl Pts',(-0.247554746683549,-42.2832374526635,
-10.5663096364682));
#20737=CARTESIAN_POINT('Ctrl Pts',(-0.400053103665666,-42.3778559173188,
-10.4702558451));
#20738=CARTESIAN_POINT('',(-0.676002124309578,-43.4947470521203,-9.34999999999999));
#20739=CARTESIAN_POINT('Ctrl Pts',(-0.400053103665649,-42.3778559173192,
-10.4702558450996));
#20740=CARTESIAN_POINT('Ctrl Pts',(-0.437302204927433,-42.5816808626376,
-10.2660883599915));
#20741=CARTESIAN_POINT('Ctrl Pts',(-0.481452074275132,-42.7846012138114,
-10.0627168595858));
#20742=CARTESIAN_POINT('Ctrl Pts',(-0.532479714674941,-42.9865892281722,
-9.86011238749097));
#20743=CARTESIAN_POINT('Ctrl Pts',(-0.575440058127383,-43.1566436222658,
-9.6895389955411));
#20744=CARTESIAN_POINT('Ctrl Pts',(-0.623276251159064,-43.326037265215,
-9.51950878871019));
#20745=CARTESIAN_POINT('Ctrl Pts',(-0.676002124309579,-43.4947470521204,
-9.34999999999999));
#20746=CARTESIAN_POINT('',(-3.9497922017429,-43.3203086503669,-9.34999999999999));
#20747=CARTESIAN_POINT('Origin',(-3.46944695195361E-15,3.46944695195361E-15,
-9.34999999999999));
#20748=CARTESIAN_POINT('',(-4.06886253049728,-42.2054617208604,-10.4488603765996));
#20749=CARTESIAN_POINT('Ctrl Pts',(-3.94979220174291,-43.3203086503669,
-9.34999999999999));
#20750=CARTESIAN_POINT('Ctrl Pts',(-3.98478982700535,-43.1122825236215,
-9.55398902691055));
#20751=CARTESIAN_POINT('Ctrl Pts',(-4.01262695712122,-42.9041475658228,
-9.75864153760437));
#20752=CARTESIAN_POINT('Ctrl Pts',(-4.03332628396802,-42.6959315891025,
-9.96398744091835));
#20753=CARTESIAN_POINT('Ctrl Pts',(-4.04957481690293,-42.5324864596859,
-10.1251796235308));
#20754=CARTESIAN_POINT('Ctrl Pts',(-4.06142404122876,-42.3689912631297,
-10.2867993162781));
#20755=CARTESIAN_POINT('Ctrl Pts',(-4.06886253049727,-42.2054617208604,
-10.4488603765996));
#20756=CARTESIAN_POINT('',(-6.42697885114042,-41.8895769551537,-10.4702558451003));
#20757=CARTESIAN_POINT('Ctrl Pts',(-4.06886253049729,-42.2054617208604,
-10.4488603765996));
#20758=CARTESIAN_POINT('Ctrl Pts',(-4.20679249002057,-42.0931565700915,
-10.5474113291167));
#20759=CARTESIAN_POINT('Ctrl Pts',(-4.36886244778991,-41.9966452860815,
-10.6271346460636));
#20760=CARTESIAN_POINT('Ctrl Pts',(-4.75204677534415,-41.8322466685932,
-10.7492419673832));
#20761=CARTESIAN_POINT('Ctrl Pts',(-4.97460298225344,-41.771598098344,-10.7838654923517));
#20762=CARTESIAN_POINT('Ctrl Pts',(-5.43269747428145,-41.7101624560557,
-10.7881590889246));
#20763=CARTESIAN_POINT('Ctrl Pts',(-5.66394271123907,-41.7099416344971,
-10.7577973123328));
#20764=CARTESIAN_POINT('Ctrl Pts',(-6.07920795595195,-41.7673137314921,
-10.6430146784582));
#20765=CARTESIAN_POINT('Ctrl Pts',(-6.2625670960526,-41.817624349051,-10.5663096364686));
#20766=CARTESIAN_POINT('Ctrl Pts',(-6.42697885114042,-41.8895769551538,
-10.4702558451003));
#20767=CARTESIAN_POINT('',(-6.85906928985839,-42.9558281083827,-9.34999999999999));
#20768=CARTESIAN_POINT('Ctrl Pts',(-6.42697885114041,-41.8895769551537,
-10.4702558451003));
#20769=CARTESIAN_POINT('Ctrl Pts',(-6.49285612438891,-42.0860261565974,
-10.2660883599931));
#20770=CARTESIAN_POINT('Ctrl Pts',(-6.56543518868484,-42.2805978896664,
-10.0627168595883));
#20771=CARTESIAN_POINT('Ctrl Pts',(-6.64468933287768,-42.4732679668919,
-9.86011238749433));
#20772=CARTESIAN_POINT('Ctrl Pts',(-6.71141366557098,-42.6354775581222,
-9.68953899554333));
#20773=CARTESIAN_POINT('Ctrl Pts',(-6.78287018403301,-42.7963392179579,
-9.51950878871131));
#20774=CARTESIAN_POINT('Ctrl Pts',(-6.85906928985838,-42.9558281083827,
-9.34999999999999));
#20775=CARTESIAN_POINT('',(-10.074711731795,-42.3172563326267,-9.34999999999999));
#20776=CARTESIAN_POINT('Origin',(-3.46944695195361E-15,3.46944695195361E-15,
-9.34999999999999));
#20777=CARTESIAN_POINT('',(-10.0339108358238,-41.1968114627984,-10.4488603766053));
#20778=CARTESIAN_POINT('Ctrl Pts',(-10.074711731795,-42.3172563326267,-9.34999999999999));
#20779=CARTESIAN_POINT('Ctrl Pts',(-10.0797479271121,-42.1063669305242,
-9.55398902690942));
#20780=CARTESIAN_POINT('Ctrl Pts',(-10.0776810225247,-41.8963888498204,
-9.75864153760213));
#20781=CARTESIAN_POINT('Ctrl Pts',(-10.0685374370191,-41.6873463901686,
-9.96398744091504));
#20782=CARTESIAN_POINT('Ctrl Pts',(-10.0613599161589,-41.5232524891608,
-10.1251796235305));
#20783=CARTESIAN_POINT('Ctrl Pts',(-10.0498207400108,-41.359735117518,-10.2867993162807));
#20784=CARTESIAN_POINT('Ctrl Pts',(-10.0339108358238,-41.1968114627984,
-10.4488603766053));
#20785=CARTESIAN_POINT('',(-12.3230698431045,-40.5485470057458,-10.470255845095));
#20786=CARTESIAN_POINT('Ctrl Pts',(-10.0339108358244,-41.1968114627986,
-10.4488603766049));
#20787=CARTESIAN_POINT('Ctrl Pts',(-10.1544541778703,-41.0660199366513,
-10.5474113291217));
#20788=CARTESIAN_POINT('Ctrl Pts',(-10.3011395093808,-40.947426038526,-10.6271346460681));
#20789=CARTESIAN_POINT('Ctrl Pts',(-10.657027210328,-40.7301679463169,-10.749241967386));
#20790=CARTESIAN_POINT('Ctrl Pts',(-10.8686869244842,-40.6384636404728,
-10.7838654923534));
#20791=CARTESIAN_POINT('Ctrl Pts',(-11.3133754716045,-40.5124596808953,
-10.7881590889241));
#20792=CARTESIAN_POINT('Ctrl Pts',(-11.5422355392933,-40.4793314784837,
-10.7577973123312));
#20793=CARTESIAN_POINT('Ctrl Pts',(-11.961438883283,-40.4770212041149,-10.6430146784548));
#20794=CARTESIAN_POINT('Ctrl Pts',(-12.1500916391208,-40.5007250057605,
-10.5663096364642));
#20795=CARTESIAN_POINT('Ctrl Pts',(-12.3230698431046,-40.5485470057456,
-10.4702558450952));
#20796=CARTESIAN_POINT('',(-12.9025055845987,-41.5424523787343,-9.34999999999999));
#20797=CARTESIAN_POINT('Ctrl Pts',(-12.3230698431044,-40.5485470057458,
-10.470255845095));
#20798=CARTESIAN_POINT('Ctrl Pts',(-12.4162342170306,-40.7336213240895,
-10.2660883599853));
#20799=CARTESIAN_POINT('Ctrl Pts',(-12.5157649758266,-40.9158835196705,
-10.062716859578));
#20800=CARTESIAN_POINT('Ctrl Pts',(-12.6216322379871,-41.0953134526064,
-9.86011238748152));
#20801=CARTESIAN_POINT('Ctrl Pts',(-12.7107622449211,-41.2463761214653,
-9.68953899553485));
#20802=CARTESIAN_POINT('Ctrl Pts',(-12.8043844401572,-41.3954311186753,
-9.51950878870709));
#20803=CARTESIAN_POINT('Ctrl Pts',(-12.9025055845986,-41.5424523787343,
-9.34999999999999));
#20804=CARTESIAN_POINT('',(-15.9945391840253,-40.4527467088538,-9.34999999999999));
#20805=CARTESIAN_POINT('Origin',(-3.46944695195361E-15,3.46944695195361E-15,
-9.34999999999999));
#20806=CARTESIAN_POINT('',(-15.7946976518867,-39.3495129251816,-10.4488603765943));
#20807=CARTESIAN_POINT('Ctrl Pts',(-15.9945391840253,-40.4527467088538,
-9.34999999999999));
#20808=CARTESIAN_POINT('Ctrl Pts',(-15.9695114269777,-40.2432871314623,
-9.55398902691376));
#20809=CARTESIAN_POINT('Ctrl Pts',(-15.9375825638984,-40.0357404760457,
-9.75864153761077));
#20810=CARTESIAN_POINT('Ctrl Pts',(-15.8987822030673,-39.8301270351085,
-9.96398744092793));
#20811=CARTESIAN_POINT('Ctrl Pts',(-15.8683247420356,-39.6687248411385,
-10.1251796235355));
#20812=CARTESIAN_POINT('Ctrl Pts',(-15.8336320697617,-39.5085140365627,
-10.2867993162778));
#20813=CARTESIAN_POINT('Ctrl Pts',(-15.7946976518867,-39.3495129251816,
-10.4488603765943));
#20814=CARTESIAN_POINT('',(-17.9682986697937,-38.3820655716606,-10.4702558451073));
#20815=CARTESIAN_POINT('Ctrl Pts',(-15.7946976518867,-39.3495129251816,
-10.4488603765943));
#20816=CARTESIAN_POINT('Ctrl Pts',(-15.8954004612252,-39.2028975625402,
-10.5474113287197));
#20817=CARTESIAN_POINT('Ctrl Pts',(-16.0237150755117,-39.0646352805812,
-10.6271346454281));
#20818=CARTESIAN_POINT('Ctrl Pts',(-16.345061301575,-38.7989404621477,-10.7492419669021));
#20819=CARTESIAN_POINT('Ctrl Pts',(-16.5415157414016,-38.6780472557653,
-10.7838654920944));
#20820=CARTESIAN_POINT('Ctrl Pts',(-16.9637457669869,-38.4900400557429,
-10.7881590891384));
#20821=CARTESIAN_POINT('Ctrl Pts',(-17.1855617344036,-38.4246788669136,
-10.7577973127721));
#20822=CARTESIAN_POINT('Ctrl Pts',(-17.600169407316,-38.3627332511513,-10.6430146790707));
#20823=CARTESIAN_POINT('Ctrl Pts',(-17.7902753536106,-38.3593476957178,
-10.5663096368568));
#20824=CARTESIAN_POINT('Ctrl Pts',(-17.9682986697938,-38.3820655716606,
-10.4702558451073));
#20825=CARTESIAN_POINT('',(-18.6832840733583,-39.2833921172065,-9.34999999999999));
#20826=CARTESIAN_POINT('Ctrl Pts',(-17.9682986697937,-38.3820655716606,
-10.4702558451073));
#20827=CARTESIAN_POINT('Ctrl Pts',(-18.0868535858997,-38.5519974267554,
-10.2660883608794));
#20828=CARTESIAN_POINT('Ctrl Pts',(-18.2113098794098,-38.718239751441,-10.062716861347));
#20829=CARTESIAN_POINT('Ctrl Pts',(-18.3416351067682,-38.8807768634145,
-9.8601123901159));
#20830=CARTESIAN_POINT('Ctrl Pts',(-18.4513563585572,-39.0176174103246,
-9.6895389972884));
#20831=CARTESIAN_POINT('Ctrl Pts',(-18.5652383532269,-39.1518314157116,
-9.51950878958326));
#20832=CARTESIAN_POINT('Ctrl Pts',(-18.6832840733583,-39.2833921172065,
-9.34999999999999));
#20833=CARTESIAN_POINT('',(-21.5887639429553,-37.7647358181592,-9.34999999999999));
#20834=CARTESIAN_POINT('Origin',(-3.46944695195361E-15,3.46944695195361E-15,
-9.34999999999999));
#20835=CARTESIAN_POINT('',(-21.2339499719768,-36.7011717789787,-10.4488603766065));
#20836=CARTESIAN_POINT('Ctrl Pts',(-21.5887639429553,-37.7647358181592,
-9.34999999999999));
#20837=CARTESIAN_POINT('Ctrl Pts',(-21.5341817265107,-37.5609700584485,
-9.55398902690961));
#20838=CARTESIAN_POINT('Ctrl Pts',(-21.4730408845247,-37.360079879714,-9.75864153760252));
#20839=CARTESIAN_POINT('Ctrl Pts',(-21.4053736118321,-37.162081154214,-9.96398744091563));
#20840=CARTESIAN_POINT('Ctrl Pts',(-21.3522562367057,-37.0066563504876,
-10.1251796235313));
#20841=CARTESIAN_POINT('Ctrl Pts',(-21.2951163110693,-36.8530135429323,
-10.2867993162817));
#20842=CARTESIAN_POINT('Ctrl Pts',(-21.2339499719768,-36.7011717789787,
-10.4488603766065));
#20843=CARTESIAN_POINT('',(-23.2477447519539,-35.434235967255,-10.4702558450962));
#20844=CARTESIAN_POINT('Ctrl Pts',(-21.2339499719768,-36.7011717789787,
-10.4488603766064));
#20845=CARTESIAN_POINT('Ctrl Pts',(-21.3127622306114,-36.5417172446673,
-10.547411329123));
#20846=CARTESIAN_POINT('Ctrl Pts',(-21.4200940133834,-36.3866011992051,
-10.6271346460693));
#20847=CARTESIAN_POINT('Ctrl Pts',(-21.7003570840256,-36.0778784343334,
-10.7492419673871));
#20848=CARTESIAN_POINT('Ctrl Pts',(-21.877607003997,-35.9302573647762,-10.7838654923545));
#20849=CARTESIAN_POINT('Ctrl Pts',(-22.2687831227019,-35.6840742095356,
-10.7881590889251));
#20850=CARTESIAN_POINT('Ctrl Pts',(-22.4790394564213,-35.5878106000643,
-10.7577973123323));
#20851=CARTESIAN_POINT('Ctrl Pts',(-22.8806112399902,-35.4674906781017,
-10.6430146784558));
#20852=CARTESIAN_POINT('Ctrl Pts',(-23.0683003663139,-35.4370846859713,
-10.5663096364652));
#20853=CARTESIAN_POINT('Ctrl Pts',(-23.2477447519539,-35.434235967255,-10.4702558450962));
#20854=CARTESIAN_POINT('',(-24.0837247765703,-36.2246352760993,-9.34999999999999));
#20855=CARTESIAN_POINT('Ctrl Pts',(-23.2477447519539,-35.434235967255,-10.4702558450962));
#20856=CARTESIAN_POINT('Ctrl Pts',(-23.3892767750413,-35.5855660380308,
-10.2660883599847));
#20857=CARTESIAN_POINT('Ctrl Pts',(-23.5361250331426,-35.7324042788876,
-10.0627168595755));
#20858=CARTESIAN_POINT('Ctrl Pts',(-23.6882551811027,-35.8747397843426,
-9.86011238747722));
#20859=CARTESIAN_POINT('Ctrl Pts',(-23.816334068434,-35.9945725289423,-9.68953899553199));
#20860=CARTESIAN_POINT('Ctrl Pts',(-23.9481575524104,-36.1112133310054,
-9.51950878870566));
#20861=CARTESIAN_POINT('Ctrl Pts',(-24.0837247765702,-36.2246352760993,
-9.34999999999999));
#20862=CARTESIAN_POINT('',(-26.7435037248304,-34.3079438107268,-9.34999999999999));
#20863=CARTESIAN_POINT('Origin',(-3.46944695195361E-15,3.46944695195361E-15,
-9.34999999999999));
#20864=CARTESIAN_POINT('',(-26.2409403042445,-33.3057006128373,-10.4488603766022));
#20865=CARTESIAN_POINT('Ctrl Pts',(-26.7435037248304,-34.3079438107268,
-9.34999999999999));
#20866=CARTESIAN_POINT('Ctrl Pts',(-26.6604781855069,-34.1140199519479,
-9.55398902691263));
#20867=CARTESIAN_POINT('Ctrl Pts',(-26.5713700158347,-33.9238757946104,
-9.75864153760855));
#20868=CARTESIAN_POINT('Ctrl Pts',(-26.4762133418097,-33.7375224676132,
-9.96398744092467));
#20869=CARTESIAN_POINT('Ctrl Pts',(-26.4015173691683,-33.59123905494,-10.1251796235359));
#20870=CARTESIAN_POINT('Ctrl Pts',(-26.3230933942782,-33.4472919689115,
-10.2867993162819));
#20871=CARTESIAN_POINT('Ctrl Pts',(-26.2409403042445,-33.3057006128373,
-10.4488603766022));
#20872=CARTESIAN_POINT('',(-28.053933791861,-31.7650675024729,-10.4702558451));
#20873=CARTESIAN_POINT('Ctrl Pts',(-26.2409403042452,-33.3057006128373,
-10.4488603766018));
#20874=CARTESIAN_POINT('Ctrl Pts',(-26.2962576214615,-33.1366529419292,
-10.547411329119));
#20875=CARTESIAN_POINT('Ctrl Pts',(-26.3804216065202,-32.9678408488439,
-10.627134646066));
#20876=CARTESIAN_POINT('Ctrl Pts',(-26.6138961728537,-32.6223748430043,
-10.7492419673853));
#20877=CARTESIAN_POINT('Ctrl Pts',(-26.7683332755725,-32.4510310493881,
-10.7838654923535));
#20878=CARTESIAN_POINT('Ctrl Pts',(-27.1204922694935,-32.1516835176302,
-10.7881590889259));
#20879=CARTESIAN_POINT('Ctrl Pts',(-27.3149087568863,-32.0264771367729,
-10.7577973123339));
#20880=CARTESIAN_POINT('Ctrl Pts',(-27.6952698084817,-31.8502322746937,
-10.6430146784589));
#20881=CARTESIAN_POINT('Ctrl Pts',(-27.8767213062725,-31.7934248240622,
-10.5663096364688));
#20882=CARTESIAN_POINT('Ctrl Pts',(-28.053933791861,-31.765067502473,-10.4702558451));
#20883=CARTESIAN_POINT('',(-28.9938902950281,-32.4284493240099,-9.34999999999999));
#20884=CARTESIAN_POINT('Ctrl Pts',(-28.053933791861,-31.7650675024729,-10.4702558451));
#20885=CARTESIAN_POINT('Ctrl Pts',(-28.2155617375712,-31.8947151443484,
-10.2660883599931));
#20886=CARTESIAN_POINT('Ctrl Pts',(-28.3818125526395,-32.0191600975308,
-10.0627168595884));
#20887=CARTESIAN_POINT('Ctrl Pts',(-28.5526506894832,-32.1383964553645,
-9.86011238749472));
#20888=CARTESIAN_POINT('Ctrl Pts',(-28.696479896089,-32.2387819492749,-9.68953899554359));
#20889=CARTESIAN_POINT('Ctrl Pts',(-28.8435613239597,-32.3354750783552,
-9.51950878871143));
#20890=CARTESIAN_POINT('Ctrl Pts',(-28.9938902950281,-32.4284493240099,
-9.34999999999999));
#20891=CARTESIAN_POINT('',(-31.3538228927626,-30.1527410032535,-9.34999999999999));
#20892=CARTESIAN_POINT('Origin',(-3.46944695195361E-15,3.46944695195361E-15,
-9.34999999999999));
#20893=CARTESIAN_POINT('',(-30.7137407645416,-29.2322214279374,-10.4488603765957));
#20894=CARTESIAN_POINT('Ctrl Pts',(-31.3538228927626,-30.1527410032535,
-9.34999999999999));
#20895=CARTESIAN_POINT('Ctrl Pts',(-31.2440441911153,-29.9726067759439,
-9.55398902691338));
#20896=CARTESIAN_POINT('Ctrl Pts',(-31.1287826791253,-29.7970794267192,
-9.75864153761002));
#20897=CARTESIAN_POINT('Ctrl Pts',(-31.0080737192424,-29.6261651145667,
-9.96398744092682));
#20898=CARTESIAN_POINT('Ctrl Pts',(-30.913319743684,-29.4920010013807,-10.1251796235352));
#20899=CARTESIAN_POINT('Ctrl Pts',(-30.8152082055132,-29.3606799844397,
-10.2867993162784));
#20900=CARTESIAN_POINT('Ctrl Pts',(-30.7137407645416,-29.2322214279374,
-10.4488603765957));
#20901=CARTESIAN_POINT('',(-32.2890256406275,-27.4492538662411,-10.4702558451039));
#20902=CARTESIAN_POINT('Ctrl Pts',(-30.7137407645416,-29.2322214279374,
-10.4488603765957));
#20903=CARTESIAN_POINT('Ctrl Pts',(-30.7444370392829,-29.0570219435195,
-10.5474113291135));
#20904=CARTESIAN_POINT('Ctrl Pts',(-30.8037198906013,-28.8779503302129,
-10.6271346460612));
#20905=CARTESIAN_POINT('Ctrl Pts',(-30.9856530837404,-28.5027737750429,
-10.7492419673821));
#20906=CARTESIAN_POINT('Ctrl Pts',(-31.114133475155,-28.3111953228912,-10.7838654923513));
#20907=CARTESIAN_POINT('Ctrl Pts',(-31.4201064027185,-27.9647772671156,
-10.7881590889256));
#20908=CARTESIAN_POINT('Ctrl Pts',(-31.5947252847521,-27.8131769557209,
-10.7577973123346));
#20909=CARTESIAN_POINT('Ctrl Pts',(-31.9461325502338,-27.5845949906688,
-10.6430146784613));
#20910=CARTESIAN_POINT('Ctrl Pts',(-32.1176525902589,-27.5025425174118,
-10.566309636472));
#20911=CARTESIAN_POINT('Ctrl Pts',(-32.2890256406275,-27.4492538662411,
-10.4702558451039));
#20912=CARTESIAN_POINT('',(-33.3138238185527,-27.9721136596152,-9.34999999999999));
#20913=CARTESIAN_POINT('Ctrl Pts',(-32.2890256406275,-27.4492538662411,
-10.4702558451039));
#20914=CARTESIAN_POINT('Ctrl Pts',(-32.4674592300822,-27.5545798271016,
-10.2660883600008));
#20915=CARTESIAN_POINT('Ctrl Pts',(-32.6497282149504,-27.6540981522332,
-10.0627168596001));
#20916=CARTESIAN_POINT('Ctrl Pts',(-32.8357965688679,-27.7478080540501,
-9.8601123875103));
#20917=CARTESIAN_POINT('Ctrl Pts',(-32.9924481468715,-27.826702738101,-9.68953899555392));
#20918=CARTESIAN_POINT('Ctrl Pts',(-33.1517933649134,-27.901479800928,-9.51950878871657));
#20919=CARTESIAN_POINT('Ctrl Pts',(-33.3138238185527,-27.9721136596152,
-9.34999999999999));
#20920=CARTESIAN_POINT('',(-35.3258686435787,-25.3837153422549,-9.34999999999999));
#20921=CARTESIAN_POINT('Origin',(-3.46944695195361E-15,3.46944695195361E-15,
-9.34999999999999));
#20922=CARTESIAN_POINT('',(-34.561298034014,-24.5636585134826,-10.4488603766016));
#20923=CARTESIAN_POINT('Ctrl Pts',(-35.3258686435787,-25.3837153422549,
-9.34999999999999));
#20924=CARTESIAN_POINT('Ctrl Pts',(-35.191571557402,-25.2210377598177,-9.5539890269114));
#20925=CARTESIAN_POINT('Ctrl Pts',(-35.0525030950958,-25.0637004493564,
-9.75864153760609));
#20926=CARTESIAN_POINT('Ctrl Pts',(-34.9086991356865,-24.9117044745671,
-9.96398744092097));
#20927=CARTESIAN_POINT('Ctrl Pts',(-34.7958160749033,-24.7923908553078,
-10.1251796235332));
#20928=CARTESIAN_POINT('Ctrl Pts',(-34.6800142414361,-24.6763692246536,
-10.2867993162803));
#20929=CARTESIAN_POINT('Ctrl Pts',(-34.561298034014,-24.5636585134826,-10.4488603766016));
#20930=CARTESIAN_POINT('',(-35.8668060412545,-22.5746525783676,-10.4702558450978));
#20931=CARTESIAN_POINT('Ctrl Pts',(-34.5612980340131,-24.5636585134822,
-10.4488603766026));
#20932=CARTESIAN_POINT('Ctrl Pts',(-34.5667483786485,-24.3858737718227,
-10.5474113291198));
#20933=CARTESIAN_POINT('Ctrl Pts',(-34.5999432683334,-24.2001880199414,
-10.6271346460667));
#20934=CARTESIAN_POINT('Ctrl Pts',(-34.7266314531219,-23.8029384281848,
-10.7492419673853));
#20935=CARTESIAN_POINT('Ctrl Pts',(-34.8265396429719,-23.5950253023176,
-10.7838654923531));
#20936=CARTESIAN_POINT('Ctrl Pts',(-35.0800977777285,-23.2085887951553,
-10.7881590889248));
#20937=CARTESIAN_POINT('Ctrl Pts',(-35.2313643175252,-23.0336806983859,
-10.7577973123324));
#20938=CARTESIAN_POINT('Ctrl Pts',(-35.546664158344,-22.7574148999972,-10.6430146784568));
#20939=CARTESIAN_POINT('Ctrl Pts',(-35.7047610872118,-22.6517877558527,
-10.5663096364666));
#20940=CARTESIAN_POINT('Ctrl Pts',(-35.8668060412538,-22.5746525783687,
-10.4702558450978));
#20941=CARTESIAN_POINT('',(-36.955583958287,-22.946346426,-9.34999999999999));
#20942=CARTESIAN_POINT('Ctrl Pts',(-35.8668060412545,-22.5746525783676,
-10.4702558450978));
#20943=CARTESIAN_POINT('Ctrl Pts',(-36.0584128811371,-22.6535127253913,
-10.2660883599907));
#20944=CARTESIAN_POINT('Ctrl Pts',(-36.2529895648988,-22.7260785163657,
-10.062716859586));
#20945=CARTESIAN_POINT('Ctrl Pts',(-36.4505003207866,-22.7923542988078,
-9.86011238749218));
#20946=CARTESIAN_POINT('Ctrl Pts',(-36.6167852957936,-22.8481521047421,
-9.68953899554191));
#20947=CARTESIAN_POINT('Ctrl Pts',(-36.7851504948685,-22.8994908559535,
-9.5195087887106));
#20948=CARTESIAN_POINT('Ctrl Pts',(-36.955583958287,-22.946346426,-9.34999999999999));
#20949=CARTESIAN_POINT('',(-38.5787815801808,-20.0979504375124,-9.34999999999999));
#20950=CARTESIAN_POINT('Origin',(-3.46944695195361E-15,3.46944695195361E-15,
-9.34999999999999));
#20951=CARTESIAN_POINT('',(-37.7052869420397,-19.3950503475036,-10.4488603765919));
#20952=CARTESIAN_POINT('Ctrl Pts',(-38.5787815801808,-20.0979504375124,
-9.34999999999999));
#20953=CARTESIAN_POINT('Ctrl Pts',(-38.4227000108615,-19.9560411464038,
-9.55398902691458));
#20954=CARTESIAN_POINT('Ctrl Pts',(-38.2626556310847,-19.8200968086245,
-9.75864153761241));
#20955=CARTESIAN_POINT('Ctrl Pts',(-38.0986841060596,-19.6901133709261,
-9.96398744093037));
#20956=CARTESIAN_POINT('Ctrl Pts',(-37.9699699336463,-19.5880791268205,
-10.1251796235364));
#20957=CARTESIAN_POINT('Ctrl Pts',(-37.8388351962726,-19.4897187482847,
-10.2867993162771));
#20958=CARTESIAN_POINT('Ctrl Pts',(-37.7052869420397,-19.3950503475036,
-10.4488603765919));
#20959=CARTESIAN_POINT('',(-38.7144417021568,-17.2404964639775,-10.4702558451079));
#20960=CARTESIAN_POINT('Ctrl Pts',(-37.70528694204,-19.3950503475025,-10.4488603765922));
#20961=CARTESIAN_POINT('Ctrl Pts',(-37.6853804032671,-19.2182995332542,
-10.5474113291108));
#20962=CARTESIAN_POINT('Ctrl Pts',(-37.6918115790876,-19.0297796692338,
-10.6271346460593));
#20963=CARTESIAN_POINT('Ctrl Pts',(-37.7606757494155,-18.6185438970059,
-10.7492419673815));
#20964=CARTESIAN_POINT('Ctrl Pts',(-37.829977895064,-18.3985286090935,-10.7838654923512));
#20965=CARTESIAN_POINT('Ctrl Pts',(-38.0259595245863,-17.9799403834372,
-10.7881590889269));
#20966=CARTESIAN_POINT('Ctrl Pts',(-38.1507943716101,-17.785285125748,-10.7577973123366));
#20967=CARTESIAN_POINT('Ctrl Pts',(-38.423568192254,-17.4669594689877,-10.6430146784646));
#20968=CARTESIAN_POINT('Ctrl Pts',(-38.5650236124062,-17.3399079180034,
-10.5663096364759));
#20969=CARTESIAN_POINT('Ctrl Pts',(-38.7144417021566,-17.2404964639768,
-10.4702558451083));
#20970=CARTESIAN_POINT('',(-39.845034979713,-17.4534577509859,-9.34999999999999));
#20971=CARTESIAN_POINT('Ctrl Pts',(-38.7144417021568,-17.2404964639775,
-10.4702558451079));
#20972=CARTESIAN_POINT('Ctrl Pts',(-38.9153212297535,-17.2912854319784,
-10.2660883600021));
#20973=CARTESIAN_POINT('Ctrl Pts',(-39.1182445922376,-17.3354214585475,
-10.0627168595987));
#20974=CARTESIAN_POINT('Ctrl Pts',(-39.323177000677,-17.3729139378015,-9.8601123875063));
#20975=CARTESIAN_POINT('Ctrl Pts',(-39.4957102901352,-17.4044789831982,
-9.68953899555125));
#20976=CARTESIAN_POINT('Ctrl Pts',(-39.6696680403279,-17.4313343138675,
-9.51950878871524));
#20977=CARTESIAN_POINT('Ctrl Pts',(-39.845034979713,-17.4534577509859,-9.34999999999999));
#20978=CARTESIAN_POINT('',(-41.0463417758467,-14.4030492195362,-9.34999999999999));
#20979=CARTESIAN_POINT('Origin',(-3.46944695195361E-15,3.46944695195361E-15,
-9.34999999999999));
#20980=CARTESIAN_POINT('',(-40.0817049410149,-13.8316148870952,-10.4488603765949));
#20981=CARTESIAN_POINT('Ctrl Pts',(-41.0463417758468,-14.4030492195362,
-9.34999999999999));
#20982=CARTESIAN_POINT('Ctrl Pts',(-40.871653094042,-14.2847970836902,-9.55398902691117));
#20983=CARTESIAN_POINT('Ctrl Pts',(-40.6938908388447,-14.1730131532785,
-9.75864153760559));
#20984=CARTESIAN_POINT('Ctrl Pts',(-40.5130897356062,-14.0676883406206,
-9.96398744092016));
#20985=CARTESIAN_POINT('Ctrl Pts',(-40.371164700926,-13.9850105946256,-10.1251796235305));
#20986=CARTESIAN_POINT('Ctrl Pts',(-40.2273665847308,-13.9063138018573,
-10.2867993162756));
#20987=CARTESIAN_POINT('Ctrl Pts',(-40.081704941015,-13.8316148870952,-10.4488603765949));
#20988=CARTESIAN_POINT('',(-40.7739629732767,-11.5553735590169,-10.4702558451026));
#20989=CARTESIAN_POINT('Ctrl Pts',(-40.0817049410152,-13.831614887095,-10.4488603765947));
#20990=CARTESIAN_POINT('Ctrl Pts',(-40.0368467585607,-13.6594961371281,
-10.5474113291124));
#20991=CARTESIAN_POINT('Ctrl Pts',(-40.0163833003259,-13.4719798817537,
-10.6271346460599));
#20992=CARTESIAN_POINT('Ctrl Pts',(-40.0260215802783,-13.0551295034711,
-10.7492419673806));
#20993=CARTESIAN_POINT('Ctrl Pts',(-40.0633068898933,-12.8274909303035,
-10.7838654923497));
#20994=CARTESIAN_POINT('Ctrl Pts',(-40.1977223933732,-12.3852722353198,
-10.7881590889239));
#20995=CARTESIAN_POINT('Ctrl Pts',(-40.2935842701349,-12.1748324364192,
-10.7577973123328));
#20996=CARTESIAN_POINT('Ctrl Pts',(-40.5182791822329,-11.8209271136879,
-10.6430146784594));
#20997=CARTESIAN_POINT('Ctrl Pts',(-40.6402134692392,-11.6750375590585,
-10.5663096364703));
#20998=CARTESIAN_POINT('Ctrl Pts',(-40.7739629732768,-11.5553735590173,
-10.4702558451023));
#20999=CARTESIAN_POINT('',(-41.9233559925594,-11.6052670077487,-9.34999999999999));
#21000=CARTESIAN_POINT('Ctrl Pts',(-40.7739629732767,-11.5553735590169,
-10.4702558451026));
#21001=CARTESIAN_POINT('Ctrl Pts',(-40.9800258606916,-11.5770574310741,
-10.2660883599987));
#21002=CARTESIAN_POINT('Ctrl Pts',(-41.1871649674178,-11.5918652110192,
-10.0627168595972));
#21003=CARTESIAN_POINT('Ctrl Pts',(-41.3953471955466,-11.5998111483317,
-9.86011238750657));
#21004=CARTESIAN_POINT('Ctrl Pts',(-41.5706165192209,-11.6065008598948,
-9.68953899555145));
#21005=CARTESIAN_POINT('Ctrl Pts',(-41.7466255423837,-11.6083260729364,
-9.51950878871534));
#21006=CARTESIAN_POINT('Ctrl Pts',(-41.9233559925594,-11.6052670077487,
-9.34999999999999));
#21007=CARTESIAN_POINT('',(-42.6783168208273,-8.4149434544203,-9.34999999999999));
#21008=CARTESIAN_POINT('Origin',(-3.46944695195361E-15,3.46944695195361E-15,
-9.34999999999999));
#21009=CARTESIAN_POINT('',(-41.6421750134749,-7.98660763468004,-10.4488603765984));
#21010=CARTESIAN_POINT('Ctrl Pts',(-42.6783168208273,-8.41494345442029,
-9.34999999999999));
#21011=CARTESIAN_POINT('Ctrl Pts',(-42.4885771843355,-8.32275574631041,
-9.5539890269104));
#21012=CARTESIAN_POINT('Ctrl Pts',(-42.2967157806069,-8.23740782173034,
-9.75864153760406));
#21013=CARTESIAN_POINT('Ctrl Pts',(-42.102765688227,-8.15888574356603,-9.96398744091788));
#21014=CARTESIAN_POINT('Ctrl Pts',(-41.9505189757091,-8.09724757616996,
-10.1251796235301));
#21015=CARTESIAN_POINT('Ctrl Pts',(-41.7969847956598,-8.0398164089298,-10.2867993162772));
#21016=CARTESIAN_POINT('Ctrl Pts',(-41.6421750134748,-7.98660763468004,
-10.4488603765984));
#21017=CARTESIAN_POINT('',(-42.0034439406495,-5.63501657134773,-10.4702558451016));
#21018=CARTESIAN_POINT('Ctrl Pts',(-41.6421750134749,-7.98660763468003,
-10.4488603765984));
#21019=CARTESIAN_POINT('Ctrl Pts',(-41.5732783705724,-7.82262479039399,
-10.5474113291159));
#21020=CARTESIAN_POINT('Ctrl Pts',(-41.5263368552795,-7.63992943387202,
-10.6271346460633));
#21021=CARTESIAN_POINT('Ctrl Pts',(-41.4765530372705,-7.22595032113848,
-10.7492419673834));
#21022=CARTESIAN_POINT('Ctrl Pts',(-41.4810624894699,-6.99532252761,-10.783865492352));
#21023=CARTESIAN_POINT('Ctrl Pts',(-41.5511755548784,-6.53847566067517,
-10.7881590889253));
#21024=CARTESIAN_POINT('Ctrl Pts',(-41.6161129900097,-6.31653526801044,
-10.7577973123337));
#21025=CARTESIAN_POINT('Ctrl Pts',(-41.788154853118,-5.93425477109959,-10.6430146784595));
#21026=CARTESIAN_POINT('Ctrl Pts',(-41.8880857765248,-5.77249710344573,
-10.5663096364699));
#21027=CARTESIAN_POINT('Ctrl Pts',(-42.0034439406495,-5.63501657134772,
-10.4702558451016));
#21028=CARTESIAN_POINT('',(-43.1482383743694,-5.52082649506381,-9.34999999999999));
#21029=CARTESIAN_POINT('Ctrl Pts',(-42.0034439406495,-5.63501657134772,
-10.4702558451016));
#21030=CARTESIAN_POINT('Ctrl Pts',(-42.2104953417357,-5.62715392635674,
-10.2660883599956));
#21031=CARTESIAN_POINT('Ctrl Pts',(-42.4176334378355,-5.61233201597962,
-10.0627168595919));
#21032=CARTESIAN_POINT('Ctrl Pts',(-42.6248274958417,-5.59056965498014,
-9.86011238749915));
#21033=CARTESIAN_POINT('Ctrl Pts',(-42.799264875735,-5.57224784947292,-9.68953899554653));
#21034=CARTESIAN_POINT('Ctrl Pts',(-42.9737421357223,-5.54900578881237,
-9.5195087887129));
#21035=CARTESIAN_POINT('Ctrl Pts',(-43.1482383743694,-5.5208264950638,-9.34999999999999));
#21036=CARTESIAN_POINT('',(-43.4414844094373,-2.25553370726721,-9.34999999999999));
#21037=CARTESIAN_POINT('Origin',(-3.46944695195361E-15,3.46944695195361E-15,
-9.34999999999999));
#21038=CARTESIAN_POINT('',(-42.3549304887756,-1.97901608230199,-10.4488603766005));
#21039=CARTESIAN_POINT('Ctrl Pts',(-43.4414844094373,-2.25553370726721,
-9.34999999999999));
#21040=CARTESIAN_POINT('Ctrl Pts',(-43.2405563700911,-2.19128710278271,
-9.55398902691193));
#21041=CARTESIAN_POINT('Ctrl Pts',(-43.038501562726,-2.13411262165511,-9.75864153760715));
#21042=CARTESIAN_POINT('Ctrl Pts',(-42.8353507457773,-2.08399176105654,
-9.96398744092254));
#21043=CARTESIAN_POINT('Ctrl Pts',(-42.6758816594476,-2.04464794759932,
-10.1251796235339));
#21044=CARTESIAN_POINT('Ctrl Pts',(-42.5157369286964,-2.00965153883589,
-10.2867993162801));
#21045=CARTESIAN_POINT('Ctrl Pts',(-42.3549304887756,-1.97901608230198,
-10.4488603766005));
#21046=CARTESIAN_POINT('',(-42.1895973099932,-1.50796436832281E-9,-10.6604026900068));
#21047=CARTESIAN_POINT('Ctrl Pts',(-42.3549304887756,-1.979016082302,-10.4488603766005));
#21048=CARTESIAN_POINT('Ctrl Pts',(-42.2777622816011,-1.8504408109375,-10.531945562799));
#21049=CARTESIAN_POINT('Ctrl Pts',(-42.2140750286935,-1.7063561510611,-10.6017307219897));
#21050=CARTESIAN_POINT('Ctrl Pts',(-42.1138804087173,-1.38542074402617,
-10.7136554733245));
#21051=CARTESIAN_POINT('Ctrl Pts',(-42.0800627876842,-1.20890695927121,
-10.7529641474029));
#21052=CARTESIAN_POINT('Ctrl Pts',(-42.046111502818,-0.795598132330741,
-10.7969991342822));
#21053=CARTESIAN_POINT('Ctrl Pts',(-42.0583624188812,-0.559734595950683,
-10.7885243575832));
#21054=CARTESIAN_POINT('Ctrl Pts',(-42.1231209760754,-0.218323779409197,
-10.7264706453147));
#21055=CARTESIAN_POINT('Ctrl Pts',(-42.1526851017604,-0.106675909104108,
-10.697314898232));
#21056=CARTESIAN_POINT('Ctrl Pts',(-42.1895973099932,-3.01592865264988E-9,
-10.6604026900068));
#21057=CARTESIAN_POINT('',(-41.5,-1.612837264507E-15,-11.35));
#21058=CARTESIAN_POINT('',(-43.5,-1.85776662433645E-15,-9.34999999999999));
#21059=CARTESIAN_POINT('Origin',(-3.46944695195361E-15,1.73472347597681E-15,
-11.35));
#21060=CARTESIAN_POINT('',(-42.3778559173175,0.400053103664136,-10.4702558451013));
#21061=CARTESIAN_POINT('Ctrl Pts',(-42.1895973099932,-3.0159285715309E-9,
-10.6604026900068));
#21062=CARTESIAN_POINT('Ctrl Pts',(-42.1974267713527,0.0226270606221863,
-10.652573228649));
#21063=CARTESIAN_POINT('Ctrl Pts',(-42.2055869083974,0.0450304331853256,
-10.6443948820145));
#21064=CARTESIAN_POINT('Ctrl Pts',(-42.2597977418648,0.186602611542281,
-10.589958769094));
#21065=CARTESIAN_POINT('Ctrl Pts',(-42.3147058279888,0.298272918359021,
-10.5343638976612));
#21066=CARTESIAN_POINT('Ctrl Pts',(-42.3778559173175,0.400053103664132,
-10.4702558451013));
#21067=CARTESIAN_POINT('',(-43.4947470521204,0.676002124309098,-9.34999999999999));
#21068=CARTESIAN_POINT('Ctrl Pts',(-42.3778559173175,0.400053103664149,
-10.4702558451013));
#21069=CARTESIAN_POINT('Ctrl Pts',(-42.5816808626342,0.437302204925704,
-10.2660883599949));
#21070=CARTESIAN_POINT('Ctrl Pts',(-42.7846012138064,0.481452074273063,
-10.0627168595909));
#21071=CARTESIAN_POINT('Ctrl Pts',(-42.9865892281655,0.532479714672422,
-9.86011238749772));
#21072=CARTESIAN_POINT('Ctrl Pts',(-43.1566436222613,0.57544005812541,-9.68953899554559));
#21073=CARTESIAN_POINT('Ctrl Pts',(-43.3260372652128,0.62327625115777,-9.51950878871243));
#21074=CARTESIAN_POINT('Ctrl Pts',(-43.4947470521204,0.676002124309097,
-9.34999999999999));
#21075=CARTESIAN_POINT('',(-43.3203086503669,3.94979220174326,-9.34999999999999));
#21076=CARTESIAN_POINT('Origin',(-3.46944695195361E-15,3.46944695195361E-15,
-9.34999999999999));
#21077=CARTESIAN_POINT('',(-42.2054617208597,4.06886253049829,-10.4488603766002));
#21078=CARTESIAN_POINT('Ctrl Pts',(-43.3203086503669,3.94979220174326,-9.34999999999999));
#21079=CARTESIAN_POINT('Ctrl Pts',(-43.1122825236194,3.98478982700619,-9.55398902691261));
#21080=CARTESIAN_POINT('Ctrl Pts',(-42.9041475658186,4.01262695712239,-9.75864153760851));
#21081=CARTESIAN_POINT('Ctrl Pts',(-42.6959315890961,4.03332628396938,-9.9639874409246));
#21082=CARTESIAN_POINT('Ctrl Pts',(-42.5324864596814,4.04957481690408,-10.1251796235352));
#21083=CARTESIAN_POINT('Ctrl Pts',(-42.3689912631271,4.0614240412298,-10.2867993162806));
#21084=CARTESIAN_POINT('Ctrl Pts',(-42.2054617208597,4.0688625304983,-10.4488603766002));
#21085=CARTESIAN_POINT('',(-41.8895769551539,6.42697885114126,-10.4702558451001));
#21086=CARTESIAN_POINT('Ctrl Pts',(-42.2054617208597,4.06886253049829,-10.4488603766002));
#21087=CARTESIAN_POINT('Ctrl Pts',(-42.0931565705377,4.20679248947244,-10.5474113287251));
#21088=CARTESIAN_POINT('Ctrl Pts',(-41.9966452868457,4.36886244650457,-10.6271346454328));
#21089=CARTESIAN_POINT('Ctrl Pts',(-41.8322466693347,4.75204677304844,-10.7492419669048));
#21090=CARTESIAN_POINT('Ctrl Pts',(-41.7715980988893,4.97460297983664,-10.7838654920958));
#21091=CARTESIAN_POINT('Ctrl Pts',(-41.7101624561644,5.43269747180171,-10.7881590891372));
#21092=CARTESIAN_POINT('Ctrl Pts',(-41.7099416343854,5.66394270882025,-10.7577973127697));
#21093=CARTESIAN_POINT('Ctrl Pts',(-41.7673137310929,6.07920795449955,-10.6430146790662));
#21094=CARTESIAN_POINT('Ctrl Pts',(-41.8176243487641,6.26256709539985,-10.5663096368512));
#21095=CARTESIAN_POINT('Ctrl Pts',(-41.8895769551532,6.42697885114131,-10.4702558451007));
#21096=CARTESIAN_POINT('',(-42.9558281083827,6.85906928985893,-9.34999999999999));
#21097=CARTESIAN_POINT('Ctrl Pts',(-41.8895769551539,6.42697885114127,-10.4702558451001));
#21098=CARTESIAN_POINT('Ctrl Pts',(-42.0860261557539,6.49285612410681,-10.2660883608697));
#21099=CARTESIAN_POINT('Ctrl Pts',(-42.2805978879953,6.56543518806218,-10.0627168613349));
#21100=CARTESIAN_POINT('Ctrl Pts',(-42.4732679644127,6.64468933185857,-9.86011239010124));
#21101=CARTESIAN_POINT('Ctrl Pts',(-42.6354775564803,6.71141366484236,-9.68953899727869));
#21102=CARTESIAN_POINT('Ctrl Pts',(-42.7963392171419,6.7828701836438,-9.51950878957843));
#21103=CARTESIAN_POINT('Ctrl Pts',(-42.9558281083827,6.85906928985893,-9.34999999999999));
#21104=CARTESIAN_POINT('',(-42.3172563326291,10.0747117317853,-9.34999999999999));
#21105=CARTESIAN_POINT('Origin',(-3.46944695195361E-15,3.46944695195361E-15,
-9.34999999999999));
#21106=CARTESIAN_POINT('',(-41.1968114628076,10.0339108358061,-10.4488603766004));
#21107=CARTESIAN_POINT('Ctrl Pts',(-42.3172563326291,10.0747117317853,-9.34999999999999));
#21108=CARTESIAN_POINT('Ctrl Pts',(-42.1063669305215,10.0797479271007,-9.55398902691476));
#21109=CARTESIAN_POINT('Ctrl Pts',(-41.8963888498126,10.0776810225116,-9.75864153761282));
#21110=CARTESIAN_POINT('Ctrl Pts',(-41.6873463901558,10.0685374370037,-9.96398744093108));
#21111=CARTESIAN_POINT('Ctrl Pts',(-41.5232524891554,10.0613599161423,-10.1251796235396));
#21112=CARTESIAN_POINT('Ctrl Pts',(-41.35973511752,10.0498207399935,-10.2867993162829));
#21113=CARTESIAN_POINT('Ctrl Pts',(-41.1968114628076,10.0339108358061,-10.4488603766004));
#21114=CARTESIAN_POINT('',(-40.5485470057466,12.3230698430839,-10.4702558451002));
#21115=CARTESIAN_POINT('Ctrl Pts',(-41.1968114628078,10.0339108358065,-10.4488603766002));
#21116=CARTESIAN_POINT('Ctrl Pts',(-41.0660199366602,10.1544541778516,-10.5474113291175));
#21117=CARTESIAN_POINT('Ctrl Pts',(-40.9474260385346,10.3011395093612,-10.6271346460645));
#21118=CARTESIAN_POINT('Ctrl Pts',(-40.7301679463243,10.6570272103071,-10.7492419673841));
#21119=CARTESIAN_POINT('Ctrl Pts',(-40.6384636404793,10.8686869244629,-10.7838654923525));
#21120=CARTESIAN_POINT('Ctrl Pts',(-40.5124596809,11.3133754715828,-10.7881590889254));
#21121=CARTESIAN_POINT('Ctrl Pts',(-40.4793314784874,11.5422355392716,-10.7577973123336));
#21122=CARTESIAN_POINT('Ctrl Pts',(-40.4770212041169,11.9614388832617,-10.6430146784589));
#21123=CARTESIAN_POINT('Ctrl Pts',(-40.5007250057618,12.1500916390997,-10.5663096364691));
#21124=CARTESIAN_POINT('Ctrl Pts',(-40.5485470057463,12.3230698430838,-10.4702558451005));
#21125=CARTESIAN_POINT('',(-41.5424523787372,12.9025055845893,-9.34999999999999));
#21126=CARTESIAN_POINT('Ctrl Pts',(-40.5485470057466,12.3230698430839,-10.4702558451002));
#21127=CARTESIAN_POINT('Ctrl Pts',(-40.7336213240878,12.4162342170104,-10.2660883599929));
#21128=CARTESIAN_POINT('Ctrl Pts',(-40.9158835196662,12.5157649758065,-10.0627168595879));
#21129=CARTESIAN_POINT('Ctrl Pts',(-41.0953134525995,12.621632237967,-9.86011238749391));
#21130=CARTESIAN_POINT('Ctrl Pts',(-41.2463761214618,12.7107622449043,-9.68953899554305));
#21131=CARTESIAN_POINT('Ctrl Pts',(-41.3954311186751,12.8043844401441,-9.51950878871116));
#21132=CARTESIAN_POINT('Ctrl Pts',(-41.5424523787372,12.9025055845893,-9.34999999999999));
#21133=CARTESIAN_POINT('',(-40.4527467088508,15.9945391840328,-9.34999999999999));
#21134=CARTESIAN_POINT('Origin',(-3.46944695195361E-15,3.46944695195361E-15,
-9.34999999999999));
#21135=CARTESIAN_POINT('',(-39.3495129251727,15.7946976518991,-10.4488603765979));
#21136=CARTESIAN_POINT('Ctrl Pts',(-40.4527467088508,15.9945391840329,-9.34999999999999));
#21137=CARTESIAN_POINT('Ctrl Pts',(-40.2432871314579,15.9695114269864,-9.55398902691462));
#21138=CARTESIAN_POINT('Ctrl Pts',(-40.03574047604,15.937582563908,-9.75864153761254));
#21139=CARTESIAN_POINT('Ctrl Pts',(-39.8301270351014,15.8987822030778,-9.96398744093064));
#21140=CARTESIAN_POINT('Ctrl Pts',(-39.6687248411308,15.8683247420467,-10.1251796235385));
#21141=CARTESIAN_POINT('Ctrl Pts',(-39.5085140365544,15.8336320697735,-10.2867993162811));
#21142=CARTESIAN_POINT('Ctrl Pts',(-39.3495129251727,15.7946976518991,-10.4488603765979));
#21143=CARTESIAN_POINT('',(-38.382065571658,17.9682986698097,-10.4702558451029));
#21144=CARTESIAN_POINT('Ctrl Pts',(-39.3495129251723,15.7946976518996,-10.4488603765981));
#21145=CARTESIAN_POINT('Ctrl Pts',(-39.2028975619468,15.8954004616402,-10.5474113291157));
#21146=CARTESIAN_POINT('Ctrl Pts',(-39.0646352794747,16.0237150765457,-10.6271346460632));
#21147=CARTESIAN_POINT('Ctrl Pts',(-38.7989404607791,16.3450613035865,-10.7492419673833));
#21148=CARTESIAN_POINT('Ctrl Pts',(-38.6780472545519,16.5415157435844,-10.783865492352));
#21149=CARTESIAN_POINT('Ctrl Pts',(-38.4900400549329,16.9637457693522,-10.7881590889255));
#21150=CARTESIAN_POINT('Ctrl Pts',(-38.4246788663334,17.1855617367719,-10.757797312334));
#21151=CARTESIAN_POINT('Ctrl Pts',(-38.3627332511209,17.6001694088377,-10.64301467846));
#21152=CARTESIAN_POINT('Ctrl Pts',(-38.3593476958059,17.7902753543337,-10.5663096364705));
#21153=CARTESIAN_POINT('Ctrl Pts',(-38.382065571659,17.9682986698092,-10.4702558451022));
#21154=CARTESIAN_POINT('',(-39.2833921172033,18.6832840733651,-9.34999999999999));
#21155=CARTESIAN_POINT('Ctrl Pts',(-38.382065571658,17.9682986698097,-10.4702558451029));
#21156=CARTESIAN_POINT('Ctrl Pts',(-38.5519974274827,18.0868535864236,-10.2660883599985));
#21157=CARTESIAN_POINT('Ctrl Pts',(-38.7182397528666,18.2113098804923,-10.0627168595965));
#21158=CARTESIAN_POINT('Ctrl Pts',(-38.880776865504,18.3416351084573,-9.86011238750546));
#21159=CARTESIAN_POINT('Ctrl Pts',(-39.017617411692,18.45135635973,-9.68953899555072));
#21160=CARTESIAN_POINT('Ctrl Pts',(-39.1518314163817,18.5652383538395,-9.51950878871498));
#21161=CARTESIAN_POINT('Ctrl Pts',(-39.2833921172033,18.6832840733651,-9.34999999999999));
#21162=CARTESIAN_POINT('',(-37.7647358181634,21.588763942948,-9.34999999999999));
#21163=CARTESIAN_POINT('Origin',(-3.46944695195361E-15,3.46944695195361E-15,
-9.34999999999999));
#21164=CARTESIAN_POINT('',(-36.7011717789913,21.2339499719654,-10.4488603766012));
#21165=CARTESIAN_POINT('Ctrl Pts',(-37.7647358181634,21.588763942948,-9.34999999999999));
#21166=CARTESIAN_POINT('Ctrl Pts',(-37.5609700584519,21.5341817265017,-9.55398902691111));
#21167=CARTESIAN_POINT('Ctrl Pts',(-37.3600798797167,21.473040884514,-9.7586415376055));
#21168=CARTESIAN_POINT('Ctrl Pts',(-37.162081154216,21.4053736118198,-9.96398744092007));
#21169=CARTESIAN_POINT('Ctrl Pts',(-37.0066563504932,21.3522562366935,-10.1251796235325));
#21170=CARTESIAN_POINT('Ctrl Pts',(-36.8530135429414,21.2951163110575,-10.2867993162797));
#21171=CARTESIAN_POINT('Ctrl Pts',(-36.7011717789913,21.2339499719654,-10.4488603766012));
#21172=CARTESIAN_POINT('',(-35.4342359672603,23.2477447519392,-10.4702558450998));
#21173=CARTESIAN_POINT('Ctrl Pts',(-36.7011717789913,21.2339499719654,-10.4488603766012));
#21174=CARTESIAN_POINT('Ctrl Pts',(-36.5417172446798,21.3127622305992,-10.5474113291184));
#21175=CARTESIAN_POINT('Ctrl Pts',(-36.3866011992174,21.4200940133705,-10.6271346460654));
#21176=CARTESIAN_POINT('Ctrl Pts',(-36.0778784343449,21.7003570840114,-10.7492419673846));
#21177=CARTESIAN_POINT('Ctrl Pts',(-35.9302573647871,21.8776070039822,-10.7838654923527));
#21178=CARTESIAN_POINT('Ctrl Pts',(-35.6840742095452,22.2687831226866,-10.7881590889251));
#21179=CARTESIAN_POINT('Ctrl Pts',(-35.5878106000732,22.4790394564059,-10.757797312333));
#21180=CARTESIAN_POINT('Ctrl Pts',(-35.4674906781093,22.8806112399746,-10.6430146784579));
#21181=CARTESIAN_POINT('Ctrl Pts',(-35.4370846859782,23.0683003662984,-10.566309636468));
#21182=CARTESIAN_POINT('Ctrl Pts',(-35.4342359672613,23.2477447519385,-10.4702558450994));
#21183=CARTESIAN_POINT('',(-36.224635276104,24.0837247765632,-9.34999999999999));
#21184=CARTESIAN_POINT('Ctrl Pts',(-35.4342359672603,23.2477447519392,-10.4702558450998));
#21185=CARTESIAN_POINT('Ctrl Pts',(-35.5855660380337,23.3892767750254,-10.2660883599909));
#21186=CARTESIAN_POINT('Ctrl Pts',(-35.7324042788881,23.5361250331255,-10.0627168595844));
#21187=CARTESIAN_POINT('Ctrl Pts',(-35.8747397843408,23.6882551810844,-9.86011238748882));
#21188=CARTESIAN_POINT('Ctrl Pts',(-35.9945725289429,23.8163340684192,-9.68953899553967));
#21189=CARTESIAN_POINT('Ctrl Pts',(-36.1112133310081,23.9481575523993,-9.51950878870948));
#21190=CARTESIAN_POINT('Ctrl Pts',(-36.224635276104,24.0837247765632,-9.34999999999999));
#21191=CARTESIAN_POINT('',(-34.3079438107289,26.7435037248277,-9.34999999999999));
#21192=CARTESIAN_POINT('Origin',(-3.46944695195361E-15,3.46944695195361E-15,
-9.34999999999999));
#21193=CARTESIAN_POINT('',(-33.3057006128448,26.2409403042404,-10.4488603765989));
#21194=CARTESIAN_POINT('Ctrl Pts',(-34.3079438107289,26.7435037248277,-9.34999999999999));
#21195=CARTESIAN_POINT('Ctrl Pts',(-34.1140199519504,26.6604781855035,-9.55398902691272));
#21196=CARTESIAN_POINT('Ctrl Pts',(-33.9238757946133,26.5713700158308,-9.75864153760872));
#21197=CARTESIAN_POINT('Ctrl Pts',(-33.7375224676165,26.4762133418051,-9.96398744092491));
#21198=CARTESIAN_POINT('Ctrl Pts',(-33.5912390549448,26.4015173691638,-10.125179623535));
#21199=CARTESIAN_POINT('Ctrl Pts',(-33.4472919689175,26.3230933942739,-10.2867993162798));
#21200=CARTESIAN_POINT('Ctrl Pts',(-33.3057006128448,26.2409403042404,-10.4488603765989));
#21201=CARTESIAN_POINT('',(-31.7650675024763,28.0539337918545,-10.4702558451018));
#21202=CARTESIAN_POINT('Ctrl Pts',(-33.3057006128448,26.2409403042404,-10.4488603765989));
#21203=CARTESIAN_POINT('Ctrl Pts',(-33.1366529419366,26.2962576214563,-10.5474113291164));
#21204=CARTESIAN_POINT('Ctrl Pts',(-32.9678408488513,26.3804216065147,-10.6271346460638));
#21205=CARTESIAN_POINT('Ctrl Pts',(-32.6223748430112,26.6138961728476,-10.7492419673837));
#21206=CARTESIAN_POINT('Ctrl Pts',(-32.4510310493948,26.7683332755662,-10.7838654923524));
#21207=CARTESIAN_POINT('Ctrl Pts',(-32.1516835176362,27.1204922694869,-10.7881590889256));
#21208=CARTESIAN_POINT('Ctrl Pts',(-32.0264771367785,27.3149087568795,-10.757797312334));
#21209=CARTESIAN_POINT('Ctrl Pts',(-31.8502322746985,27.6952698084749,-10.6430146784597));
#21210=CARTESIAN_POINT('Ctrl Pts',(-31.7934248240667,27.8767213062657,-10.5663096364699));
#21211=CARTESIAN_POINT('Ctrl Pts',(-31.7650675024771,28.0539337918543,-10.4702558451013));
#21212=CARTESIAN_POINT('',(-32.4284493240122,28.9938902950256,-9.34999999999999));
#21213=CARTESIAN_POINT('Ctrl Pts',(-31.7650675024763,28.0539337918545,-10.4702558451018));
#21214=CARTESIAN_POINT('Ctrl Pts',(-31.8947151443539,28.2155617375679,-10.2660883599912));
#21215=CARTESIAN_POINT('Ctrl Pts',(-32.019160097538,28.3818125526397,-10.0627168595829));
#21216=CARTESIAN_POINT('Ctrl Pts',(-32.1383964553732,28.552650689487,-9.86011238748564));
#21217=CARTESIAN_POINT('Ctrl Pts',(-32.2387819492814,28.6964798960908,-9.68953899553755));
#21218=CARTESIAN_POINT('Ctrl Pts',(-32.3354750783595,28.8435613239594,-9.51950878870842));
#21219=CARTESIAN_POINT('Ctrl Pts',(-32.4284493240122,28.9938902950256,-9.34999999999999));
#21220=CARTESIAN_POINT('',(-30.1527410032581,31.353822892758,-9.34999999999999));
#21221=CARTESIAN_POINT('Origin',(-3.46944695195361E-15,3.46944695195361E-15,
-9.34999999999999));
#21222=CARTESIAN_POINT('',(-29.2322214279503,30.7137407645344,-10.448860376592));
#21223=CARTESIAN_POINT('Ctrl Pts',(-30.1527410032581,31.353822892758,-9.34999999999999));
#21224=CARTESIAN_POINT('Ctrl Pts',(-29.9726067759491,31.2440441911095,-9.55398902691394));
#21225=CARTESIAN_POINT('Ctrl Pts',(-29.797079426725,31.1287826791183,-9.75864153761113));
#21226=CARTESIAN_POINT('Ctrl Pts',(-29.6261651145731,31.0080737192341,-9.96398744092845));
#21227=CARTESIAN_POINT('Ctrl Pts',(-29.4920010013893,30.9133197436759,-10.1251796235351));
#21228=CARTESIAN_POINT('Ctrl Pts',(-29.3606799844505,30.8152082055055,-10.2867993162765));
#21229=CARTESIAN_POINT('Ctrl Pts',(-29.2322214279503,30.7137407645344,-10.448860376592));
#21230=CARTESIAN_POINT('',(-27.4492538662502,32.2890256406138,-10.4702558451084));
#21231=CARTESIAN_POINT('Ctrl Pts',(-29.2322214279499,30.7137407645349,-10.4488603765919));
#21232=CARTESIAN_POINT('Ctrl Pts',(-29.0570219435323,30.7444370392754,-10.5474113291101));
#21233=CARTESIAN_POINT('Ctrl Pts',(-28.877950330226,30.803719890593,-10.6271346460583));
#21234=CARTESIAN_POINT('Ctrl Pts',(-28.502773775056,30.9856530837304,-10.7492419673805));
#21235=CARTESIAN_POINT('Ctrl Pts',(-28.311195322904,31.1141334751444,-10.7838654923505));
#21236=CARTESIAN_POINT('Ctrl Pts',(-27.9647772671275,31.4201064027068,-10.7881590889265));
#21237=CARTESIAN_POINT('Ctrl Pts',(-27.8131769557322,31.59472528474,-10.7577973123362));
#21238=CARTESIAN_POINT('Ctrl Pts',(-27.5845949906789,31.9461325502209,-10.6430146784644));
#21239=CARTESIAN_POINT('Ctrl Pts',(-27.5025425174213,32.1176525902456,-10.566309636476));
#21240=CARTESIAN_POINT('Ctrl Pts',(-27.4492538662497,32.2890256406138,-10.4702558451087));
#21241=CARTESIAN_POINT('',(-27.9721136596209,33.313823818548,-9.34999999999999));
#21242=CARTESIAN_POINT('Ctrl Pts',(-27.4492538662502,32.2890256406138,-10.4702558451084));
#21243=CARTESIAN_POINT('Ctrl Pts',(-27.5545798271122,32.4674592300734,-10.2660883600007));
#21244=CARTESIAN_POINT('Ctrl Pts',(-27.654098152245,32.6497282149467,-10.0627168595954));
#21245=CARTESIAN_POINT('Ctrl Pts',(-27.7478080540628,32.8357965688694,-9.86011238750101));
#21246=CARTESIAN_POINT('Ctrl Pts',(-27.8267027381112,32.9924481468711,-9.68953899554773));
#21247=CARTESIAN_POINT('Ctrl Pts',(-27.9014798009359,33.1517933649108,-9.51950878871348));
#21248=CARTESIAN_POINT('Ctrl Pts',(-27.9721136596209,33.313823818548,-9.34999999999999));
#21249=CARTESIAN_POINT('',(-25.3837153422505,35.3258686435819,-9.34999999999999));
#21250=CARTESIAN_POINT('Origin',(-3.46944695195361E-15,3.46944695195361E-15,
-9.34999999999999));
#21251=CARTESIAN_POINT('',(-24.5636585134689,34.561298034017,-10.4488603766072));
#21252=CARTESIAN_POINT('Ctrl Pts',(-25.3837153422505,35.3258686435819,-9.34999999999999));
#21253=CARTESIAN_POINT('Ctrl Pts',(-25.2210377598102,35.1915715574042,-9.55398902691391));
#21254=CARTESIAN_POINT('Ctrl Pts',(-25.0637004493459,35.052503095097,-9.75864153761116));
#21255=CARTESIAN_POINT('Ctrl Pts',(-24.9117044745538,34.9086991356865,-9.96398744092865));
#21256=CARTESIAN_POINT('Ctrl Pts',(-24.7923908552944,34.7958160749043,-10.1251796235402));
#21257=CARTESIAN_POINT('Ctrl Pts',(-24.67636922464,34.6800142414381,-10.2867993162866));
#21258=CARTESIAN_POINT('Ctrl Pts',(-24.5636585134689,34.561298034017,-10.4488603766072));
#21259=CARTESIAN_POINT('',(-22.5746525783567,35.8668060412644,-10.4702558450952));
#21260=CARTESIAN_POINT('Ctrl Pts',(-24.563658513468,34.5612980340179,-10.4488603766069));
#21261=CARTESIAN_POINT('Ctrl Pts',(-24.3858737718084,34.5667483786537,-10.5474113291238));
#21262=CARTESIAN_POINT('Ctrl Pts',(-24.200188019927,34.5999432683392,-10.6271346460702));
#21263=CARTESIAN_POINT('Ctrl Pts',(-23.8029384281704,34.7266314531289,-10.7492419673877));
#21264=CARTESIAN_POINT('Ctrl Pts',(-23.5950253023033,34.8265396429796,-10.7838654923547));
#21265=CARTESIAN_POINT('Ctrl Pts',(-23.2085887951417,35.0800977777375,-10.7881590889249));
#21266=CARTESIAN_POINT('Ctrl Pts',(-23.0336806983727,35.2313643175347,-10.7577973123318));
#21267=CARTESIAN_POINT('Ctrl Pts',(-22.757414899985,35.5466641583542,-10.6430146784548));
#21268=CARTESIAN_POINT('Ctrl Pts',(-22.6517877558409,35.7047610872222,-10.5663096364641));
#21269=CARTESIAN_POINT('Ctrl Pts',(-22.5746525783574,35.8668060412645,-10.4702558450948));
#21270=CARTESIAN_POINT('',(-22.9463464259947,36.9555839582903,-9.34999999999999));
#21271=CARTESIAN_POINT('Ctrl Pts',(-22.5746525783567,35.8668060412644,-10.4702558450952));
#21272=CARTESIAN_POINT('Ctrl Pts',(-22.6535127253813,36.0584128811461,-10.2660883599885));
#21273=CARTESIAN_POINT('Ctrl Pts',(-22.7260785163567,36.2529895649068,-10.062716859584));
#21274=CARTESIAN_POINT('Ctrl Pts',(-22.7923542987999,36.4505003207935,-9.86011238749044));
#21275=CARTESIAN_POINT('Ctrl Pts',(-22.848152104735,36.6167852957994,-9.68953899554077));
#21276=CARTESIAN_POINT('Ctrl Pts',(-22.8994908559473,36.785150494873,-9.51950878871004));
#21277=CARTESIAN_POINT('Ctrl Pts',(-22.9463464259947,36.9555839582903,-9.34999999999999));
#21278=CARTESIAN_POINT('',(-20.0979504374858,38.5787815801947,-9.34999999999999));
#21279=CARTESIAN_POINT('Origin',(-3.46944695195361E-15,3.46944695195361E-15,
-9.34999999999999));
#21280=CARTESIAN_POINT('',(-19.3950503474463,37.7052869420536,-10.4488603766057));
#21281=CARTESIAN_POINT('Ctrl Pts',(-20.0979504374858,38.5787815801947,-9.35));
#21282=CARTESIAN_POINT('Ctrl Pts',(-19.9560411463757,38.4227000108812,-9.55398902691007));
#21283=CARTESIAN_POINT('Ctrl Pts',(-19.8200968085948,38.2626556311101,-9.75864153760344));
#21284=CARTESIAN_POINT('Ctrl Pts',(-19.6901133708948,38.0986841060908,-9.96398744091703));
#21285=CARTESIAN_POINT('Ctrl Pts',(-19.5880791267801,37.9699699336721,-10.125179623532));
#21286=CARTESIAN_POINT('Ctrl Pts',(-19.4897187482356,37.8388351962927,-10.2867993162817));
#21287=CARTESIAN_POINT('Ctrl Pts',(-19.3950503474463,37.7052869420536,-10.4488603766058));
#21288=CARTESIAN_POINT('',(-17.2404964639284,38.7144417021942,-10.4702558450937));
#21289=CARTESIAN_POINT('Ctrl Pts',(-19.3950503474456,37.7052869420535,-10.4488603766062));
#21290=CARTESIAN_POINT('Ctrl Pts',(-19.2182995331962,37.6853804032832,-10.5474113291228));
#21291=CARTESIAN_POINT('Ctrl Pts',(-19.0297796691752,37.6918115791063,-10.6271346460691));
#21292=CARTESIAN_POINT('Ctrl Pts',(-18.6185438969465,37.7606757494393,-10.7492419673865));
#21293=CARTESIAN_POINT('Ctrl Pts',(-18.3985286090339,37.8299778950903,-10.7838654923536));
#21294=CARTESIAN_POINT('Ctrl Pts',(-17.9799403833786,38.0259595246174,-10.7881590889238));
#21295=CARTESIAN_POINT('Ctrl Pts',(-17.7852851256906,38.1507943716434,-10.7577973123307));
#21296=CARTESIAN_POINT('Ctrl Pts',(-17.4669594689343,38.4235681922903,-10.6430146784537));
#21297=CARTESIAN_POINT('Ctrl Pts',(-17.3399079179525,38.5650236124433,-10.566309636463));
#21298=CARTESIAN_POINT('Ctrl Pts',(-17.2404964639285,38.7144417021941,-10.4702558450937));
#21299=CARTESIAN_POINT('',(-17.4534577509583,39.8450349797251,-9.34999999999999));
#21300=CARTESIAN_POINT('Ctrl Pts',(-17.2404964639284,38.7144417021942,-10.4702558450937));
#21301=CARTESIAN_POINT('Ctrl Pts',(-17.2912854319336,38.9153212297907,-10.2660883599863));
#21302=CARTESIAN_POINT('Ctrl Pts',(-17.335421458507,39.1182445922746,-10.0627168595812));
#21303=CARTESIAN_POINT('Ctrl Pts',(-17.3729139377655,39.3231770007139,-9.86011238748706));
#21304=CARTESIAN_POINT('Ctrl Pts',(-17.4044789831645,39.4957102901639,-9.68953899553853));
#21305=CARTESIAN_POINT('Ctrl Pts',(-17.4313343138366,39.6696680403483,-9.51950878870892));
#21306=CARTESIAN_POINT('Ctrl Pts',(-17.4534577509583,39.8450349797251,-9.34999999999999));
#21307=CARTESIAN_POINT('',(-14.4030492195196,41.0463417758526,-9.34999999999999));
#21308=CARTESIAN_POINT('Origin',(-3.46944695195361E-15,3.46944695195361E-15,
-9.34999999999999));
#21309=CARTESIAN_POINT('',(-13.8316148870599,40.0817049410166,-10.4488603766049));
#21310=CARTESIAN_POINT('Ctrl Pts',(-14.4030492195196,41.0463417758526,-9.34999999999999));
#21311=CARTESIAN_POINT('Ctrl Pts',(-14.2847970836707,40.8716530940489,-9.55398902691104));
#21312=CARTESIAN_POINT('Ctrl Pts',(-14.1730131532563,40.6938908388526,-9.7586415376054));
#21313=CARTESIAN_POINT('Ctrl Pts',(-14.0676883405958,40.5130897356151,-9.96398744091997));
#21314=CARTESIAN_POINT('Ctrl Pts',(-13.9850105945971,40.3711647009326,-10.1251796235337));
#21315=CARTESIAN_POINT('Ctrl Pts',(-13.9063138018252,40.227366584735,-10.2867993162822));
#21316=CARTESIAN_POINT('Ctrl Pts',(-13.8316148870599,40.0817049410166,-10.4488603766049));
#21317=CARTESIAN_POINT('',(-11.5553735589841,40.7739629732932,-10.4702558450957));
#21318=CARTESIAN_POINT('Ctrl Pts',(-13.8316148870598,40.0817049410166,-10.4488603766049));
#21319=CARTESIAN_POINT('Ctrl Pts',(-13.6594961370917,40.0368467585633,-10.5474113291217));
#21320=CARTESIAN_POINT('Ctrl Pts',(-13.4719798817163,40.0163833003297,-10.6271346460682));
#21321=CARTESIAN_POINT('Ctrl Pts',(-13.0551295034324,40.0260215802851,-10.7492419673861));
#21322=CARTESIAN_POINT('Ctrl Pts',(-12.8274909302648,40.0633068899016,-10.7838654923536));
#21323=CARTESIAN_POINT('Ctrl Pts',(-12.3852722352818,40.1977223933844,-10.7881590889245));
#21324=CARTESIAN_POINT('Ctrl Pts',(-12.174832436382,40.2935842701473,-10.7577973123317));
#21325=CARTESIAN_POINT('Ctrl Pts',(-11.8209271136526,40.5182791822475,-10.6430146784553));
#21326=CARTESIAN_POINT('Ctrl Pts',(-11.6750375590242,40.6402134692549,-10.5663096364647));
#21327=CARTESIAN_POINT('Ctrl Pts',(-11.5553735589844,40.7739629732933,-10.4702558450954));
#21328=CARTESIAN_POINT('',(-11.6052670077299,41.9233559925646,-9.34999999999999));
#21329=CARTESIAN_POINT('Ctrl Pts',(-11.5553735589841,40.7739629732932,-10.4702558450957));
#21330=CARTESIAN_POINT('Ctrl Pts',(-11.5770574310437,40.9800258607092,-10.2660883599901));
#21331=CARTESIAN_POINT('Ctrl Pts',(-11.5918652109912,41.1871649674364,-10.0627168595868));
#21332=CARTESIAN_POINT('Ctrl Pts',(-11.5998111483063,41.3953471955663,-9.86011238749444));
#21333=CARTESIAN_POINT('Ctrl Pts',(-11.6065008598711,41.5706165192358,-9.68953899554343));
#21334=CARTESIAN_POINT('Ctrl Pts',(-11.608326072915,41.7466255423937,-9.51950878871137));
#21335=CARTESIAN_POINT('Ctrl Pts',(-11.6052670077299,41.9233559925646,-9.34999999999999));
#21336=CARTESIAN_POINT('',(-8.41494345442185,42.678316820827,-9.34999999999999));
#21337=CARTESIAN_POINT('Origin',(-3.46944695195361E-15,3.46944695195361E-15,
-9.34999999999999));
#21338=CARTESIAN_POINT('',(-7.98660763468405,41.6421750134759,-10.4488603765967));
#21339=CARTESIAN_POINT('Ctrl Pts',(-8.41494345442186,42.678316820827,-9.34999999999999));
#21340=CARTESIAN_POINT('Ctrl Pts',(-8.32275574631089,42.4885771843321,-9.55398902691367));
#21341=CARTESIAN_POINT('Ctrl Pts',(-8.23740782172991,42.2967157806002,-9.75864153761063));
#21342=CARTESIAN_POINT('Ctrl Pts',(-8.1588857435649,42.1027656882172,-9.96398744092778));
#21343=CARTESIAN_POINT('Ctrl Pts',(-8.09724757617075,41.9505189757028,-10.1251796235362));
#21344=CARTESIAN_POINT('Ctrl Pts',(-8.03981640893231,41.7969847956571,-10.2867993162793));
#21345=CARTESIAN_POINT('Ctrl Pts',(-7.98660763468405,41.6421750134759,-10.4488603765967));
#21346=CARTESIAN_POINT('',(-5.63501657135133,42.0034439406494,-10.4702558451012));
#21347=CARTESIAN_POINT('Ctrl Pts',(-7.98660763468398,41.6421750134755,-10.448860376597));
#21348=CARTESIAN_POINT('Ctrl Pts',(-7.82262479039767,41.5732783705729,-10.5474113291148));
#21349=CARTESIAN_POINT('Ctrl Pts',(-7.6399294338754,41.5263368552799,-10.6271346460624));
#21350=CARTESIAN_POINT('Ctrl Pts',(-7.22595032114179,41.4765530372707,-10.7492419673826));
#21351=CARTESIAN_POINT('Ctrl Pts',(-6.99532252761349,41.4810624894699,-10.7838654923514));
#21352=CARTESIAN_POINT('Ctrl Pts',(-6.53847566067895,41.551175554878,-10.7881590889251));
#21353=CARTESIAN_POINT('Ctrl Pts',(-6.31653526801434,41.6161129900091,-10.7577973123337));
#21354=CARTESIAN_POINT('Ctrl Pts',(-5.93425477110337,41.7881548531172,-10.6430146784598));
#21355=CARTESIAN_POINT('Ctrl Pts',(-5.77249710344944,41.888085776524,-10.5663096364702));
#21356=CARTESIAN_POINT('Ctrl Pts',(-5.63501657135134,42.0034439406487,-10.4702558451019));
#21357=CARTESIAN_POINT('',(-5.52082649506595,43.1482383743691,-9.34999999999999));
#21358=CARTESIAN_POINT('Ctrl Pts',(-5.63501657135133,42.0034439406494,-10.4702558451012));
#21359=CARTESIAN_POINT('Ctrl Pts',(-5.62715392636005,42.210495341738,-10.2660883599929));
#21360=CARTESIAN_POINT('Ctrl Pts',(-5.61233201598245,42.4176334378401,-10.062716859587));
#21361=CARTESIAN_POINT('Ctrl Pts',(-5.5905696549823,42.6248274958485,-9.86011238749209));
#21362=CARTESIAN_POINT('Ctrl Pts',(-5.57224784947496,42.7992648757395,-9.68953899554182));
#21363=CARTESIAN_POINT('Ctrl Pts',(-5.54900578881441,42.9737421357244,-9.51950878871054));
#21364=CARTESIAN_POINT('Ctrl Pts',(-5.52082649506595,43.1482383743691,-9.34999999999999));
#21365=CARTESIAN_POINT('',(-2.25553370726646,43.4414844094374,-9.34999999999999));
#21366=CARTESIAN_POINT('Origin',(-3.46944695195361E-15,3.46944695195361E-15,
-9.34999999999999));
#21367=CARTESIAN_POINT('',(-1.9790160823007,42.3549304887752,-10.4488603766009));
#21368=CARTESIAN_POINT('Ctrl Pts',(-2.25553370726647,43.4414844094374,-9.34999999999999));
#21369=CARTESIAN_POINT('Ctrl Pts',(-2.19128710278198,43.2405563700915,-9.55398902691156));
#21370=CARTESIAN_POINT('Ctrl Pts',(-2.13411262165439,43.0385015627268,-9.7586415376064));
#21371=CARTESIAN_POINT('Ctrl Pts',(-2.08399176105579,42.8353507457784,-9.96398744092142));
#21372=CARTESIAN_POINT('Ctrl Pts',(-2.04464794759835,42.6758816594482,-10.1251796235333));
#21373=CARTESIAN_POINT('Ctrl Pts',(-2.00965153883474,42.5157369286965,-10.28679931628));
#21374=CARTESIAN_POINT('Ctrl Pts',(-1.97901608230068,42.3549304887752,-10.4488603766009));
#21375=CARTESIAN_POINT('',(0.400053103665631,42.3778559173192,-10.4702558450996));
#21376=CARTESIAN_POINT('Ctrl Pts',(-1.97901608230066,42.3549304887752,-10.4488603766009));
#21377=CARTESIAN_POINT('Ctrl Pts',(-1.82650736151777,42.2633979223932,-10.5474113291179));
#21378=CARTESIAN_POINT('Ctrl Pts',(-1.65235205445744,42.1909339439257,-10.6271346460647));
#21379=CARTESIAN_POINT('Ctrl Pts',(-1.24967162819109,42.0827414829252,-10.7492419673841));
#21380=CARTESIAN_POINT('Ctrl Pts',(-1.02074953110196,42.0543832782663,-10.7838654923523));
#21381=CARTESIAN_POINT('Ctrl Pts',(-0.558574576988578,42.0587666057809,
-10.7881590889248));
#21382=CARTESIAN_POINT('Ctrl Pts',(-0.32965165693059,42.0914576603666,-10.7577973123328));
#21383=CARTESIAN_POINT('Ctrl Pts',(0.0732218856487259,42.2073441982801,
-10.6430146784578));
#21384=CARTESIAN_POINT('Ctrl Pts',(0.247554746683578,42.2832374526635,-10.5663096364682));
#21385=CARTESIAN_POINT('Ctrl Pts',(0.400053103665668,42.3778559173188,-10.4702558451));
#21386=CARTESIAN_POINT('',(0.67600212430957,43.4947470521204,-9.34999999999999));
#21387=CARTESIAN_POINT('Ctrl Pts',(0.400053103665649,42.3778559173192,-10.4702558450996));
#21388=CARTESIAN_POINT('Ctrl Pts',(0.437302204927781,42.5816808626396,-10.2660883599896));
#21389=CARTESIAN_POINT('Ctrl Pts',(0.48145207427596,42.7846012138153,-10.062716859582));
#21390=CARTESIAN_POINT('Ctrl Pts',(0.532479714676378,42.9865892281779,-9.86011238748525));
#21391=CARTESIAN_POINT('Ctrl Pts',(0.575440058128448,43.1566436222696,-9.68953899553729));
#21392=CARTESIAN_POINT('Ctrl Pts',(0.623276251159649,43.3260372652169,-9.51950878870829));
#21393=CARTESIAN_POINT('Ctrl Pts',(0.67600212430957,43.4947470521203,-9.34999999999999));
#21394=CARTESIAN_POINT('',(3.94979220174152,43.320308650367,-9.34999999999999));
#21395=CARTESIAN_POINT('Origin',(-3.46944695195361E-15,3.46944695195361E-15,
-9.34999999999999));
#21396=CARTESIAN_POINT('',(4.06886253049489,42.2054617208602,-10.4488603766));
#21397=CARTESIAN_POINT('Ctrl Pts',(3.94979220174152,43.320308650367,-9.34999999999999));
#21398=CARTESIAN_POINT('Ctrl Pts',(3.98478982700399,43.1122825236203,-9.55398902691186));
#21399=CARTESIAN_POINT('Ctrl Pts',(4.0126269571198,42.9041475658203,-9.758641537607));
#21400=CARTESIAN_POINT('Ctrl Pts',(4.03332628396646,42.6959315890987,-9.96398744092232));
#21401=CARTESIAN_POINT('Ctrl Pts',(4.04957481690103,42.5324864596833,-10.1251796235336));
#21402=CARTESIAN_POINT('Ctrl Pts',(4.06142404122659,42.3689912631283,-10.2867993162797));
#21403=CARTESIAN_POINT('Ctrl Pts',(4.06886253049491,42.2054617208602,-10.4488603766));
#21404=CARTESIAN_POINT('',(6.42697885113784,41.8895769551534,-10.4702558451011));
#21405=CARTESIAN_POINT('Ctrl Pts',(4.0688625304949,42.2054617208602,-10.4488603766));
#21406=CARTESIAN_POINT('Ctrl Pts',(4.20679249001818,42.0931565700911,-10.5474113291173));
#21407=CARTESIAN_POINT('Ctrl Pts',(4.36886244778761,41.996645286081,-10.6271346460644));
#21408=CARTESIAN_POINT('Ctrl Pts',(4.75204677534186,41.8322466685925,-10.7492419673842));
#21409=CARTESIAN_POINT('Ctrl Pts',(4.97460298225102,41.7715980983432,-10.7838654923527));
#21410=CARTESIAN_POINT('Ctrl Pts',(5.43269747427877,41.7101624560549,-10.7881590889257));
#21411=CARTESIAN_POINT('Ctrl Pts',(5.6639427112363,41.7099416344962,-10.757797312334));
#21412=CARTESIAN_POINT('Ctrl Pts',(6.07920795594927,41.7673137314911,-10.6430146784595));
#21413=CARTESIAN_POINT('Ctrl Pts',(6.26256709604998,41.81762434905,-10.56630963647));
#21414=CARTESIAN_POINT('Ctrl Pts',(6.42697885113787,41.8895769551527,-10.4702558451018));
#21415=CARTESIAN_POINT('',(6.8590692898575,42.9558281083829,-9.34999999999999));
#21416=CARTESIAN_POINT('Ctrl Pts',(6.42697885113785,41.8895769551534,-10.4702558451011));
#21417=CARTESIAN_POINT('Ctrl Pts',(6.49285612438642,42.0860261565966,-10.2660883599944));
#21418=CARTESIAN_POINT('Ctrl Pts',(6.5654351886824,42.2805978896651,-10.0627168595899));
#21419=CARTESIAN_POINT('Ctrl Pts',(6.64468933287527,42.4732679668901,-9.86011238749645));
#21420=CARTESIAN_POINT('Ctrl Pts',(6.71141366556903,42.6354775581211,-9.68953899554473));
#21421=CARTESIAN_POINT('Ctrl Pts',(6.78287018403159,42.7963392179574,-9.519508788712));
#21422=CARTESIAN_POINT('Ctrl Pts',(6.85906928985751,42.9558281083829,-9.34999999999999));
#21423=CARTESIAN_POINT('',(10.0747117317978,42.317256332626,-9.34999999999999));
#21424=CARTESIAN_POINT('Origin',(-3.46944695195361E-15,3.46944695195361E-15,
-9.34999999999999));
#21425=CARTESIAN_POINT('',(10.0339108358286,41.1968114627961,-10.4488603766063));
#21426=CARTESIAN_POINT('Ctrl Pts',(10.0747117317978,42.317256332626,-9.34999999999999));
#21427=CARTESIAN_POINT('Ctrl Pts',(10.0797479271153,42.1063669305229,-9.55398902690997));
#21428=CARTESIAN_POINT('Ctrl Pts',(10.0776810225284,41.8963888498183,-9.75864153760328));
#21429=CARTESIAN_POINT('Ctrl Pts',(10.0685374370231,41.6873463901658,-9.96398744091679));
#21430=CARTESIAN_POINT('Ctrl Pts',(10.0613599161632,41.5232524891582,-10.125179623532));
#21431=CARTESIAN_POINT('Ctrl Pts',(10.0498207400154,41.3597351175156,-10.286799316282));
#21432=CARTESIAN_POINT('Ctrl Pts',(10.0339108358287,41.1968114627961,-10.4488603766063));
#21433=CARTESIAN_POINT('',(12.3230698431103,40.5485470057438,-10.4702558450952));
#21434=CARTESIAN_POINT('Ctrl Pts',(10.0339108358291,41.1968114627954,-10.4488603766069));
#21435=CARTESIAN_POINT('Ctrl Pts',(10.1544541778752,41.0660199366484,-10.5474113291233));
#21436=CARTESIAN_POINT('Ctrl Pts',(10.3011395093857,40.9474260385234,-10.6271346460695));
#21437=CARTESIAN_POINT('Ctrl Pts',(10.6570272103333,40.7301679463145,-10.749241967387));
#21438=CARTESIAN_POINT('Ctrl Pts',(10.86868692449,40.6384636404703,-10.7838654923542));
#21439=CARTESIAN_POINT('Ctrl Pts',(11.3133754716112,40.5124596808929,-10.7881590889245));
#21440=CARTESIAN_POINT('Ctrl Pts',(11.5422355393004,40.4793314784814,-10.7577973123314));
#21441=CARTESIAN_POINT('Ctrl Pts',(11.9614388832899,40.4770212041131,-10.6430146784546));
#21442=CARTESIAN_POINT('Ctrl Pts',(12.1500916391271,40.5007250057588,-10.5663096364641));
#21443=CARTESIAN_POINT('Ctrl Pts',(12.3230698431103,40.5485470057438,-10.4702558450952));
#21444=CARTESIAN_POINT('',(12.9025055846018,41.5424523787333,-9.34999999999999));
#21445=CARTESIAN_POINT('Ctrl Pts',(12.3230698431103,40.5485470057438,-10.4702558450952));
#21446=CARTESIAN_POINT('Ctrl Pts',(12.4162342170355,40.7336213240864,-10.2660883599869));
#21447=CARTESIAN_POINT('Ctrl Pts',(12.5157649758303,40.9158835196663,-10.0627168595808));
#21448=CARTESIAN_POINT('Ctrl Pts',(12.6216322379894,41.0953134526012,-9.86011238748572));
#21449=CARTESIAN_POINT('Ctrl Pts',(12.7107622449237,41.2463761214615,-9.68953899553764));
#21450=CARTESIAN_POINT('Ctrl Pts',(12.8043844401601,41.3954311186729,-9.51950878870848));
#21451=CARTESIAN_POINT('Ctrl Pts',(12.9025055846018,41.5424523787333,-9.35));
#21452=CARTESIAN_POINT('',(15.9945391840345,40.4527467088502,-9.34999999999999));
#21453=CARTESIAN_POINT('Origin',(-3.46944695195361E-15,3.46944695195361E-15,
-9.34999999999999));
#21454=CARTESIAN_POINT('',(15.7946976519012,39.3495129251702,-10.4488603765994));
#21455=CARTESIAN_POINT('Ctrl Pts',(15.9945391840345,40.4527467088502,-9.34999999999999));
#21456=CARTESIAN_POINT('Ctrl Pts',(15.9695114269884,40.2432871314594,-9.55398902691247));
#21457=CARTESIAN_POINT('Ctrl Pts',(15.9375825639107,40.0357404760436,-9.75864153760821));
#21458=CARTESIAN_POINT('Ctrl Pts',(15.8987822030811,39.830127035107,-9.96398744092413));
#21459=CARTESIAN_POINT('Ctrl Pts',(15.8683247420498,39.6687248411337,-10.1251796235346));
#21460=CARTESIAN_POINT('Ctrl Pts',(15.8336320697762,39.5085140365546,-10.2867993162799));
#21461=CARTESIAN_POINT('Ctrl Pts',(15.7946976519012,39.3495129251702,-10.4488603765994));
#21462=CARTESIAN_POINT('',(17.9682986698117,38.3820655716568,-10.4702558451031));
#21463=CARTESIAN_POINT('Ctrl Pts',(15.7946976519015,39.3495129251703,-10.4488603765992));
#21464=CARTESIAN_POINT('Ctrl Pts',(15.895400461241,39.202897562529,-10.5474113287242));
#21465=CARTESIAN_POINT('Ctrl Pts',(16.0237150755281,39.0646352805704,-10.6271346454319));
#21466=CARTESIAN_POINT('Ctrl Pts',(16.3450613015928,38.7989404621379,-10.7492419669043));
#21467=CARTESIAN_POINT('Ctrl Pts',(16.5415157414198,38.6780472557562,-10.7838654920957));
#21468=CARTESIAN_POINT('Ctrl Pts',(16.9637457670055,38.4900400557353,-10.7881590891377));
#21469=CARTESIAN_POINT('Ctrl Pts',(17.1855617344222,38.424678866907,-10.7577973127706));
#21470=CARTESIAN_POINT('Ctrl Pts',(17.6001694073344,38.3627332511461,-10.6430146790677));
#21471=CARTESIAN_POINT('Ctrl Pts',(17.7902753536288,38.3593476957134,-10.5663096368531));
#21472=CARTESIAN_POINT('Ctrl Pts',(17.9682986698117,38.3820655716568,-10.4702558451031));
#21473=CARTESIAN_POINT('',(18.6832840733669,39.2833921172024,-9.34999999999999));
#21474=CARTESIAN_POINT('Ctrl Pts',(17.9682986698117,38.3820655716568,-10.4702558451031));
#21475=CARTESIAN_POINT('Ctrl Pts',(18.0868535859201,38.5519974267569,-10.2660883608694));
#21476=CARTESIAN_POINT('Ctrl Pts',(18.2113098794329,38.7182397514476,-10.0627168613312));
#21477=CARTESIAN_POINT('Ctrl Pts',(18.3416351067942,38.8807768634261,-9.86011239009425));
#21478=CARTESIAN_POINT('Ctrl Pts',(18.4513563585778,39.0176174103307,-9.68953899727404));
#21479=CARTESIAN_POINT('Ctrl Pts',(18.5652383532418,39.1518314157124,-9.5195087895761));
#21480=CARTESIAN_POINT('Ctrl Pts',(18.6832840733669,39.2833921172024,-9.34999999999999));
#21481=CARTESIAN_POINT('',(21.588763942955,37.7647358181594,-9.34999999999999));
#21482=CARTESIAN_POINT('Origin',(-3.46944695195361E-15,3.46944695195361E-15,
-9.34999999999999));
#21483=CARTESIAN_POINT('',(21.2339499719776,36.7011717789779,-10.4488603766068));
#21484=CARTESIAN_POINT('Ctrl Pts',(21.588763942955,37.7647358181594,-9.34999999999999));
#21485=CARTESIAN_POINT('Ctrl Pts',(21.5341817265093,37.5609700584441,-9.55398902691411));
#21486=CARTESIAN_POINT('Ctrl Pts',(21.473040884522,37.360079879705,-9.75864153761156));
#21487=CARTESIAN_POINT('Ctrl Pts',(21.4053736118279,37.1620811542006,-9.96398744092925));
#21488=CARTESIAN_POINT('Ctrl Pts',(21.3522562367029,37.0066563504785,-10.1251796235405));
#21489=CARTESIAN_POINT('Ctrl Pts',(21.2951163110683,36.8530135429274,-10.2867993162865));
#21490=CARTESIAN_POINT('Ctrl Pts',(21.2339499719776,36.7011717789779,-10.4488603766068));
#21491=CARTESIAN_POINT('',(23.2477447519555,35.4342359672547,-10.4702558450955));
#21492=CARTESIAN_POINT('Ctrl Pts',(21.2339499719779,36.7011717789774,-10.448860376607));
#21493=CARTESIAN_POINT('Ctrl Pts',(21.3127622302985,36.541717245301,-10.5474113287312));
#21494=CARTESIAN_POINT('Ctrl Pts',(21.4200940125319,36.3866012004346,-10.627134645438));
#21495=CARTESIAN_POINT('Ctrl Pts',(21.7003570822457,36.0778784359621,-10.749241966908));
#21496=CARTESIAN_POINT('Ctrl Pts',(21.8776070020259,35.9302573662764,-10.7838654920979));
#21497=CARTESIAN_POINT('Ctrl Pts',(22.2687831204933,35.6840742106644,-10.788159089137));
#21498=CARTESIAN_POINT('Ctrl Pts',(22.4790394541771,35.5878106009671,-10.7577973127683));
#21499=CARTESIAN_POINT('Ctrl Pts',(22.8806112385055,35.4674906783418,-10.6430146790628));
#21500=CARTESIAN_POINT('Ctrl Pts',(23.0683003656025,35.4370846859814,-10.5663096368471));
#21501=CARTESIAN_POINT('Ctrl Pts',(23.2477447519554,35.434235967254,-10.4702558450962));
#21502=CARTESIAN_POINT('',(24.0837247765699,36.2246352760995,-9.34999999999999));
#21503=CARTESIAN_POINT('Ctrl Pts',(23.2477447519555,35.4342359672547,-10.4702558450955));
#21504=CARTESIAN_POINT('Ctrl Pts',(23.3892767744334,35.5855660373794,-10.2660883608628));
#21505=CARTESIAN_POINT('Ctrl Pts',(23.5361250318794,35.7324042776236,-10.0627168613255));
#21506=CARTESIAN_POINT('Ctrl Pts',(23.6882551791415,35.8747397825072,-9.86011239008947));
#21507=CARTESIAN_POINT('Ctrl Pts',(23.816334067086,35.9945725277493,-9.68953899727089));
#21508=CARTESIAN_POINT('Ctrl Pts',(23.9481575517153,36.1112133304241,-9.51950878957455));
#21509=CARTESIAN_POINT('Ctrl Pts',(24.0837247765699,36.2246352760995,-9.34999999999999));
#21510=CARTESIAN_POINT('',(26.7435037248324,34.3079438107253,-9.34999999999999));
#21511=CARTESIAN_POINT('Origin',(-3.46944695195361E-15,3.46944695195361E-15,
-9.34999999999999));
#21512=CARTESIAN_POINT('',(26.2409403042474,33.3057006128359,-10.4488603766015));
#21513=CARTESIAN_POINT('Ctrl Pts',(26.7435037248324,34.3079438107253,-9.34999999999999));
#21514=CARTESIAN_POINT('Ctrl Pts',(26.6604781855094,34.1140199519472,-9.55398902691165));
#21515=CARTESIAN_POINT('Ctrl Pts',(26.5713700158378,33.9238757946105,-9.75864153760659));
#21516=CARTESIAN_POINT('Ctrl Pts',(26.4762133418134,33.7375224676141,-9.96398744092173));
#21517=CARTESIAN_POINT('Ctrl Pts',(26.4015173691717,33.5912390549401,-10.1251796235337));
#21518=CARTESIAN_POINT('Ctrl Pts',(26.3230933942815,33.4472919689108,-10.2867993162805));
#21519=CARTESIAN_POINT('Ctrl Pts',(26.2409403042474,33.3057006128359,-10.4488603766015));
#21520=CARTESIAN_POINT('',(28.0539337918648,31.7650675024716,-10.4702558450985));
#21521=CARTESIAN_POINT('Ctrl Pts',(26.2409403042471,33.3057006128354,-10.4488603766021));
#21522=CARTESIAN_POINT('Ctrl Pts',(26.2962576214637,33.1366529419271,-10.5474113291192));
#21523=CARTESIAN_POINT('Ctrl Pts',(26.3804216065228,32.9678408488418,-10.627134646066));
#21524=CARTESIAN_POINT('Ctrl Pts',(26.613896172857,32.6223748430022,-10.7492419673848));
#21525=CARTESIAN_POINT('Ctrl Pts',(26.768333275576,32.4510310493861,-10.7838654923528));
#21526=CARTESIAN_POINT('Ctrl Pts',(27.1204922694974,32.1516835176286,-10.7881590889247));
#21527=CARTESIAN_POINT('Ctrl Pts',(27.3149087568902,32.0264771367714,-10.7577973123325));
#21528=CARTESIAN_POINT('Ctrl Pts',(27.6952698084857,31.8502322746928,-10.6430146784569));
#21529=CARTESIAN_POINT('Ctrl Pts',(27.8767213062763,31.7934248240617,-10.5663096364667));
#21530=CARTESIAN_POINT('Ctrl Pts',(28.0539337918646,31.7650675024728,-10.4702558450978));
#21531=CARTESIAN_POINT('',(28.9938902950294,32.4284493240087,-9.34999999999999));
#21532=CARTESIAN_POINT('Ctrl Pts',(28.0539337918648,31.7650675024716,-10.4702558450985));
#21533=CARTESIAN_POINT('Ctrl Pts',(28.2155617375765,31.8947151443487,-10.2660883599894));
#21534=CARTESIAN_POINT('Ctrl Pts',(28.3818125526464,32.0191600975325,-10.0627168595826));
#21535=CARTESIAN_POINT('Ctrl Pts',(28.5526506894918,32.1383964553675,-9.86011238748669));
#21536=CARTESIAN_POINT('Ctrl Pts',(28.6964798960953,32.2387819492764,-9.68953899553826));
#21537=CARTESIAN_POINT('Ctrl Pts',(28.8435613239636,32.3354750783553,-9.51950878870877));
#21538=CARTESIAN_POINT('Ctrl Pts',(28.9938902950295,32.4284493240087,-9.34999999999999));
#21539=CARTESIAN_POINT('',(31.3538228927686,30.1527410032472,-9.34999999999999));
#21540=CARTESIAN_POINT('Origin',(-3.46944695195361E-15,3.46944695195361E-15,
-9.34999999999999));
#21541=CARTESIAN_POINT('',(30.7137407645493,29.2322214279229,-10.4488603766001));
#21542=CARTESIAN_POINT('Ctrl Pts',(31.3538228927686,30.1527410032472,-9.34999999999999));
#21543=CARTESIAN_POINT('Ctrl Pts',(31.2440441911241,29.9726067759396,-9.55398902690996));
#21544=CARTESIAN_POINT('Ctrl Pts',(31.128782679137,29.7970794267169,-9.7586415376032));
#21545=CARTESIAN_POINT('Ctrl Pts',(31.0080737192571,29.6261651145661,-9.9639874409166));
#21546=CARTESIAN_POINT('Ctrl Pts',(30.9133197436966,29.4920010013753,-10.1251796235298));
#21547=CARTESIAN_POINT('Ctrl Pts',(30.8152082055235,29.3606799844297,-10.2867993162779));
#21548=CARTESIAN_POINT('Ctrl Pts',(30.7137407645493,29.2322214279229,-10.4488603766001));
#21549=CARTESIAN_POINT('',(32.2890256406395,27.4492538662297,-10.4702558451021));
#21550=CARTESIAN_POINT('Ctrl Pts',(30.713740764549,29.232221427923,-10.4488603766003));
#21551=CARTESIAN_POINT('Ctrl Pts',(30.7444370392911,29.0570219435048,-10.5474113291176));
#21552=CARTESIAN_POINT('Ctrl Pts',(30.8037198906101,28.8779503301982,-10.6271346460648));
#21553=CARTESIAN_POINT('Ctrl Pts',(30.9856530837504,28.5027737750284,-10.7492419673845));
#21554=CARTESIAN_POINT('Ctrl Pts',(31.1141334751655,28.311195322877,-10.783865492353));
#21555=CARTESIAN_POINT('Ctrl Pts',(31.4201064027297,27.9647772671023,-10.7881590889261));
#21556=CARTESIAN_POINT('Ctrl Pts',(31.5947252847635,27.8131769557082,-10.7577973123345));
#21557=CARTESIAN_POINT('Ctrl Pts',(31.9461325502455,27.5845949906572,-10.64301467846));
#21558=CARTESIAN_POINT('Ctrl Pts',(32.1176525902707,27.5025425174008,-10.5663096364702));
#21559=CARTESIAN_POINT('Ctrl Pts',(32.2890256406393,27.4492538662306,-10.4702558451017));
#21560=CARTESIAN_POINT('',(33.313823818559,27.9721136596077,-9.34999999999999));
#21561=CARTESIAN_POINT('Ctrl Pts',(32.2890256406395,27.4492538662297,-10.4702558451021));
#21562=CARTESIAN_POINT('Ctrl Pts',(32.4674592300993,27.5545798270942,-10.2660883599925));
#21563=CARTESIAN_POINT('Ctrl Pts',(32.6497282149729,27.6540981522296,-10.0627168595853));
#21564=CARTESIAN_POINT('Ctrl Pts',(32.835796568896,27.74780805405,-9.86011238748894));
#21565=CARTESIAN_POINT('Ctrl Pts',(32.9924481468926,27.8267027380979,-9.68953899553974));
#21566=CARTESIAN_POINT('Ctrl Pts',(33.1517933649272,27.9014798009225,-9.51950878870952));
#21567=CARTESIAN_POINT('Ctrl Pts',(33.313823818559,27.9721136596077,-9.34999999999999));
#21568=CARTESIAN_POINT('',(35.3258686435729,25.383715342263,-9.34999999999999));
#21569=CARTESIAN_POINT('Origin',(-3.46944695195361E-15,3.46944695195361E-15,
-9.34999999999999));
#21570=CARTESIAN_POINT('',(34.5612980340057,24.5636585134986,-10.4488603765991));
#21571=CARTESIAN_POINT('Ctrl Pts',(35.3258686435729,25.383715342263,-9.34999999999999));
#21572=CARTESIAN_POINT('Ctrl Pts',(35.1915715573956,25.2210377598276,-9.55398902691078));
#21573=CARTESIAN_POINT('Ctrl Pts',(35.0525030950891,25.0637004493679,-9.75864153760484));
#21574=CARTESIAN_POINT('Ctrl Pts',(34.9086991356795,24.9117044745802,-9.96398744091905));
#21575=CARTESIAN_POINT('Ctrl Pts',(34.7958160748959,24.7923908553219,-10.1251796235311));
#21576=CARTESIAN_POINT('Ctrl Pts',(34.6800142414282,24.6763692246686,-10.286799316278));
#21577=CARTESIAN_POINT('Ctrl Pts',(34.5612980340057,24.5636585134986,-10.4488603765991));
#21578=CARTESIAN_POINT('',(35.8668060412405,22.5746525783803,-10.4702558451029));
#21579=CARTESIAN_POINT('Ctrl Pts',(34.561298034005,24.5636585134985,-10.4488603765997));
#21580=CARTESIAN_POINT('Ctrl Pts',(34.56674837864,24.3858737718396,-10.5474113291169));
#21581=CARTESIAN_POINT('Ctrl Pts',(34.5999432683243,24.2001880199589,-10.6271346460641));
#21582=CARTESIAN_POINT('Ctrl Pts',(34.7266314531113,23.8029384282025,-10.7492419673841));
#21583=CARTESIAN_POINT('Ctrl Pts',(34.8265396429607,23.5950253023348,-10.7838654923528));
#21584=CARTESIAN_POINT('Ctrl Pts',(35.0800977777163,23.2085887951713,-10.7881590889262));
#21585=CARTESIAN_POINT('Ctrl Pts',(35.2313643175126,23.0336806984012,-10.7577973123347));
#21586=CARTESIAN_POINT('Ctrl Pts',(35.5466641583307,22.7574149000112,-10.6430146784605));
#21587=CARTESIAN_POINT('Ctrl Pts',(35.7047610871982,22.6517877558659,-10.566309636471));
#21588=CARTESIAN_POINT('Ctrl Pts',(35.86680604124,22.5746525783811,-10.4702558451029));
#21589=CARTESIAN_POINT('',(36.9555839582819,22.9463464260082,-9.34999999999999));
#21590=CARTESIAN_POINT('Ctrl Pts',(35.8668060412405,22.5746525783803,-10.4702558451029));
#21591=CARTESIAN_POINT('Ctrl Pts',(36.0584128811214,22.653512725402,-10.2660883599983));
#21592=CARTESIAN_POINT('Ctrl Pts',(36.2529895648814,22.7260785163746,-10.062716859596));
#21593=CARTESIAN_POINT('Ctrl Pts',(36.4505003207673,22.792354298815,-9.86011238750467));
#21594=CARTESIAN_POINT('Ctrl Pts',(36.616785295779,22.8481521047499,-9.68953899555019));
#21595=CARTESIAN_POINT('Ctrl Pts',(36.7851504948585,22.8994908559617,-9.51950878871472));
#21596=CARTESIAN_POINT('Ctrl Pts',(36.9555839582819,22.9463464260082,-9.34999999999999));
#21597=CARTESIAN_POINT('',(38.5787815801853,20.0979504375039,-9.34999999999999));
#21598=CARTESIAN_POINT('Origin',(-3.46944695195361E-15,3.46944695195361E-15,
-9.34999999999999));
#21599=CARTESIAN_POINT('',(37.705286942044,19.3950503474818,-10.4488603765981));
#21600=CARTESIAN_POINT('Ctrl Pts',(38.5787815801853,20.0979504375039,-9.34999999999999));
#21601=CARTESIAN_POINT('Ctrl Pts',(38.4227000108675,19.9560411463938,-9.55398902691392));
#21602=CARTESIAN_POINT('Ctrl Pts',(38.2626556310921,19.820096808613,-9.75864153761112));
#21603=CARTESIAN_POINT('Ctrl Pts',(38.0986841060684,19.6901133709132,-9.9639874409285));
#21604=CARTESIAN_POINT('Ctrl Pts',(37.9699699336537,19.5880791268045,-10.1251796235371));
#21605=CARTESIAN_POINT('Ctrl Pts',(37.8388351962785,19.4897187482658,-10.2867993162805));
#21606=CARTESIAN_POINT('Ctrl Pts',(37.705286942044,19.3950503474818,-10.4488603765981));
#21607=CARTESIAN_POINT('',(38.7144417021698,17.2404964639591,-10.4702558451034));
#21608=CARTESIAN_POINT('Ctrl Pts',(37.7052869420443,19.3950503474814,-10.4488603765979));
#21609=CARTESIAN_POINT('Ctrl Pts',(37.6853804032726,19.2182995332333,-10.5474113291154));
#21610=CARTESIAN_POINT('Ctrl Pts',(37.6918115790941,19.0297796692134,-10.6271346460628));
#21611=CARTESIAN_POINT('Ctrl Pts',(37.7606757494237,18.6185438969855,-10.7492419673832));
#21612=CARTESIAN_POINT('Ctrl Pts',(37.8299778950733,18.3985286090725,-10.7838654923521));
#21613=CARTESIAN_POINT('Ctrl Pts',(38.0259595245977,17.9799403834156,-10.7881590889258));
#21614=CARTESIAN_POINT('Ctrl Pts',(38.1507943716225,17.7852851257265,-10.7577973123345));
#21615=CARTESIAN_POINT('Ctrl Pts',(38.4235681922673,17.4669594689679,-10.6430146784607));
#21616=CARTESIAN_POINT('Ctrl Pts',(38.5650236124193,17.3399079179848,-10.5663096364715));
#21617=CARTESIAN_POINT('Ctrl Pts',(38.7144417021694,17.2404964639595,-10.4702558451036));
#21618=CARTESIAN_POINT('',(39.8450349797172,17.4534577509763,-9.34999999999999));
#21619=CARTESIAN_POINT('Ctrl Pts',(38.7144417021698,17.2404964639591,-10.4702558451034));
#21620=CARTESIAN_POINT('Ctrl Pts',(38.9153212297648,17.2912854319613,-10.2660883599988));
#21621=CARTESIAN_POINT('Ctrl Pts',(39.118244592247,17.3354214585318,-10.0627168595964));
#21622=CARTESIAN_POINT('Ctrl Pts',(39.3231770006846,17.3729139377875,-9.86011238750502));
#21623=CARTESIAN_POINT('Ctrl Pts',(39.4957102901416,17.4044789831856,-9.68953899555042));
#21624=CARTESIAN_POINT('Ctrl Pts',(39.6696680403332,17.4313343138563,-9.51950878871483));
#21625=CARTESIAN_POINT('Ctrl Pts',(39.8450349797172,17.4534577509763,-9.34999999999999));
#21626=CARTESIAN_POINT('',(41.0463417758493,14.4030492195288,-9.34999999999999));
#21627=CARTESIAN_POINT('Origin',(-3.46944695195361E-15,3.46944695195361E-15,
-9.34999999999999));
#21628=CARTESIAN_POINT('',(40.081704941015,13.8316148870794,-10.4488603766));
#21629=CARTESIAN_POINT('Ctrl Pts',(41.0463417758493,14.4030492195288,-9.34999999999999));
#21630=CARTESIAN_POINT('Ctrl Pts',(40.8716530940425,14.2847970836798,-9.55398902691413));
#21631=CARTESIAN_POINT('Ctrl Pts',(40.6938908388429,14.1730131532654,-9.75864153761155));
#21632=CARTESIAN_POINT('Ctrl Pts',(40.5130897356021,14.067688340605,-9.96398744092918));
#21633=CARTESIAN_POINT('Ctrl Pts',(40.3711647009233,13.98501059461,-10.1251796235382));
#21634=CARTESIAN_POINT('Ctrl Pts',(40.2273665847295,13.9063138018416,-10.286799316282));
#21635=CARTESIAN_POINT('Ctrl Pts',(40.081704941015,13.8316148870794,-10.4488603766));
#21636=CARTESIAN_POINT('',(40.7739629732833,11.5553735590025,-10.4702558451001));
#21637=CARTESIAN_POINT('Ctrl Pts',(40.0817049410145,13.8316148870796,-10.4488603766004));
#21638=CARTESIAN_POINT('Ctrl Pts',(40.0368467585605,13.6594961371123,-10.5474113291177));
#21639=CARTESIAN_POINT('Ctrl Pts',(40.0163833003262,13.4719798817374,-10.6271346460648));
#21640=CARTESIAN_POINT('Ctrl Pts',(40.02602158028,13.0551295034541,-10.7492419673843));
#21641=CARTESIAN_POINT('Ctrl Pts',(40.0633068898957,12.8274909302863,-10.7838654923527));
#21642=CARTESIAN_POINT('Ctrl Pts',(40.197722393377,12.3852722353025,-10.7881590889254));
#21643=CARTESIAN_POINT('Ctrl Pts',(40.2935842701394,12.1748324364022,-10.7577973123335));
#21644=CARTESIAN_POINT('Ctrl Pts',(40.5182791822383,11.8209271136718,-10.6430146784588));
#21645=CARTESIAN_POINT('Ctrl Pts',(40.640213469245,11.6750375590429,-10.5663096364691));
#21646=CARTESIAN_POINT('Ctrl Pts',(40.7739629732828,11.5553735590024,-10.4702558451007));
#21647=CARTESIAN_POINT('',(41.9233559925618,11.6052670077401,-9.34999999999999));
#21648=CARTESIAN_POINT('Ctrl Pts',(40.7739629732833,11.5553735590025,-10.4702558451001));
#21649=CARTESIAN_POINT('Ctrl Pts',(40.9800258606994,11.5770574310607,-10.2660883599949));
#21650=CARTESIAN_POINT('Ctrl Pts',(41.1871649674267,11.5918652110069,-10.0627168595919));
#21651=CARTESIAN_POINT('Ctrl Pts',(41.3953471955567,11.5998111483204,-9.86011238749989));
#21652=CARTESIAN_POINT('Ctrl Pts',(41.5706165192284,11.6065008598841,-9.68953899554702));
#21653=CARTESIAN_POINT('Ctrl Pts',(41.7466255423886,11.6083260729267,-9.51950878871314));
#21654=CARTESIAN_POINT('Ctrl Pts',(41.9233559925618,11.6052670077401,-9.34999999999999));
#21655=CARTESIAN_POINT('',(42.6783168208273,8.41494345442032,-9.34999999999999));
#21656=CARTESIAN_POINT('Origin',(-3.46944695195361E-15,3.46944695195361E-15,
-9.34999999999999));
#21657=CARTESIAN_POINT('',(41.6421750134739,7.98660763468041,-10.4488603765993));
#21658=CARTESIAN_POINT('Ctrl Pts',(42.6783168208273,8.41494345442032,-9.34999999999999));
#21659=CARTESIAN_POINT('Ctrl Pts',(42.4885771843334,8.32275574630956,-9.55398902691263));
#21660=CARTESIAN_POINT('Ctrl Pts',(42.2967157806026,8.23740782172875,-9.75864153760853));
#21661=CARTESIAN_POINT('Ctrl Pts',(42.1027656882206,8.15888574356384,-9.96398744092461));
#21662=CARTESIAN_POINT('Ctrl Pts',(41.9505189757044,8.09724757616873,-10.1251796235349));
#21663=CARTESIAN_POINT('Ctrl Pts',(41.796984795657,8.03981640892943,-10.28679931628));
#21664=CARTESIAN_POINT('Ctrl Pts',(41.6421750134739,7.98660763468041,-10.4488603765993));
#21665=CARTESIAN_POINT('',(42.0034439406491,5.6350165713479,-10.4702558451019));
#21666=CARTESIAN_POINT('Ctrl Pts',(41.6421750134739,7.98660763468041,-10.4488603765993));
#21667=CARTESIAN_POINT('Ctrl Pts',(41.5732783705715,7.82262479039417,-10.5474113291168));
#21668=CARTESIAN_POINT('Ctrl Pts',(41.5263368552786,7.63992943387202,-10.6271346460642));
#21669=CARTESIAN_POINT('Ctrl Pts',(41.4765530372697,7.22595032113834,-10.7492419673841));
#21670=CARTESIAN_POINT('Ctrl Pts',(41.4810624894692,6.99532252760984,-10.7838654923528));
#21671=CARTESIAN_POINT('Ctrl Pts',(41.5511755548777,6.538475660675,-10.7881590889261));
#21672=CARTESIAN_POINT('Ctrl Pts',(41.616112990009,6.31653526801026,-10.7577973123345));
#21673=CARTESIAN_POINT('Ctrl Pts',(41.7881548531172,5.93425477109961,-10.6430146784602));
#21674=CARTESIAN_POINT('Ctrl Pts',(41.888085776524,5.77249710344601,-10.5663096364707));
#21675=CARTESIAN_POINT('Ctrl Pts',(42.0034439406485,5.6350165713482,-10.4702558451025));
#21676=CARTESIAN_POINT('',(43.1482383743694,5.52082649506359,-9.34999999999999));
#21677=CARTESIAN_POINT('Ctrl Pts',(42.0034439406491,5.6350165713479,-10.4702558451019));
#21678=CARTESIAN_POINT('Ctrl Pts',(42.2104953417366,5.62715392635685,-10.2660883599947));
#21679=CARTESIAN_POINT('Ctrl Pts',(42.4176334378376,5.61233201597956,-10.0627168595898));
#21680=CARTESIAN_POINT('Ctrl Pts',(42.624827495845,5.59056965497981,-9.86011238749592));
#21681=CARTESIAN_POINT('Ctrl Pts',(42.7992648757372,5.57224784947257,-9.68953899554438));
#21682=CARTESIAN_POINT('Ctrl Pts',(42.9737421357234,5.54900578881206,-9.51950878871182));
#21683=CARTESIAN_POINT('Ctrl Pts',(43.1482383743694,5.52082649506359,-9.34999999999999));
#21684=CARTESIAN_POINT('',(43.4414844094374,2.25553370726654,-9.34999999999999));
#21685=CARTESIAN_POINT('Origin',(-3.46944695195361E-15,3.46944695195361E-15,
-9.34999999999999));
#21686=CARTESIAN_POINT('Ctrl Pts',(43.4414844094374,2.25553370726654,-9.34999999999999));
#21687=CARTESIAN_POINT('Ctrl Pts',(43.2405563700923,2.19128710278242,-9.55398902691076));
#21688=CARTESIAN_POINT('Ctrl Pts',(43.0385015627283,2.13411262165513,-9.7586415376048));
#21689=CARTESIAN_POINT('Ctrl Pts',(42.8353507457808,2.08399176105678,-9.96398744091901));
#21690=CARTESIAN_POINT('Ctrl Pts',(42.67588165945,2.04464794759924,-10.1251796235315));
#21691=CARTESIAN_POINT('Ctrl Pts',(42.5157369286977,2.00965153883555,-10.2867993162788));
#21692=CARTESIAN_POINT('Ctrl Pts',(42.3549304887758,1.97901608230145,-10.4488603766003));
#21693=CARTESIAN_POINT('Origin',(-1.73472347597681E-15,-1.73472347597681E-15,
11.35));
#21694=CARTESIAN_POINT('Ctrl Pts',(8.41494345441915,-42.6783168208275,-9.34999999999999));
#21695=CARTESIAN_POINT('Ctrl Pts',(8.47350165196269,-42.6667708190677,-8.81583928864268));
#21696=CARTESIAN_POINT('Ctrl Pts',(8.53749789216075,-42.6540295511139,-8.29847152339217));
#21697=CARTESIAN_POINT('Ctrl Pts',(8.67708507802148,-42.6258516250367,-7.21668429187557));
#21698=CARTESIAN_POINT('Ctrl Pts',(8.74798535871021,-42.6113531950663,-6.68828131371252));
#21699=CARTESIAN_POINT('Ctrl Pts',(8.8148974458234,-42.5975067699932,-6.16441400296899));
#21700=CARTESIAN_POINT('Ctrl Pts',(10.821785190392,-42.1323980482125,-6.16441400296898));
#21701=CARTESIAN_POINT('Ctrl Pts',(10.9673906983499,-42.0949990013352,-6.69963387813806));
#21702=CARTESIAN_POINT('Ctrl Pts',(11.1049325306235,-42.0588790443691,-7.21760449588555));
#21703=CARTESIAN_POINT('Ctrl Pts',(11.369604888333,-41.988102864666,-8.28098049190398));
#21704=CARTESIAN_POINT('Ctrl Pts',(11.4933208311464,-41.9543450495947,-8.81289306231308));
#21705=CARTESIAN_POINT('Ctrl Pts',(11.6052670077404,-41.9233559925617,-9.34999999999999));
#21706=CARTESIAN_POINT('Origin',(-1.73472347597681E-15,-1.73472347597681E-15,
11.35));
#21707=CARTESIAN_POINT('Ctrl Pts',(4.71556960657991,-43.2436515951822,-6.16441400296899));
#21708=CARTESIAN_POINT('Ctrl Pts',(4.86501549971827,-43.2273550409941,-6.69963387813254));
#21709=CARTESIAN_POINT('Ctrl Pts',(5.00629776029487,-43.2111769767249,-7.21760449588749));
#21710=CARTESIAN_POINT('Ctrl Pts',(5.27834863560216,-43.1787880002625,-8.28098049191805));
#21711=CARTESIAN_POINT('Ctrl Pts',(5.405609566491,-43.1629804054675,-8.81289306231201));
#21712=CARTESIAN_POINT('Ctrl Pts',(5.52082649506267,-43.1482383743695,-9.34999999999999));
#21713=CARTESIAN_POINT('Ctrl Pts',(2.25553370726645,-43.4414844094374,-9.34999999999999));
#21714=CARTESIAN_POINT('Ctrl Pts',(2.31513903416692,-43.4383896297404,-8.81583928864891));
#21715=CARTESIAN_POINT('Ctrl Pts',(2.38029715641292,-43.4348856640963,-8.29847152332599));
#21716=CARTESIAN_POINT('Ctrl Pts',(2.52247368297688,-43.4268598764585,-7.21668429184531));
#21717=CARTESIAN_POINT('Ctrl Pts',(2.5947156427552,-43.4225991815798,-6.68828131367592));
#21718=CARTESIAN_POINT('Ctrl Pts',(2.66291721304302,-43.4184162760053,-6.16441400296897));
#21719=CARTESIAN_POINT('Origin',(-1.73472347597681E-15,-1.73472347597681E-15,
11.35));
#21720=CARTESIAN_POINT('Ctrl Pts',(14.4030492195297,-41.046341775849,-9.34999999999999));
#21721=CARTESIAN_POINT('Ctrl Pts',(14.4593682116851,-41.0265795953254,-8.81583928864243));
#21722=CARTESIAN_POINT('Ctrl Pts',(14.5208997909382,-41.0048604005364,-8.29847152344933));
#21723=CARTESIAN_POINT('Ctrl Pts',(14.6550564651938,-40.9571038072317,-7.21668089174327));
#21724=CARTESIAN_POINT('Ctrl Pts',(14.7231709221295,-40.9326630822678,-6.68828455624565));
#21725=CARTESIAN_POINT('Ctrl Pts',(14.787431786677,-40.9094348672085,-6.16441400296898));
#21726=CARTESIAN_POINT('Ctrl Pts',(16.7077004351884,-40.1634503767792,-6.16441400296897));
#21727=CARTESIAN_POINT('Ctrl Pts',(16.8465014496973,-40.105710173964,-6.69963387810965));
#21728=CARTESIAN_POINT('Ctrl Pts',(16.9775028986062,-40.0503836224622,-7.21760449589626));
#21729=CARTESIAN_POINT('Ctrl Pts',(17.2294087727606,-39.9426610384398,-8.28098049186901));
#21730=CARTESIAN_POINT('Ctrl Pts',(17.347061227683,-39.8916402148512,-8.81289306231304));
#21731=CARTESIAN_POINT('Ctrl Pts',(17.4534577509835,-39.8450349797141,-9.34999999999999));
#21732=CARTESIAN_POINT('Origin',(-1.73472347597681E-15,-1.73472347597681E-15,
11.35));
#21733=CARTESIAN_POINT('Ctrl Pts',(20.0979504375088,-38.5787815801827,-9.35));
#21734=CARTESIAN_POINT('Ctrl Pts',(20.1508837319947,-38.5512055219067,-8.81583928863476));
#21735=CARTESIAN_POINT('Ctrl Pts',(20.2086980447853,-38.520950540461,-8.29847152350441));
#21736=CARTESIAN_POINT('Ctrl Pts',(20.334692329685,-38.4545877635936,-7.21668429184472));
#21737=CARTESIAN_POINT('Ctrl Pts',(20.3986359710957,-38.4207017045448,-6.68828131367372));
#21738=CARTESIAN_POINT('Ctrl Pts',(20.4589366597946,-38.38856484359,-6.16441400296897));
#21739=CARTESIAN_POINT('Ctrl Pts',(22.2534950801302,-37.3768906775112,-6.16441400296898));
#21740=CARTESIAN_POINT('Ctrl Pts',(22.382666012821,-37.2999847427738,-6.69963387809245));
#21741=CARTESIAN_POINT('Ctrl Pts',(22.5044602666517,-37.2265778857695,-7.21760449589733));
#21742=CARTESIAN_POINT('Ctrl Pts',(22.7384715801301,-37.0841018185718,-8.28098049198328));
#21743=CARTESIAN_POINT('Ctrl Pts',(22.8476654824114,-37.0168566233269,-8.81289306231471));
#21744=CARTESIAN_POINT('Ctrl Pts',(22.9463464260018,-36.9555839582859,-9.34999999999999));
#21745=CARTESIAN_POINT('Origin',(-1.73472347597681E-15,-1.73472347597681E-15,
11.35));
#21746=CARTESIAN_POINT('Ctrl Pts',(25.3837153422573,-35.325868643577,-9.34999999999999));
#21747=CARTESIAN_POINT('Ctrl Pts',(25.4321853698649,-35.2910400765618,-8.81583928865113));
#21748=CARTESIAN_POINT('Ctrl Pts',(25.4851054835569,-35.2528652126025,-8.29847152324279));
#21749=CARTESIAN_POINT('Ctrl Pts',(25.6003732827136,-35.16924679404,-7.21668089167132));
#21750=CARTESIAN_POINT('Ctrl Pts',(25.6588428776096,-35.1266060300569,-6.68828455616324));
#21751=CARTESIAN_POINT('Ctrl Pts',(25.7139565811959,-35.0862143432485,-6.16441400296897));
#21752=CARTESIAN_POINT('Ctrl Pts',(27.3462727390257,-33.829445270102,-6.16441400296898));
#21753=CARTESIAN_POINT('Ctrl Pts',(27.4631840422152,-33.7349391864884,-6.69963387811431));
#21754=CARTESIAN_POINT('Ctrl Pts',(27.5732917211693,-33.6449463759102,-7.21760449589188));
#21755=CARTESIAN_POINT('Ctrl Pts',(27.7846446784427,-33.4706172274022,-8.28098049202515));
#21756=CARTESIAN_POINT('Ctrl Pts',(27.8831571551483,-33.3885165787492,-8.81289306232346));
#21757=CARTESIAN_POINT('Ctrl Pts',(27.9721136596011,-33.3138238185646,-9.34999999999998));
#21758=CARTESIAN_POINT('Origin',(-1.73472347597681E-15,-1.73472347597681E-15,
11.35));
#21759=CARTESIAN_POINT('Ctrl Pts',(30.15274100324,-31.3538228927755,-9.34999999999999));
#21760=CARTESIAN_POINT('Ctrl Pts',(30.195761053975,-31.3124508262114,-8.81583928863301));
#21761=CARTESIAN_POINT('Ctrl Pts',(30.2427096676391,-31.2671332098872,-8.29847152309517));
#21762=CARTESIAN_POINT('Ctrl Pts',(30.344904065072,-31.1679615880787,-7.21668089169457));
#21763=CARTESIAN_POINT('Ctrl Pts',(30.3967101103647,-31.1174337546518,-6.6882845561955));
#21764=CARTESIAN_POINT('Ctrl Pts',(30.44551449954,-31.0696096991627,-6.16441400296898));
#21765=CARTESIAN_POINT('Ctrl Pts',(31.8823591451049,-29.5933299130488,-6.16441400296898));
#21766=CARTESIAN_POINT('Ctrl Pts',(31.984630841798,-29.4831475518908,-6.69963387813157));
#21767=CARTESIAN_POINT('Ctrl Pts',(32.0808104710531,-29.378400781849,-7.21760449588776));
#21768=CARTESIAN_POINT('Ctrl Pts',(32.2652025353894,-29.1757673907798,-8.28098049202437));
#21769=CARTESIAN_POINT('Ctrl Pts',(32.3510281565927,-29.0804826211578,-8.81289306233601));
#21770=CARTESIAN_POINT('Ctrl Pts',(32.4284493240119,-28.9938902950258,-9.34999999999999));
#21771=CARTESIAN_POINT('Origin',(-1.73472347597681E-15,-1.73472347597681E-15,
11.35));
#21772=CARTESIAN_POINT('Ctrl Pts',(34.3079438107283,-26.7435037248284,-9.34999999999999));
#21773=CARTESIAN_POINT('Ctrl Pts',(34.3446381204109,-26.6964303746902,-8.81583928862145));
#21774=CARTESIAN_POINT('Ctrl Pts',(34.3846594956414,-26.6448925420002,-8.29847152310463));
#21775=CARTESIAN_POINT('Ctrl Pts',(34.4717001081413,-26.5321865651654,-7.21668089171778));
#21776=CARTESIAN_POINT('Ctrl Pts',(34.51578798215,-26.4748002632685,-6.68828455622075));
#21777=CARTESIAN_POINT('Ctrl Pts',(34.5572895402933,-26.4205173989522,-6.16441400296898));
#21778=CARTESIAN_POINT('Ctrl Pts',(35.7694126601179,-24.7547796990844,-6.16441400296898));
#21779=CARTESIAN_POINT('Ctrl Pts',(35.8549627934919,-24.6311640555206,-6.69963387812577));
#21780=CARTESIAN_POINT('Ctrl Pts',(35.9352564331632,-24.5137956681819,-7.21760449588857));
#21781=CARTESIAN_POINT('Ctrl Pts',(36.0889339138623,-24.2869830660677,-8.28098049192201));
#21782=CARTESIAN_POINT('Ctrl Pts',(36.1603255174261,-24.1804538985912,-8.81289306230615));
#21783=CARTESIAN_POINT('Ctrl Pts',(36.2246352761032,-24.0837247765644,-9.34999999999999));
#21784=CARTESIAN_POINT('Origin',(-1.73472347597681E-15,-1.73472347597681E-15,
11.35));
#21785=CARTESIAN_POINT('Ctrl Pts',(37.7647352670483,-21.588764907001,-9.35000993815262));
#21786=CARTESIAN_POINT('Ctrl Pts',(37.7943568453571,-21.5369485509418,-8.81584922680642));
#21787=CARTESIAN_POINT('Ctrl Pts',(37.8266368134661,-21.4802386995136,-8.29847152338959));
#21788=CARTESIAN_POINT('Ctrl Pts',(37.8967517451859,-21.3562927362902,-7.21668089172103));
#21789=CARTESIAN_POINT('Ctrl Pts',(37.9322239459333,-21.2932161855427,-6.68828455622328));
#21790=CARTESIAN_POINT('Ctrl Pts',(37.9655778209991,-21.23357955498,-6.16441400296897));
#21791=CARTESIAN_POINT('Ctrl Pts',(38.9283040838375,-19.4122935573384,-6.16441400296897));
#21792=CARTESIAN_POINT('Ctrl Pts',(38.9953910998897,-19.2777610893824,-6.69963387815563));
#21793=CARTESIAN_POINT('Ctrl Pts',(39.0581642030152,-19.150160366662,-7.21760449588037));
#21794=CARTESIAN_POINT('Ctrl Pts',(39.1779986697582,-18.9037858039865,-8.28098049192675));
#21795=CARTESIAN_POINT('Ctrl Pts',(39.2335029284966,-18.7881808653144,-8.8128930623207));
#21796=CARTESIAN_POINT('Ctrl Pts',(39.2833921172024,-18.6832840733669,-9.35));
#21797=CARTESIAN_POINT('Origin',(-1.73472347597681E-15,-1.73472347597681E-15,
11.35));
#21798=CARTESIAN_POINT('Ctrl Pts',(40.4527467088507,-15.9945391840333,-9.34999999999999));
#21799=CARTESIAN_POINT('Ctrl Pts',(40.4746925458677,-15.9390346536464,-8.81583928863806));
#21800=CARTESIAN_POINT('Ctrl Pts',(40.4985728888029,-15.8783091409716,-8.29847152339854));
#21801=CARTESIAN_POINT('Ctrl Pts',(40.5503346392115,-15.7456467907431,-7.21668429190581));
#21802=CARTESIAN_POINT('Ctrl Pts',(40.5764693694874,-15.6781632361046,-6.68828131374606));
#21803=CARTESIAN_POINT('Ctrl Pts',(40.6009964209531,-15.614387263859,-6.16441400296897));
#21804=CARTESIAN_POINT('Ctrl Pts',(41.2947274963708,-13.6746290991923,-6.16441400296898));
#21805=CARTESIAN_POINT('Ctrl Pts',(41.3419856969081,-13.5319184999507,-6.69963387813235));
#21806=CARTESIAN_POINT('Ctrl Pts',(41.3859603841398,-13.3966830245769,-7.21760449588791));
#21807=CARTESIAN_POINT('Ctrl Pts',(41.469512352753,-13.1357619769634,-8.28098049188705));
#21808=CARTESIAN_POINT('Ctrl Pts',(41.5079993600206,-13.0134346502621,-8.81289306230997));
#21809=CARTESIAN_POINT('Ctrl Pts',(41.5424523787385,-12.9025055845851,-9.34999999999999));
#21810=CARTESIAN_POINT('Origin',(-1.73472347597681E-15,-1.73472347597681E-15,
11.35));
#21811=CARTESIAN_POINT('Ctrl Pts',(42.31725633263,-10.0747117317813,-9.34999999999999));
#21812=CARTESIAN_POINT('Ctrl Pts',(42.3310796744042,-10.0166489392364,-8.81583928865039));
#21813=CARTESIAN_POINT('Ctrl Pts',(42.3460748083624,-9.95314299759242,-8.29847152349818));
#21814=CARTESIAN_POINT('Ctrl Pts',(42.3784298778726,-9.81446449364917,-7.21668429186938));
#21815=CARTESIAN_POINT('Ctrl Pts',(42.3946946831139,-9.74394846437754,-6.68828131370223));
#21816=CARTESIAN_POINT('Ctrl Pts',(42.4098958173845,-9.67733107621064,-6.16441400296897));
#21817=CARTESIAN_POINT('Ctrl Pts',(42.8205093412358,-7.65858862696908,-6.16441400296897));
#21818=CARTESIAN_POINT('Ctrl Pts',(42.8469766855802,-7.5106050726955,-6.69963387810951));
#21819=CARTESIAN_POINT('Ctrl Pts',(42.8712577590976,-7.37048784895445,-7.21760449589371));
#21820=CARTESIAN_POINT('Ctrl Pts',(42.9168263524529,-7.10033191646616,-8.28098049196745));
#21821=CARTESIAN_POINT('Ctrl Pts',(42.9375126237602,-6.97377243337836,-8.8128930623116));
#21822=CARTESIAN_POINT('Ctrl Pts',(42.9558281083822,-6.85906928986171,-9.34999999999999));
#21823=CARTESIAN_POINT('Origin',(-1.73472347597681E-15,-1.73472347597681E-15,
11.35));
#21824=CARTESIAN_POINT('Ctrl Pts',(43.3203086503665,-3.94979220174698,-9.34999999999999));
#21825=CARTESIAN_POINT('Ctrl Pts',(43.325728093523,-3.8903531380549,-8.81583928863827));
#21826=CARTESIAN_POINT('Ctrl Pts',(43.3315327608277,-3.82535956522521,-8.29847152323037));
#21827=CARTESIAN_POINT('Ctrl Pts',(43.3438225321466,-3.68348755612829,-7.21668089169733));
#21828=CARTESIAN_POINT('Ctrl Pts',(43.3498862347432,-3.61137542267607,-6.68828455619463));
#21829=CARTESIAN_POINT('Ctrl Pts',(43.3554520350114,-3.54327233497895,-6.16441400296897));
#21830=CARTESIAN_POINT('Ctrl Pts',(43.4745891000668,-1.48664137583803,-6.16441400296898));
#21831=CARTESIAN_POINT('Ctrl Pts',(43.4797267894152,-1.33639738493906,-6.69963387812117));
#21832=CARTESIAN_POINT('Ctrl Pts',(43.4838199565783,-1.19425079545893,-7.2176044958904));
#21833=CARTESIAN_POINT('Ctrl Pts',(43.4904775295168,-0.920359573847044,
-8.28098049193426));
#21834=CARTESIAN_POINT('Ctrl Pts',(43.492941952042,-0.792144320447485,-8.81289306231382));
#21835=CARTESIAN_POINT('Ctrl Pts',(43.4947470521204,-0.676002124309745,
-9.34999999999999));
#21836=CARTESIAN_POINT('Origin',(-1.73472347597681E-15,-1.73472347597681E-15,
11.35));
#21837=CARTESIAN_POINT('Ctrl Pts',(43.4414844094373,2.25553370726654,-9.34999999999999));
#21838=CARTESIAN_POINT('Ctrl Pts',(43.4383896297404,2.31513903416689,-8.81583928864678));
#21839=CARTESIAN_POINT('Ctrl Pts',(43.4348856640966,2.38029715640743,-8.29847152336333));
#21840=CARTESIAN_POINT('Ctrl Pts',(43.4268598764586,2.52247368297485,-7.21668429185844));
#21841=CARTESIAN_POINT('Ctrl Pts',(43.4225991815799,2.59471564275292,-6.6882813136911));
#21842=CARTESIAN_POINT('Ctrl Pts',(43.4184162760054,2.6629172130419,-6.16441400296898));
#21843=CARTESIAN_POINT('Ctrl Pts',(43.2436515951818,4.71556960658336,-6.16441400296898));
#21844=CARTESIAN_POINT('Ctrl Pts',(43.2273550409942,4.86501549971759,-6.6996338781248));
#21845=CARTESIAN_POINT('Ctrl Pts',(43.2111769767249,5.00629776029513,-7.21760449588901));
#21846=CARTESIAN_POINT('Ctrl Pts',(43.1787880002636,5.27834863559312,-8.28098049188509));
#21847=CARTESIAN_POINT('Ctrl Pts',(43.1629804054676,5.40560956649083,-8.81289306230564));
#21848=CARTESIAN_POINT('Ctrl Pts',(43.1482383743694,5.52082649506359,-9.34999999999999));
#21849=CARTESIAN_POINT('Origin',(-1.73472347597681E-15,-1.73472347597681E-15,
11.35));
#21850=CARTESIAN_POINT('Ctrl Pts',(42.6783168208273,8.41494345442032,-9.34999999999999));
#21851=CARTESIAN_POINT('Ctrl Pts',(42.6667708190677,8.47350165196264,-8.81583928865448));
#21852=CARTESIAN_POINT('Ctrl Pts',(42.654029551117,8.53749789214549,-8.29847152350322));
#21853=CARTESIAN_POINT('Ctrl Pts',(42.625851536471,8.67708551675633,-7.21668089172215));
#21854=CARTESIAN_POINT('Ctrl Pts',(42.6113532807691,8.74798494455602,-6.68828455622002));
#21855=CARTESIAN_POINT('Ctrl Pts',(42.5975067699923,8.81489744582799,-6.16441400296898));
#21856=CARTESIAN_POINT('Ctrl Pts',(42.1323980482129,10.8217851903902,-6.16441400296898));
#21857=CARTESIAN_POINT('Ctrl Pts',(42.0949990013376,10.9673906983404,-6.69963387811488));
#21858=CARTESIAN_POINT('Ctrl Pts',(42.0588790443691,11.1049325306234,-7.21760449589152));
#21859=CARTESIAN_POINT('Ctrl Pts',(41.9881028646612,11.3696048883509,-8.28098049197336));
#21860=CARTESIAN_POINT('Ctrl Pts',(41.9543450495945,11.4933208311469,-8.81289306231959));
#21861=CARTESIAN_POINT('Ctrl Pts',(41.9233559925618,11.60526700774,-9.34999999999999));
#21862=CARTESIAN_POINT('Origin',(-1.73472347597681E-15,-1.73472347597681E-15,
11.35));
#21863=CARTESIAN_POINT('Ctrl Pts',(41.0463417758493,14.4030492195288,-9.34999999999999));
#21864=CARTESIAN_POINT('Ctrl Pts',(41.0265795953255,14.4593682116847,-8.81583928863649));
#21865=CARTESIAN_POINT('Ctrl Pts',(41.0048604005271,14.5208997909645,-8.29847152324346));
#21866=CARTESIAN_POINT('Ctrl Pts',(40.9571039573323,14.6550560435348,-7.21668429184298));
#21867=CARTESIAN_POINT('Ctrl Pts',(40.9326629384941,14.7231713198794,-6.6882813136778));
#21868=CARTESIAN_POINT('Ctrl Pts',(40.9094348672085,14.7874317866772,-6.16441400296898));
#21869=CARTESIAN_POINT('Ctrl Pts',(40.1634514154035,16.7076979384513,-6.16440437552831));
#21870=CARTESIAN_POINT('Ctrl Pts',(40.105711212588,16.8464989529609,-6.69962425066112));
#21871=CARTESIAN_POINT('Ctrl Pts',(40.0503836224625,16.9775028986055,-7.21760449589682));
#21872=CARTESIAN_POINT('Ctrl Pts',(39.9426610384324,17.2294087727778,-8.28098049193118));
#21873=CARTESIAN_POINT('Ctrl Pts',(39.891640214852,17.3470612276812,-8.81289306231108));
#21874=CARTESIAN_POINT('Ctrl Pts',(39.8450349797172,17.4534577509763,-9.34999999999999));
#21875=CARTESIAN_POINT('Origin',(-1.73472347597681E-15,-1.73472347597681E-15,
11.35));
#21876=CARTESIAN_POINT('Ctrl Pts',(38.5787815801853,20.0979504375039,-9.34999999999999));
#21877=CARTESIAN_POINT('Ctrl Pts',(38.551205521908,20.1508837319923,-8.81583928865653));
#21878=CARTESIAN_POINT('Ctrl Pts',(38.5209505404534,20.2086980447997,-8.29847152339421));
#21879=CARTESIAN_POINT('Ctrl Pts',(38.4545875550103,20.3346927256946,-7.21668089168163));
#21880=CARTESIAN_POINT('Ctrl Pts',(38.420701903461,20.3986355978551,-6.68828455617096));
#21881=CARTESIAN_POINT('Ctrl Pts',(38.3885648435948,20.4589366597857,-6.16441400296898));
#21882=CARTESIAN_POINT('Ctrl Pts',(37.3768906775087,22.2534950801344,-6.16441400296899));
#21883=CARTESIAN_POINT('Ctrl Pts',(37.299984742768,22.3826660128308,-6.69963387811716));
#21884=CARTESIAN_POINT('Ctrl Pts',(37.2265778857701,22.5044602666508,-7.21760449589159));
#21885=CARTESIAN_POINT('Ctrl Pts',(37.0841018185842,22.7384715801098,-8.28098049189961));
#21886=CARTESIAN_POINT('Ctrl Pts',(37.0168566233263,22.8476654824123,-8.81289306230973));
#21887=CARTESIAN_POINT('Ctrl Pts',(36.9555839582819,22.9463464260082,-9.34999999999999));
#21888=CARTESIAN_POINT('Origin',(-1.73472347597681E-15,-1.73472347597681E-15,
11.35));
#21889=CARTESIAN_POINT('Ctrl Pts',(35.3258686435729,25.383715342263,-9.34999999999999));
#21890=CARTESIAN_POINT('Ctrl Pts',(35.2910400765608,25.4321853698662,-8.8158392886509));
#21891=CARTESIAN_POINT('Ctrl Pts',(35.2528652126222,25.4851054835298,-8.29847152347939));
#21892=CARTESIAN_POINT('Ctrl Pts',(35.1692467940428,25.6003732827099,-7.2166808917155));
#21893=CARTESIAN_POINT('Ctrl Pts',(35.1266060300575,25.6588428776089,-6.6882845562118));
#21894=CARTESIAN_POINT('Ctrl Pts',(35.0862143432449,25.7139565812008,-6.16441400296898));
#21895=CARTESIAN_POINT('Ctrl Pts',(33.8294452700945,27.346272739035,-6.16441400296899));
#21896=CARTESIAN_POINT('Ctrl Pts',(33.7349391864853,27.463184042219,-6.69963387811333));
#21897=CARTESIAN_POINT('Ctrl Pts',(33.6449463759122,27.5732917211668,-7.21760449589191));
#21898=CARTESIAN_POINT('Ctrl Pts',(33.4706172274441,27.7846446783919,-8.28098049178978));
#21899=CARTESIAN_POINT('Ctrl Pts',(33.388516578751,27.8831571551463,-8.81289306227819));
#21900=CARTESIAN_POINT('Ctrl Pts',(33.313823818559,27.9721136596077,-9.34999999999999));
#21901=CARTESIAN_POINT('Origin',(-1.73472347597681E-15,-1.73472347597681E-15,
11.35));
#21902=CARTESIAN_POINT('Ctrl Pts',(31.3538228927686,30.1527410032472,-9.34999999999999));
#21903=CARTESIAN_POINT('Ctrl Pts',(31.3124508262117,30.1957610539746,-8.81583928870648));
#21904=CARTESIAN_POINT('Ctrl Pts',(31.2671332099589,30.2427096675652,-8.29847152382584));
#21905=CARTESIAN_POINT('Ctrl Pts',(31.1679615880845,30.344904065066,-7.2166808917017));
#21906=CARTESIAN_POINT('Ctrl Pts',(31.1174337546515,30.396710110365,-6.68828455619383));
#21907=CARTESIAN_POINT('Ctrl Pts',(31.0696096991581,30.4455144995446,-6.16441400296898));
#21908=CARTESIAN_POINT('Ctrl Pts',(29.5933299130457,31.8823591451077,-6.16441400296898));
#21909=CARTESIAN_POINT('Ctrl Pts',(29.4831475518988,31.9846308417905,-6.69963387809554));
#21910=CARTESIAN_POINT('Ctrl Pts',(29.3784007818486,32.0808104710534,-7.2176044958975));
#21911=CARTESIAN_POINT('Ctrl Pts',(29.1757673907945,32.265202535376,-8.28098049194909));
#21912=CARTESIAN_POINT('Ctrl Pts',(29.0804826211604,32.3510281565903,-8.81289306230641));
#21913=CARTESIAN_POINT('Ctrl Pts',(28.9938902950294,32.4284493240087,-9.34999999999999));
#21914=CARTESIAN_POINT('Origin',(-1.73472347597681E-15,-1.73472347597681E-15,
11.35));
#21915=CARTESIAN_POINT('Ctrl Pts',(26.7435037248324,34.3079438107253,-9.34999999999999));
#21916=CARTESIAN_POINT('Ctrl Pts',(26.6964303746913,34.34463812041,-8.81583928865456));
#21917=CARTESIAN_POINT('Ctrl Pts',(26.6448925420221,34.3846594956245,-8.29847152331405));
#21918=CARTESIAN_POINT('Ctrl Pts',(26.5321865651601,34.4717001081453,-7.21668089167348));
#21919=CARTESIAN_POINT('Ctrl Pts',(26.4748002632605,34.5157879821561,-6.68828455616666));
#21920=CARTESIAN_POINT('Ctrl Pts',(26.4205173989462,34.5572895402979,-6.16441400296898));
#21921=CARTESIAN_POINT('Ctrl Pts',(24.7547796990912,35.7694126601132,-6.16441400296897));
#21922=CARTESIAN_POINT('Ctrl Pts',(24.631164055528,35.8549627934868,-6.69963387811261));
#21923=CARTESIAN_POINT('Ctrl Pts',(24.5137956681809,35.9352564331639,-7.21760449589143));
#21924=CARTESIAN_POINT('Ctrl Pts',(24.2869830660353,36.0889339138842,-8.28098049206058));
#21925=CARTESIAN_POINT('Ctrl Pts',(24.1804538985909,36.1603255174263,-8.8128930623247));
#21926=CARTESIAN_POINT('Ctrl Pts',(24.0837247765699,36.2246352760995,-9.34999999999999));
#21927=CARTESIAN_POINT('Origin',(-1.73472347597681E-15,-1.73472347597681E-15,
11.35));
#21928=CARTESIAN_POINT('Ctrl Pts',(21.588763942955,37.7647358181594,-9.34999999999999));
#21929=CARTESIAN_POINT('Ctrl Pts',(21.536947586891,37.7943573964709,-8.81583928863289));
#21930=CARTESIAN_POINT('Ctrl Pts',(21.4802386994667,37.8266368134926,-8.29847152300709));
#21931=CARTESIAN_POINT('Ctrl Pts',(21.3562931258567,37.8967515248122,-7.21668429183446));
#21932=CARTESIAN_POINT('Ctrl Pts',(21.2932158164189,37.9322241523787,-6.68828131367098));
#21933=CARTESIAN_POINT('Ctrl Pts',(21.2335795549855,37.965577820996,-6.16441400296897));
#21934=CARTESIAN_POINT('Ctrl Pts',(19.4122959772784,38.9283028770912,-6.1644043755283));
#21935=CARTESIAN_POINT('Ctrl Pts',(19.277763509337,38.995389893136,-6.699624250679));
#21936=CARTESIAN_POINT('Ctrl Pts',(19.1501603666614,39.0581642030155,-7.21760449589032));
#21937=CARTESIAN_POINT('Ctrl Pts',(18.9037858040018,39.1779986697508,-8.28098049186625));
#21938=CARTESIAN_POINT('Ctrl Pts',(18.7881808653155,39.233502928496,-8.81289306230204));
#21939=CARTESIAN_POINT('Ctrl Pts',(18.6832840733669,39.2833921172024,-9.34999999999999));
#21940=CARTESIAN_POINT('Origin',(-1.73472347597681E-15,-1.73472347597681E-15,
11.35));
#21941=CARTESIAN_POINT('Ctrl Pts',(15.9945391840345,40.4527467088502,-9.34999999999999));
#21942=CARTESIAN_POINT('Ctrl Pts',(15.9390346536467,40.4746925458676,-8.81583928865999));
#21943=CARTESIAN_POINT('Ctrl Pts',(15.8783091409914,40.4985728887952,-8.29847152355329));
#21944=CARTESIAN_POINT('Ctrl Pts',(15.7456467907371,40.5503346392138,-7.21668429185831));
#21945=CARTESIAN_POINT('Ctrl Pts',(15.6781632360945,40.5764693694913,-6.68828131368947));
#21946=CARTESIAN_POINT('Ctrl Pts',(15.6143872638506,40.6009964209563,-6.16441400296898));
#21947=CARTESIAN_POINT('Ctrl Pts',(13.6746290992085,41.2947274963655,-6.16441400296897));
#21948=CARTESIAN_POINT('Ctrl Pts',(13.531918499964,41.3419856969037,-6.69963387811841));
#21949=CARTESIAN_POINT('Ctrl Pts',(13.3966830245759,41.3859603841401,-7.21760449588863));
#21950=CARTESIAN_POINT('Ctrl Pts',(13.1357619769188,41.4695123527673,-8.28098049204476));
#21951=CARTESIAN_POINT('Ctrl Pts',(13.0134346502651,41.5079993600196,-8.81289306231732));
#21952=CARTESIAN_POINT('Ctrl Pts',(12.9025055846018,41.5424523787333,-9.35));
#21953=CARTESIAN_POINT('Origin',(-1.73472347597681E-15,-1.73472347597681E-15,
11.35));
#21954=CARTESIAN_POINT('Ctrl Pts',(10.0747117317978,42.317256332626,-9.34999999999999));
#21955=CARTESIAN_POINT('Ctrl Pts',(10.0166489392394,42.3310796744035,-8.81583928863872));
#21956=CARTESIAN_POINT('Ctrl Pts',(9.95314299752702,42.3460748083777,-8.29847152304224));
#21957=CARTESIAN_POINT('Ctrl Pts',(9.81446405776504,42.3784299795687,-7.21668089169946));
#21958=CARTESIAN_POINT('Ctrl Pts',(9.74394887671559,42.3946945890243,-6.68828455620137));
#21959=CARTESIAN_POINT('Ctrl Pts',(9.67733107622405,42.4098958173815,-6.16441400296897));
#21960=CARTESIAN_POINT('Ctrl Pts',(7.65858862696457,42.8205093412366,-6.16441400296897));
#21961=CARTESIAN_POINT('Ctrl Pts',(7.51060507268604,42.8469766855819,-6.69963387812706));
#21962=CARTESIAN_POINT('Ctrl Pts',(7.37048784895403,42.8712577590977,-7.21760449588847));
#21963=CARTESIAN_POINT('Ctrl Pts',(7.10033191648018,42.9168263524505,-8.28098049191645));
#21964=CARTESIAN_POINT('Ctrl Pts',(6.97377243337731,42.9375126237604,-8.81289306231198));
#21965=CARTESIAN_POINT('Ctrl Pts',(6.85906928985752,42.9558281083829,-9.35));
#21966=CARTESIAN_POINT('Origin',(-1.73472347597681E-15,-1.73472347597681E-15,
11.35));
#21967=CARTESIAN_POINT('Ctrl Pts',(3.94979220174152,43.320308650367,-9.34999999999999));
#21968=CARTESIAN_POINT('Ctrl Pts',(3.89035313805397,43.3257280935231,-8.81583928864517));
#21969=CARTESIAN_POINT('Ctrl Pts',(3.82535956525061,43.3315327608255,-8.29847152340904));
#21970=CARTESIAN_POINT('Ctrl Pts',(3.68348800204737,43.3438224935185,-7.21668429186925));
#21971=CARTESIAN_POINT('Ctrl Pts',(3.61137500115279,43.3498862691927,-6.68828131370428));
#21972=CARTESIAN_POINT('Ctrl Pts',(3.54327233497912,43.3554520350114,-6.16441400296898));
#21973=CARTESIAN_POINT('Ctrl Pts',(1.48664137583835,43.4745891000668,-6.16441400296897));
#21974=CARTESIAN_POINT('Ctrl Pts',(1.33639738494147,43.4797267894151,-6.69963387811528));
#21975=CARTESIAN_POINT('Ctrl Pts',(1.19425079545862,43.4838199565783,-7.21760449589258));
#21976=CARTESIAN_POINT('Ctrl Pts',(0.920359573842253,43.4904775295169,-8.2809804919506));
#21977=CARTESIAN_POINT('Ctrl Pts',(0.792144320446845,43.492941952042,-8.81289306231523));
#21978=CARTESIAN_POINT('Ctrl Pts',(0.676002124309571,43.4947470521204,-9.34999999999999));
#21979=CARTESIAN_POINT('Origin',(-1.73472347597681E-15,-1.73472347597681E-15,
11.35));
#21980=CARTESIAN_POINT('Ctrl Pts',(-2.25553370726646,43.4414844094374,-9.34999999999999));
#21981=CARTESIAN_POINT('Ctrl Pts',(-2.31513903416694,43.4383896297404,-8.81583928864895));
#21982=CARTESIAN_POINT('Ctrl Pts',(-2.38029715641292,43.4348856640963,-8.29847152332613));
#21983=CARTESIAN_POINT('Ctrl Pts',(-2.52247368297692,43.4268598764585,-7.21668429184511));
#21984=CARTESIAN_POINT('Ctrl Pts',(-2.59471564275521,43.4225991815798,-6.68828131367596));
#21985=CARTESIAN_POINT('Ctrl Pts',(-2.66291721304303,43.4184162760053,-6.16441400296898));
#21986=CARTESIAN_POINT('Ctrl Pts',(-4.71556960658337,43.2436515951818,-6.16441400296897));
#21987=CARTESIAN_POINT('Ctrl Pts',(-4.8650154997179,43.2273550409941,-6.69963387812718));
#21988=CARTESIAN_POINT('Ctrl Pts',(-5.00629776029438,43.2111769767249,-7.21760449588948));
#21989=CARTESIAN_POINT('Ctrl Pts',(-5.27834863559037,43.1787880002639,-8.28098049187636));
#21990=CARTESIAN_POINT('Ctrl Pts',(-5.40560956649133,43.1629804054675,-8.81289306230479));
#21991=CARTESIAN_POINT('Ctrl Pts',(-5.52082649506595,43.1482383743691,-9.34999999999999));
#21992=CARTESIAN_POINT('Origin',(-1.73472347597681E-15,-1.73472347597681E-15,
11.35));
#21993=CARTESIAN_POINT('Ctrl Pts',(-8.41494345442186,42.678316820827,-9.34999999999999));
#21994=CARTESIAN_POINT('Ctrl Pts',(-8.47350165196332,42.6667708190676,-8.81583928865055));
#21995=CARTESIAN_POINT('Ctrl Pts',(-8.53749789214447,42.6540295511172,-8.29847152350979));
#21996=CARTESIAN_POINT('Ctrl Pts',(-8.67708507802188,42.6258516250367,-7.21668429187095));
#21997=CARTESIAN_POINT('Ctrl Pts',(-8.74798535871346,42.6113531950656,-6.68828131370458));
#21998=CARTESIAN_POINT('Ctrl Pts',(-8.81489744582792,42.5975067699923,-6.16441400296897));
#21999=CARTESIAN_POINT('Ctrl Pts',(-10.8217851903811,42.1323980482153,-6.16441400296898));
#22000=CARTESIAN_POINT('Ctrl Pts',(-10.9673906983384,42.0949990013381,-6.69963387812129));
#22001=CARTESIAN_POINT('Ctrl Pts',(-11.1049325306246,42.0588790443689,-7.2176044958879));
#22002=CARTESIAN_POINT('Ctrl Pts',(-11.36960488837,41.9881028646561,-8.28098049203455));
#22003=CARTESIAN_POINT('Ctrl Pts',(-11.4933208311451,41.954345049595,-8.81289306232201));
#22004=CARTESIAN_POINT('Ctrl Pts',(-11.6052670077299,41.9233559925646,-9.34999999999999));
#22005=CARTESIAN_POINT('Origin',(-1.73472347597681E-15,-1.73472347597681E-15,
11.35));
#22006=CARTESIAN_POINT('Ctrl Pts',(-14.4030492195196,41.0463417758526,-9.34999999999999));
#22007=CARTESIAN_POINT('Ctrl Pts',(-14.4593682116834,41.026579595326,-8.81583928863168));
#22008=CARTESIAN_POINT('Ctrl Pts',(-14.5208997909904,41.0048604005178,-8.29847152306799));
#22009=CARTESIAN_POINT('Ctrl Pts',(-14.6550564651991,40.9571038072298,-7.21668089171361));
#22010=CARTESIAN_POINT('Ctrl Pts',(-14.7231709221274,40.9326630822685,-6.68828455621876));
#22011=CARTESIAN_POINT('Ctrl Pts',(-14.7874317866676,40.9094348672119,-6.16441400296897));
#22012=CARTESIAN_POINT('Ctrl Pts',(-16.7077004351661,40.1634503767885,-6.16441400296897));
#22013=CARTESIAN_POINT('Ctrl Pts',(-16.8465014496801,40.1057101739713,-6.69963387809185));
#22014=CARTESIAN_POINT('Ctrl Pts',(-16.9775028986086,40.0503836224612,-7.21760449589783));
#22015=CARTESIAN_POINT('Ctrl Pts',(-17.2294087728188,39.9426610384149,-8.2809804920777));
#22016=CARTESIAN_POINT('Ctrl Pts',(-17.3470612276791,39.8916402148528,-8.81289306232322));
#22017=CARTESIAN_POINT('Ctrl Pts',(-17.4534577509583,39.8450349797251,-9.34999999999999));
#22018=CARTESIAN_POINT('Origin',(-1.73472347597681E-15,-1.73472347597681E-15,
11.35));
#22019=CARTESIAN_POINT('Ctrl Pts',(-20.0979504374858,38.5787815801947,-9.34999999999999));
#22020=CARTESIAN_POINT('Ctrl Pts',(-20.1508837319902,38.5512055219091,-8.81583928863358));
#22021=CARTESIAN_POINT('Ctrl Pts',(-20.2086980448599,38.5209505404217,-8.29847152294191));
#22022=CARTESIAN_POINT('Ctrl Pts',(-20.3346927257031,38.4545875550058,-7.21668089166178));
#22023=CARTESIAN_POINT('Ctrl Pts',(-20.3986355978538,38.4207019034617,-6.68828455615817));
#22024=CARTESIAN_POINT('Ctrl Pts',(-20.4589366597763,38.3885648435998,-6.16441400296897));
#22025=CARTESIAN_POINT('Ctrl Pts',(-22.2534950801163,37.3768906775195,-6.16441400296897));
#22026=CARTESIAN_POINT('Ctrl Pts',(-22.3826660128241,37.299984742772,-6.6996338781274));
#22027=CARTESIAN_POINT('Ctrl Pts',(-22.5044602666512,37.2265778857698,-7.21760449588769));
#22028=CARTESIAN_POINT('Ctrl Pts',(-22.7384715801542,37.0841018185571,-8.28098049207543));
#22029=CARTESIAN_POINT('Ctrl Pts',(-22.8476674107164,37.0168554326535,-8.81290280339141));
#22030=CARTESIAN_POINT('Ctrl Pts',(-22.9463482217481,36.9555828432766,-9.35000977404799));
#22031=CARTESIAN_POINT('Origin',(-1.73472347597681E-15,-1.73472347597681E-15,
11.35));
#22032=CARTESIAN_POINT('Ctrl Pts',(-25.3837153422505,35.3258686435819,-9.35));
#22033=CARTESIAN_POINT('Ctrl Pts',(-25.4321853698649,35.2910400765618,-8.81583928862139));
#22034=CARTESIAN_POINT('Ctrl Pts',(-25.4851054835929,35.2528652125764,-8.29847152294655));
#22035=CARTESIAN_POINT('Ctrl Pts',(-25.6003732827113,35.1692467940417,-7.21668089172052));
#22036=CARTESIAN_POINT('Ctrl Pts',(-25.6588428775992,35.1266060300646,-6.68828455622536));
#22037=CARTESIAN_POINT('Ctrl Pts',(-25.7139565811841,35.0862143432572,-6.16441400296897));
#22038=CARTESIAN_POINT('Ctrl Pts',(-27.3462727390392,33.829445270091,-6.16441400296897));
#22039=CARTESIAN_POINT('Ctrl Pts',(-27.463184042233,33.7349391864739,-6.69963387815876));
#22040=CARTESIAN_POINT('Ctrl Pts',(-27.5732917211642,33.6449463759143,-7.21760449588191));
#22041=CARTESIAN_POINT('Ctrl Pts',(-27.7846446783725,33.4706172274601,-8.28098049170841));
#22042=CARTESIAN_POINT('Ctrl Pts',(-27.8831571551494,33.3885165787484,-8.81289306228552));
#22043=CARTESIAN_POINT('Ctrl Pts',(-27.9721136596209,33.313823818548,-9.34999999999999));
#22044=CARTESIAN_POINT('Origin',(-1.73472347597681E-15,-1.73472347597681E-15,
11.35));
#22045=CARTESIAN_POINT('Ctrl Pts',(-30.1527410032581,31.353822892758,-9.35));
#22046=CARTESIAN_POINT('Ctrl Pts',(-30.1957610539777,31.3124508262088,-8.81583928867595));
#22047=CARTESIAN_POINT('Ctrl Pts',(-30.2427096675459,31.2671332099776,-8.29847152400003));
#22048=CARTESIAN_POINT('Ctrl Pts',(-30.3449037438555,31.1679618997941,-7.2166842919219));
#22049=CARTESIAN_POINT('Ctrl Pts',(-30.3967104124394,31.1174334586449,-6.68828131375689));
#22050=CARTESIAN_POINT('Ctrl Pts',(-30.4455144995497,31.0696096991531,-6.16441400296897));
#22051=CARTESIAN_POINT('Ctrl Pts',(-31.8823591451153,29.5933299130376,-6.16441400296897));
#22052=CARTESIAN_POINT('Ctrl Pts',(-31.9846308417932,29.4831475518959,-6.69963387808623));
#22053=CARTESIAN_POINT('Ctrl Pts',(-32.080810471055,29.3784007818469,-7.21760449590099));
#22054=CARTESIAN_POINT('Ctrl Pts',(-32.2652025353664,29.175767390805,-8.28098049190116));
#22055=CARTESIAN_POINT('Ctrl Pts',(-32.351028156591,29.0804826211596,-8.81289306230433));
#22056=CARTESIAN_POINT('Ctrl Pts',(-32.4284493240122,28.9938902950255,-9.34999999999999));
#22057=CARTESIAN_POINT('Origin',(-1.73472347597681E-15,-1.73472347597681E-15,
11.35));
#22058=CARTESIAN_POINT('Ctrl Pts',(-34.3079438107289,26.7435037248276,-9.34999999999999));
#22059=CARTESIAN_POINT('Ctrl Pts',(-34.3446381204104,26.6964303746908,-8.81583928866682));
#22060=CARTESIAN_POINT('Ctrl Pts',(-34.3846594956096,26.6448925420414,-8.29847152347883));
#22061=CARTESIAN_POINT('Ctrl Pts',(-34.4717001081448,26.5321865651608,-7.21668089166674));
#22062=CARTESIAN_POINT('Ctrl Pts',(-34.5157879821584,26.4748002632575,-6.68828455615516));
#22063=CARTESIAN_POINT('Ctrl Pts',(-34.5572895403017,26.4205173989413,-6.16441400296897));
#22064=CARTESIAN_POINT('Ctrl Pts',(-35.7694126601179,24.7547796990843,-6.16441400296897));
#22065=CARTESIAN_POINT('Ctrl Pts',(-35.8549627934916,24.631164055521,-6.6996338781248));
#22066=CARTESIAN_POINT('Ctrl Pts',(-35.935256433163,24.5137956681822,-7.2176044958884));
#22067=CARTESIAN_POINT('Ctrl Pts',(-36.0889339138622,24.2869830660678,-8.2809804919214));
#22068=CARTESIAN_POINT('Ctrl Pts',(-36.1603255174268,24.1804538985902,-8.81289306230888));
#22069=CARTESIAN_POINT('Ctrl Pts',(-36.224635276104,24.0837247765632,-9.34999999999999));
#22070=CARTESIAN_POINT('Origin',(-1.73472347597681E-15,-1.73472347597681E-15,
11.35));
#22071=CARTESIAN_POINT('Ctrl Pts',(-37.7647358181634,21.5887639429479,-9.34999999999999));
#22072=CARTESIAN_POINT('Ctrl Pts',(-37.7943573964715,21.5369475868897,-8.81583928865539));
#22073=CARTESIAN_POINT('Ctrl Pts',(-37.8266368134634,21.4802386995183,-8.29847152342751));
#22074=CARTESIAN_POINT('Ctrl Pts',(-37.8967515248098,21.356293125861,-7.21668429186077));
#22075=CARTESIAN_POINT('Ctrl Pts',(-37.9322241523793,21.2932158164178,-6.68828131369573));
#22076=CARTESIAN_POINT('Ctrl Pts',(-37.9655778209998,21.2335795549787,-6.16441400296897));
#22077=CARTESIAN_POINT('Ctrl Pts',(-38.92830408384,19.4122935573335,-6.16441400296897));
#22078=CARTESIAN_POINT('Ctrl Pts',(-38.995391099886,19.2777610893897,-6.6996338781252));
#22079=CARTESIAN_POINT('Ctrl Pts',(-39.0581642030157,19.150160366661,-7.21760449589139));
#22080=CARTESIAN_POINT('Ctrl Pts',(-39.1779986697573,18.9037858039884,-8.28098049192254));
#22081=CARTESIAN_POINT('Ctrl Pts',(-39.2335029284966,18.7881808653144,-8.81289306231383));
#22082=CARTESIAN_POINT('Ctrl Pts',(-39.2833921172032,18.6832840733651,-9.34999999999999));
#22083=CARTESIAN_POINT('Origin',(-1.73472347597681E-15,-1.73472347597681E-15,
11.35));
#22084=CARTESIAN_POINT('Ctrl Pts',(-40.4527467088508,15.9945391840328,-9.34999999999999));
#22085=CARTESIAN_POINT('Ctrl Pts',(-40.4746925458678,15.9390346536462,-8.81583928863956));
#22086=CARTESIAN_POINT('Ctrl Pts',(-40.4985728888043,15.8783091409682,-8.29847152336921));
#22087=CARTESIAN_POINT('Ctrl Pts',(-40.5503348019053,15.7456463737683,-7.21668089171989));
#22088=CARTESIAN_POINT('Ctrl Pts',(-40.5764692176789,15.6781636308416,-6.68828455621838));
#22089=CARTESIAN_POINT('Ctrl Pts',(-40.6009964209562,15.6143872638508,-6.16441400296897));
#22090=CARTESIAN_POINT('Ctrl Pts',(-41.2947274963707,13.6746290991927,-6.16441400296901));
#22091=CARTESIAN_POINT('Ctrl Pts',(-41.3419856969067,13.5319184999549,-6.69963387811762));
#22092=CARTESIAN_POINT('Ctrl Pts',(-41.3859603841406,13.3966830245743,-7.21760449589209));
#22093=CARTESIAN_POINT('Ctrl Pts',(-41.4695123527587,13.1357619769457,-8.28098049195159));
#22094=CARTESIAN_POINT('Ctrl Pts',(-41.5079993600206,13.0134346502621,-8.81289306231735));
#22095=CARTESIAN_POINT('Ctrl Pts',(-41.5424523787372,12.9025055845893,-9.34999999999999));
#22096=CARTESIAN_POINT('Origin',(-1.73472347597681E-15,-1.73472347597681E-15,
11.35));
#22097=CARTESIAN_POINT('Ctrl Pts',(-42.3172560754436,10.0747128120527,-9.35000993815263));
#22098=CARTESIAN_POINT('Ctrl Pts',(-42.3310794172186,10.0166500195044,-8.81584922679741));
#22099=CARTESIAN_POINT('Ctrl Pts',(-42.3460748083683,9.95314299756727,-8.29847152331858));
#22100=CARTESIAN_POINT('Ctrl Pts',(-42.3784298778735,9.8144644936454,-7.21668429184823));
#22101=CARTESIAN_POINT('Ctrl Pts',(-42.3946946831143,9.74394846437601,-6.68828131367989));
#22102=CARTESIAN_POINT('Ctrl Pts',(-42.4098958173841,9.6773310762126,-6.16441400296897));
#22103=CARTESIAN_POINT('Ctrl Pts',(-42.8205093412364,7.65858862696564,-6.16441400296902));
#22104=CARTESIAN_POINT('Ctrl Pts',(-42.8469766855814,7.51060507268903,-6.69963387812033));
#22105=CARTESIAN_POINT('Ctrl Pts',(-42.8712577590977,7.37048784895363,-7.21760449589055));
#22106=CARTESIAN_POINT('Ctrl Pts',(-42.9168263524516,7.10033191647366,-8.28098049193938));
#22107=CARTESIAN_POINT('Ctrl Pts',(-42.9375126237604,6.97377243337723,-8.81289306231365));
#22108=CARTESIAN_POINT('Ctrl Pts',(-42.9558281083827,6.85906928985893,-9.34999999999999));
#22109=CARTESIAN_POINT('Origin',(-1.73472347597681E-15,-1.73472347597681E-15,
11.35));
#22110=CARTESIAN_POINT('Ctrl Pts',(-43.3203086503669,3.94979220174327,-9.34999999999999));
#22111=CARTESIAN_POINT('Ctrl Pts',(-43.325728093523,3.89035313805446,-8.81583928864667));
#22112=CARTESIAN_POINT('Ctrl Pts',(-43.3315327608263,3.82535956524115,-8.29847152334301));
#22113=CARTESIAN_POINT('Ctrl Pts',(-43.3438225321464,3.68348755613132,-7.21668089171067));
#22114=CARTESIAN_POINT('Ctrl Pts',(-43.3498862347431,3.61137542267791,-6.68828455620843));
#22115=CARTESIAN_POINT('Ctrl Pts',(-43.3554520350114,3.54327233497869,-6.16441400296897));
#22116=CARTESIAN_POINT('Ctrl Pts',(-43.4745891000669,1.48664137583783,-6.16441400296901));
#22117=CARTESIAN_POINT('Ctrl Pts',(-43.4797267894151,1.3363973849409,-6.69963387811629));
#22118=CARTESIAN_POINT('Ctrl Pts',(-43.4838199565783,1.19425079545889,-7.21760449589232));
#22119=CARTESIAN_POINT('Ctrl Pts',(-43.4904775295169,0.920359573845538,
-8.28098049193959));
#22120=CARTESIAN_POINT('Ctrl Pts',(-43.492941952042,0.792144320446992,-8.81289306231399));
#22121=CARTESIAN_POINT('Ctrl Pts',(-43.4947470521204,0.676002124309095,
-9.34999999999999));
#22122=CARTESIAN_POINT('Origin',(-1.73472347597681E-15,-1.73472347597681E-15,
11.35));
#22123=CARTESIAN_POINT('Ctrl Pts',(-43.4414844094373,-2.25553370726721,
-9.34999999999999));
#22124=CARTESIAN_POINT('Ctrl Pts',(-43.4383896297404,-2.31513903416679,
-8.81583928865233));
#22125=CARTESIAN_POINT('Ctrl Pts',(-43.4348856640966,-2.38029715640739,
-8.29847152336314));
#22126=CARTESIAN_POINT('Ctrl Pts',(-43.4268598764585,-2.52247368297661,
-7.21668429184337));
#22127=CARTESIAN_POINT('Ctrl Pts',(-43.4225991815797,-2.59471564275568,
-6.68828131367366));
#22128=CARTESIAN_POINT('Ctrl Pts',(-43.4184162760052,-2.66291721304384,
-6.16441400296897));
#22129=CARTESIAN_POINT('Ctrl Pts',(-43.2436515951816,-4.71556960658529,
-6.16441400296901));
#22130=CARTESIAN_POINT('Ctrl Pts',(-43.2273550409947,-4.86501549971271,
-6.699633878108));
#22131=CARTESIAN_POINT('Ctrl Pts',(-43.2111769767248,-5.0062977602958,-7.21760449589389));
#22132=CARTESIAN_POINT('Ctrl Pts',(-43.1787880002633,-5.27834863559578,
-8.2809804918952));
#22133=CARTESIAN_POINT('Ctrl Pts',(-43.1629804054676,-5.40560956649091,
-8.81289306230376));
#22134=CARTESIAN_POINT('Ctrl Pts',(-43.1482383743694,-5.5208264950638,-9.34999999999999));
#22135=CARTESIAN_POINT('Origin',(-1.73472347597681E-15,-1.73472347597681E-15,
11.35));
#22136=CARTESIAN_POINT('Ctrl Pts',(-42.6783168208273,-8.41494345442028,
-9.34999999999999));
#22137=CARTESIAN_POINT('Ctrl Pts',(-42.6667708190676,-8.47350165196288,
-8.8158392886554));
#22138=CARTESIAN_POINT('Ctrl Pts',(-42.6540295511159,-8.53749789215064,
-8.29847152346515));
#22139=CARTESIAN_POINT('Ctrl Pts',(-42.6258515364705,-8.67708551675907,
-7.21668089169991));
#22140=CARTESIAN_POINT('Ctrl Pts',(-42.6113532807684,-8.74798494455966,
-6.68828455619364));
#22141=CARTESIAN_POINT('Ctrl Pts',(-42.5975067699919,-8.81489744582999,
-6.16441400296896));
#22142=CARTESIAN_POINT('Ctrl Pts',(-42.1323980482118,-10.8217851903945,
-6.16441400296901));
#22143=CARTESIAN_POINT('Ctrl Pts',(-42.0949990013363,-10.9673906983452,
-6.69963387812546));
#22144=CARTESIAN_POINT('Ctrl Pts',(-42.0588790443698,-11.104932530621,-7.21760449589023));
#22145=CARTESIAN_POINT('Ctrl Pts',(-41.9881028646677,-11.3696048883265,
-8.28098049188592));
#22146=CARTESIAN_POINT('Ctrl Pts',(-41.9543450495943,-11.4933208311478,
-8.81289306230854));
#22147=CARTESIAN_POINT('Ctrl Pts',(-41.9233559925594,-11.6052670077487,
-9.34999999999999));
#22148=CARTESIAN_POINT('Origin',(-1.73472347597681E-15,-1.73472347597681E-15,
11.35));
#22149=CARTESIAN_POINT('Ctrl Pts',(-41.0463417758467,-14.4030492195362,
-9.34999999999999));
#22150=CARTESIAN_POINT('Ctrl Pts',(-41.0265795953249,-14.4593682116866,
-8.81583928863918));
#22151=CARTESIAN_POINT('Ctrl Pts',(-41.0048604005375,-14.5208997909351,
-8.29847152346152));
#22152=CARTESIAN_POINT('Ctrl Pts',(-40.9571039573334,-14.6550560435318,
-7.21668429186506));
#22153=CARTESIAN_POINT('Ctrl Pts',(-40.9326629384938,-14.7231713198805,
-6.68828131370069));
#22154=CARTESIAN_POINT('Ctrl Pts',(-40.9094348672063,-14.7874317866831,
-6.16441400296897));
#22155=CARTESIAN_POINT('Ctrl Pts',(-40.1634514153995,-16.7076979384609,
-6.16440437552835));
#22156=CARTESIAN_POINT('Ctrl Pts',(-40.1057112125809,-16.8464989529779,
-6.69962425069541));
#22157=CARTESIAN_POINT('Ctrl Pts',(-40.0503836224627,-16.977502898605,-7.21760449588796));
#22158=CARTESIAN_POINT('Ctrl Pts',(-39.9426610384488,-17.2294087727396,
-8.28098049178294));
#22159=CARTESIAN_POINT('Ctrl Pts',(-39.8916402148513,-17.3470612276828,
-8.81289306230247));
#22160=CARTESIAN_POINT('Ctrl Pts',(-39.845034979713,-17.4534577509859,-9.34999999999999));
#22161=CARTESIAN_POINT('Origin',(-1.73472347597681E-15,-1.73472347597681E-15,
11.35));
#22162=CARTESIAN_POINT('Ctrl Pts',(-38.5787815801808,-20.0979504375124,
-9.34999999999999));
#22163=CARTESIAN_POINT('Ctrl Pts',(-38.5512055219064,-20.1508837319952,
-8.81583928865245));
#22164=CARTESIAN_POINT('Ctrl Pts',(-38.5209505404797,-20.2086980447498,
-8.29847152379691));
#22165=CARTESIAN_POINT('Ctrl Pts',(-38.4545877635967,-20.334692329679,-7.21668429188963));
#22166=CARTESIAN_POINT('Ctrl Pts',(-38.4207017045473,-20.398635971091,-6.68828131372094));
#22167=CARTESIAN_POINT('Ctrl Pts',(-38.3885648435901,-20.4589366597944,
-6.16441400296898));
#22168=CARTESIAN_POINT('Ctrl Pts',(-37.3768920608804,-22.253492756628,-6.16440437552834));
#22169=CARTESIAN_POINT('Ctrl Pts',(-37.2999861261424,-22.3826636893199,
-6.69962425065386));
#22170=CARTESIAN_POINT('Ctrl Pts',(-37.2265778857679,-22.5044602666544,
-7.21760449589713));
#22171=CARTESIAN_POINT('Ctrl Pts',(-37.0841018185697,-22.7384715801335,
-8.28098049199277));
#22172=CARTESIAN_POINT('Ctrl Pts',(-37.0168566233265,-22.847665482412,-8.8128930623192));
#22173=CARTESIAN_POINT('Ctrl Pts',(-36.955583958287,-22.946346426,-9.34999999999999));
#22174=CARTESIAN_POINT('Origin',(-1.73472347597681E-15,-1.73472347597681E-15,
11.35));
#22175=CARTESIAN_POINT('Ctrl Pts',(-35.3258692915697,-25.3837144404623,
-9.35000993815263));
#22176=CARTESIAN_POINT('Ctrl Pts',(-35.2910407245523,-25.4321844680731,
-8.81584922678877));
#22177=CARTESIAN_POINT('Ctrl Pts',(-35.252865212596,-25.4851054835659,-8.29847152317624));
#22178=CARTESIAN_POINT('Ctrl Pts',(-35.1692467940378,-25.6003732827167,
-7.21668089167782));
#22179=CARTESIAN_POINT('Ctrl Pts',(-35.1266060300552,-25.658842877612,-6.6882845561739));
#22180=CARTESIAN_POINT('Ctrl Pts',(-35.0862143432467,-25.7139565811984,
-6.16441400296897));
#22181=CARTESIAN_POINT('Ctrl Pts',(-33.8294452700949,-27.3462727390344,
-6.16441400296902));
#22182=CARTESIAN_POINT('Ctrl Pts',(-33.7349391864802,-27.4631840422253,
-6.69963387813819));
#22183=CARTESIAN_POINT('Ctrl Pts',(-33.6449463759126,-27.5732917211663,
-7.21760449588766));
#22184=CARTESIAN_POINT('Ctrl Pts',(-33.4706172274317,-27.7846446784069,
-8.28098049186743));
#22185=CARTESIAN_POINT('Ctrl Pts',(-33.3885165787479,-27.88315715515,-8.8128930623081));
#22186=CARTESIAN_POINT('Ctrl Pts',(-33.3138238185527,-27.9721136596152,
-9.34999999999999));
#22187=CARTESIAN_POINT('Origin',(-1.73472347597681E-15,-1.73472347597681E-15,
11.35));
#22188=CARTESIAN_POINT('Ctrl Pts',(-31.3538228927626,-30.1527410032535,
-9.34999999999999));
#22189=CARTESIAN_POINT('Ctrl Pts',(-31.3124508262098,-30.1957610539767,
-8.81583928865918));
#22190=CARTESIAN_POINT('Ctrl Pts',(-31.2671332099354,-30.2427096675894,
-8.29847152356755));
#22191=CARTESIAN_POINT('Ctrl Pts',(-31.1679615880869,-30.3449040650636,
-7.21668089173702));
#22192=CARTESIAN_POINT('Ctrl Pts',(-31.1174337546538,-30.3967101103627,
-6.68828455623348));
#22193=CARTESIAN_POINT('Ctrl Pts',(-31.069609699158,-30.4455144995448,-6.16441400296898));
#22194=CARTESIAN_POINT('Ctrl Pts',(-29.5933299130507,-31.8823591451032,
-6.16441400296901));
#22195=CARTESIAN_POINT('Ctrl Pts',(-29.4831475518907,-31.9846308417981,
-6.69963387813632));
#22196=CARTESIAN_POINT('Ctrl Pts',(-29.3784007818493,-32.0808104710528,
-7.21760449588548));
#22197=CARTESIAN_POINT('Ctrl Pts',(-29.1757673907854,-32.2652025353842,
-8.280980491991));
#22198=CARTESIAN_POINT('Ctrl Pts',(-29.0804826211579,-32.3510281565926,
-8.81289306232937));
#22199=CARTESIAN_POINT('Ctrl Pts',(-28.9938902950281,-32.4284493240099,
-9.34999999999999));
#22200=CARTESIAN_POINT('Origin',(-1.73472347597681E-15,-1.73472347597681E-15,
11.35));
#22201=CARTESIAN_POINT('Ctrl Pts',(-26.7435037248304,-34.3079438107268,
-9.34999999999999));
#22202=CARTESIAN_POINT('Ctrl Pts',(-26.6964303746899,-34.344638120411,-8.8158392886314));
#22203=CARTESIAN_POINT('Ctrl Pts',(-26.6448925420125,-34.3846594956319,
-8.29847152322916));
#22204=CARTESIAN_POINT('Ctrl Pts',(-26.5321865651666,-34.4717001081404,
-7.2166808917316));
#22205=CARTESIAN_POINT('Ctrl Pts',(-26.4748002632703,-34.5157879821486,
-6.68828455623219));
#22206=CARTESIAN_POINT('Ctrl Pts',(-26.4205173989538,-34.5572895402921,
-6.16441400296898));
#22207=CARTESIAN_POINT('Ctrl Pts',(-24.7547796990836,-35.7694126601185,
-6.16441400296901));
#22208=CARTESIAN_POINT('Ctrl Pts',(-24.6311640555348,-35.854962793482,-6.69963387807314));
#22209=CARTESIAN_POINT('Ctrl Pts',(-24.5137956681789,-35.9352564331652,
-7.21760449590187));
#22210=CARTESIAN_POINT('Ctrl Pts',(-24.2869830660437,-36.0889339138785,
-8.28098049202429));
#22211=CARTESIAN_POINT('Ctrl Pts',(-24.1804538985908,-36.1603255174264,
-8.81289306231515));
#22212=CARTESIAN_POINT('Ctrl Pts',(-24.0837247765702,-36.2246352760993,
-9.34999999999999));
#22213=CARTESIAN_POINT('Origin',(-1.73472347597681E-15,-1.73472347597681E-15,
11.35));
#22214=CARTESIAN_POINT('Ctrl Pts',(-21.5887639429553,-37.7647358181592,
-9.34999999999999));
#22215=CARTESIAN_POINT('Ctrl Pts',(-21.5369475868915,-37.7943573964706,
-8.81583928865988));
#22216=CARTESIAN_POINT('Ctrl Pts',(-21.4802386994815,-37.8266368134842,
-8.29847152312796));
#22217=CARTESIAN_POINT('Ctrl Pts',(-21.3562931258516,-37.8967515248151,
-7.21668429177588));
#22218=CARTESIAN_POINT('Ctrl Pts',(-21.2932158164099,-37.9322241523837,
-6.68828131359938));
#22219=CARTESIAN_POINT('Ctrl Pts',(-21.2335795549793,-37.9655778209995,
-6.16441400296897));
#22220=CARTESIAN_POINT('Ctrl Pts',(-19.4122935573269,-38.9283040838433,
-6.16441400296902));
#22221=CARTESIAN_POINT('Ctrl Pts',(-19.2777610893895,-38.9953910998861,
-6.69963387811522));
#22222=CARTESIAN_POINT('Ctrl Pts',(-19.1501603666615,-39.0581642030155,
-7.21760449589381));
#22223=CARTESIAN_POINT('Ctrl Pts',(-18.9037858039981,-39.1779986697526,
-8.28098049188953));
#22224=CARTESIAN_POINT('Ctrl Pts',(-18.7881808653121,-39.2335029284977,
-8.81289306231679));
#22225=CARTESIAN_POINT('Ctrl Pts',(-18.6832840733583,-39.2833921172065,
-9.34999999999999));
#22226=CARTESIAN_POINT('Origin',(-1.73472347597681E-15,-1.73472347597681E-15,
11.35));
#22227=CARTESIAN_POINT('Ctrl Pts',(-15.9945391840253,-40.4527467088538,
-9.34999999999999));
#22228=CARTESIAN_POINT('Ctrl Pts',(-15.9390346536446,-40.4746925458684,
-8.81583928864358));
#22229=CARTESIAN_POINT('Ctrl Pts',(-15.8783091409867,-40.498572888797,-8.29847152349527));
#22230=CARTESIAN_POINT('Ctrl Pts',(-15.7456463737691,-40.550334801905,-7.21668089170353));
#22231=CARTESIAN_POINT('Ctrl Pts',(-15.6781636308371,-40.5764692176807,
-6.68828455619327));
#22232=CARTESIAN_POINT('Ctrl Pts',(-15.6143872638446,-40.6009964209586,
-6.16441400296898));
#22233=CARTESIAN_POINT('Ctrl Pts',(-13.6746290992012,-41.2947274963679,
-6.16441400296902));
#22234=CARTESIAN_POINT('Ctrl Pts',(-13.5319184999655,-41.3419856969032,
-6.69963387810014));
#22235=CARTESIAN_POINT('Ctrl Pts',(-13.3966830245737,-41.3859603841408,
-7.21760449589543));
#22236=CARTESIAN_POINT('Ctrl Pts',(-13.1357619769182,-41.4695123527675,
-8.28098049205013));
#22237=CARTESIAN_POINT('Ctrl Pts',(-13.0134346502636,-41.5079993600201,
-8.81289306232158));
#22238=CARTESIAN_POINT('Ctrl Pts',(-12.9025055845986,-41.5424523787343,
-9.34999999999999));
#22239=CARTESIAN_POINT('Origin',(-1.73472347597681E-15,-1.73472347597681E-15,
11.35));
#22240=CARTESIAN_POINT('Ctrl Pts',(-10.074711731795,-42.3172563326267,-9.35));
#22241=CARTESIAN_POINT('Ctrl Pts',(-10.0166489392386,-42.3310796744037,
-8.81583928863731));
#22242=CARTESIAN_POINT('Ctrl Pts',(-9.95314299752523,-42.3460748083781,
-8.29847152302227));
#22243=CARTESIAN_POINT('Ctrl Pts',(-9.81446405776189,-42.3784299795695,
-7.21668089167201));
#22244=CARTESIAN_POINT('Ctrl Pts',(-9.7439488767096,-42.3946945890256,-6.68828455616903));
#22245=CARTESIAN_POINT('Ctrl Pts',(-9.67733107621878,-42.4098958173827,
-6.16441400296897));
#22246=CARTESIAN_POINT('Ctrl Pts',(-7.65858862696401,-42.8205093412367,
-6.16441400296901));
#22247=CARTESIAN_POINT('Ctrl Pts',(-7.51060507269031,-42.8469766855811,
-6.69963387811412));
#22248=CARTESIAN_POINT('Ctrl Pts',(-7.3704878489533,-42.8712577590978,-7.21760449589294));
#22249=CARTESIAN_POINT('Ctrl Pts',(-7.10033191647729,-42.916826352451,-8.28098049192608));
#22250=CARTESIAN_POINT('Ctrl Pts',(-6.9737724333775,-42.9375126237603,-8.81289306230911));
#22251=CARTESIAN_POINT('Ctrl Pts',(-6.85906928985838,-42.9558281083827,
-9.34999999999999));
#22252=CARTESIAN_POINT('Origin',(-1.73472347597681E-15,-1.73472347597681E-15,
11.35));
#22253=CARTESIAN_POINT('Ctrl Pts',(-3.94979220174291,-43.3203086503669,
-9.34999999999999));
#22254=CARTESIAN_POINT('Ctrl Pts',(-3.8903531380541,-43.325728093523,-8.81583928864717));
#22255=CARTESIAN_POINT('Ctrl Pts',(-3.82535956524451,-43.331532760826,-8.29847152336844));
#22256=CARTESIAN_POINT('Ctrl Pts',(-3.683488002044,-43.3438224935188,-7.2166842918505));
#22257=CARTESIAN_POINT('Ctrl Pts',(-3.61137500114881,-43.349886269193,-6.68828131368176));
#22258=CARTESIAN_POINT('Ctrl Pts',(-3.5432723349768,-43.3554520350116,-6.16441400296897));
#22259=CARTESIAN_POINT('Ctrl Pts',(-1.48664137583836,-43.4745891000668,
-6.16441400296897));
#22260=CARTESIAN_POINT('Ctrl Pts',(-1.33639738494146,-43.4797267894151,
-6.69963387811538));
#22261=CARTESIAN_POINT('Ctrl Pts',(-1.19425079545864,-43.4838199565783,
-7.2176044958926));
#22262=CARTESIAN_POINT('Ctrl Pts',(-0.920359573842274,-43.4904775295169,
-8.28098049195057));
#22263=CARTESIAN_POINT('Ctrl Pts',(-0.792144320446858,-43.492941952042,
-8.81289306231522));
#22264=CARTESIAN_POINT('Ctrl Pts',(-0.676002124309579,-43.4947470521204,
-9.34999999999999));
#22265=CARTESIAN_POINT('Origin',(-1.73472347597681E-15,-1.73472347597681E-15,
11.35));
#22266=CARTESIAN_POINT('Ctrl Pts',(4.71518277776759,-43.2436937757663,6.16441400296896));
#22267=CARTESIAN_POINT('Ctrl Pts',(4.8650977532406,-43.2273474267669,6.70062138560741));
#22268=CARTESIAN_POINT('Ctrl Pts',(5.00655712290831,-43.2111479469791,7.21784327704619));
#22269=CARTESIAN_POINT('Ctrl Pts',(5.27969251824256,-43.178626142302,8.28373602794635));
#22270=CARTESIAN_POINT('Ctrl Pts',(5.40632229142204,-43.1628906187996,8.81321169230961));
#22271=CARTESIAN_POINT('Ctrl Pts',(5.52134683388059,-43.1481717937157,9.34999999998855));
#22272=CARTESIAN_POINT('Ctrl Pts',(2.25607198755898,-43.4414564579384,9.34999999999998));
#22273=CARTESIAN_POINT('Ctrl Pts',(2.31575404873037,-43.4383569525961,8.81613492203368));
#22274=CARTESIAN_POINT('Ctrl Pts',(2.38157881405563,-43.4348138690301,8.29345816615258));
#22275=CARTESIAN_POINT('Ctrl Pts',(2.52277267021435,-43.4268424365167,7.21621981188664));
#22276=CARTESIAN_POINT('Ctrl Pts',(2.59475150835134,-43.4225967225811,6.68773441334971));
#22277=CARTESIAN_POINT('Ctrl Pts',(2.66275246602647,-43.4184263798755,6.16441400296896));
#22278=CARTESIAN_POINT('Origin',(-1.73472347597681E-15,-1.73472347597681E-15,
11.35));
#22279=CARTESIAN_POINT('Ctrl Pts',(8.41547227788092,-42.6782125485618,9.34999999998854));
#22280=CARTESIAN_POINT('Ctrl Pts',(8.47410575612226,-42.6666509488314,8.81613492202544));
#22281=CARTESIAN_POINT('Ctrl Pts',(8.53875628688305,-42.6537760879159,8.29345816614668));
#22282=CARTESIAN_POINT('Ctrl Pts',(8.67737854004119,-42.6257918122874,7.21621981188599));
#22283=CARTESIAN_POINT('Ctrl Pts',(8.74802050929878,-42.6113456568892,6.68773441334886));
#22284=CARTESIAN_POINT('Ctrl Pts',(8.81473581362626,-42.5975402169653,6.16441400296897));
#22285=CARTESIAN_POINT('Ctrl Pts',(10.8214083018597,-42.1324948509395,6.16441400296896));
#22286=CARTESIAN_POINT('Ctrl Pts',(10.9674710310278,-42.0949797587143,6.70062138560767));
#22287=CARTESIAN_POINT('Ctrl Pts',(11.1051851219337,-42.0588133989565,7.2178432770462));
#22288=CARTESIAN_POINT('Ctrl Pts',(11.3709120573992,-41.9877513997447,8.28373602794641));
#22289=CARTESIAN_POINT('Ctrl Pts',(11.4940135235903,-41.9541547454922,8.81321169230964));
#22290=CARTESIAN_POINT('Ctrl Pts',(11.605772574847,-41.9232160376674,9.34999999998854));
#22291=CARTESIAN_POINT('Origin',(-1.73472347597681E-15,-1.73472347597681E-15,
11.35));
#22292=CARTESIAN_POINT('Ctrl Pts',(14.4035578208426,-41.0461633054985,9.34999999998854));
#22293=CARTESIAN_POINT('Ctrl Pts',(14.4599491076221,-41.0263749722096,8.8161349220257));
#22294=CARTESIAN_POINT('Ctrl Pts',(14.5221093054489,-41.0044304289847,8.29345816614813));
#22295=CARTESIAN_POINT('Ctrl Pts',(14.6553380062866,-40.9570029893927,7.21621981188605));
#22296=CARTESIAN_POINT('Ctrl Pts',(14.7232050398853,-40.9326504745967,6.68773441334895));
#22297=CARTESIAN_POINT('Ctrl Pts',(14.7872765596602,-40.9094909763997,6.16441400296897));
#22298=CARTESIAN_POINT('Ctrl Pts',(16.7073411592906,-40.1635998310296,6.16441400296896));
#22299=CARTESIAN_POINT('Ctrl Pts',(16.846578226198,-40.1056796946716,6.70062138560762));
#22300=CARTESIAN_POINT('Ctrl Pts',(16.9777435765859,-40.0502826977333,7.21784327704622));
#22301=CARTESIAN_POINT('Ctrl Pts',(17.2306526180698,-39.9421271213649,8.28373602794653));
#22302=CARTESIAN_POINT('Ctrl Pts',(17.3477197864163,-39.8913532673581,8.81321169230968));
#22303=CARTESIAN_POINT('Ctrl Pts',(17.4539382544739,-39.8448244996639,9.34999999998855));
#22304=CARTESIAN_POINT('Origin',(-1.73472347597681E-15,-1.73472347597681E-15,
11.35));
#22305=CARTESIAN_POINT('Ctrl Pts',(20.0984284630027,-38.5785325448956,9.34999999998854));
#22306=CARTESIAN_POINT('Ctrl Pts',(20.1514295943406,-38.5509203114491,8.81613492202573));
#22307=CARTESIAN_POINT('Ctrl Pts',(20.2098340568611,-38.5203528135321,8.2934581661483));
#22308=CARTESIAN_POINT('Ctrl Pts',(20.3349570532291,-38.4544476958773,7.21621981188512));
#22309=CARTESIAN_POINT('Ctrl Pts',(20.398667574077,-38.4206845686579,6.68773441334953));
#22310=CARTESIAN_POINT('Ctrl Pts',(20.4587909979238,-38.3886424727845,6.16441400296896));
#22311=CARTESIAN_POINT('Ctrl Pts',(22.2531607307116,-37.3770897408174,6.16441400296897));
#22312=CARTESIAN_POINT('Ctrl Pts',(22.3827376702025,-37.2999436472751,6.70062138560737));
#22313=CARTESIAN_POINT('Ctrl Pts',(22.5046841317882,-37.2264437362622,7.21784327704616));
#22314=CARTESIAN_POINT('Ctrl Pts',(22.7396267805353,-37.0833963183772,8.28373602794666));
#22315=CARTESIAN_POINT('Ctrl Pts',(22.8482765010835,-37.016478873864,8.81321169230972));
#22316=CARTESIAN_POINT('Ctrl Pts',(22.9467920842412,-36.9553072378327,9.34999999998855));
#22317=CARTESIAN_POINT('Origin',(-1.73472347597681E-15,-1.73472347597681E-15,
11.35));
#22318=CARTESIAN_POINT('Ctrl Pts',(25.3841530607376,-35.3255541129796,9.34999999998854));
#22319=CARTESIAN_POINT('Ctrl Pts',(25.4326850864425,-35.2906800848214,8.81613492202558));
#22320=CARTESIAN_POINT('Ctrl Pts',(25.4861448672244,-35.2521118983204,8.2934581661475));
#22321=CARTESIAN_POINT('Ctrl Pts',(25.6006150157412,-35.1690707407437,7.21621981188588));
#22322=CARTESIAN_POINT('Ctrl Pts',(25.6588720613602,-35.1265843210061,6.68773441334898));
#22323=CARTESIAN_POINT('Ctrl Pts',(25.7138234497508,-35.0863119121267,6.16441400296896));
#22324=CARTESIAN_POINT('Ctrl Pts',(27.3459701224716,-33.8296898901083,6.16441400296896));
#22325=CARTESIAN_POINT('Ctrl Pts',(27.4632491217272,-33.7348883113751,6.70062138560758));
#22326=CARTESIAN_POINT('Ctrl Pts',(27.5734942162173,-33.6447817325196,7.21784327704617));
#22327=CARTESIAN_POINT('Ctrl Pts',(27.7856877174178,-33.4697545060314,8.28373602794671));
#22328=CARTESIAN_POINT('Ctrl Pts',(27.8837081951772,-33.3880557172081,8.81321169230973));
#22329=CARTESIAN_POINT('Ctrl Pts',(27.9725154002573,-33.3134864909449,9.34999999998854));
#22330=CARTESIAN_POINT('Origin',(-1.73472347597681E-15,-1.73472347597681E-15,
11.35));
#22331=CARTESIAN_POINT('Ctrl Pts',(30.1531295040085,-31.3534492698092,9.34999999998854));
#22332=CARTESIAN_POINT('Ctrl Pts',(30.1962044519918,-31.3120233815841,8.81613492202547));
#22333=CARTESIAN_POINT('Ctrl Pts',(30.2436312640637,-31.2662396435548,8.29345816614697));
#22334=CARTESIAN_POINT('Ctrl Pts',(30.3451186039616,-31.1677526127026,7.21621640088951));
#22335=CARTESIAN_POINT('Ctrl Pts',(30.3967356067597,-31.11740840803,6.68773764820084));
#22336=CARTESIAN_POINT('Ctrl Pts',(30.4453966086845,-31.0697252215063,6.16441400296896));
#22337=CARTESIAN_POINT('Ctrl Pts',(31.8820944218039,-29.5936151100062,6.16441400296896));
#22338=CARTESIAN_POINT('Ctrl Pts',(31.9846880186039,-29.48308793284,6.70062138560735));
#22339=CARTESIAN_POINT('Ctrl Pts',(32.0809874737953,-29.3782089962415,7.21784327704616));
#22340=CARTESIAN_POINT('Ctrl Pts',(32.2661121796801,-29.1747650107446,8.28373602794627));
#22341=CARTESIAN_POINT('Ctrl Pts',(32.3515080003913,-29.0799480293518,8.81321169230959));
#22342=CARTESIAN_POINT('Ctrl Pts',(32.4287989687974,-28.9934992272635,9.34999999998855));
#22343=CARTESIAN_POINT('Origin',(-1.73472347597681E-15,-1.73472347597681E-15,
11.35));
#22344=CARTESIAN_POINT('Ctrl Pts',(37.7650033201655,-21.5882960010254,9.34999999998854));
#22345=CARTESIAN_POINT('Ctrl Pts',(37.7946624086853,-21.5364125371166,8.81613492202549));
#22346=CARTESIAN_POINT('Ctrl Pts',(37.8272693320525,-21.4791216851438,8.29345816614708));
#22347=CARTESIAN_POINT('Ctrl Pts',(37.8968987185776,-21.3560317832924,7.21621640088866));
#22348=CARTESIAN_POINT('Ctrl Pts',(37.9322412685768,-21.2931846824721,6.68773764820146));
#22349=CARTESIAN_POINT('Ctrl Pts',(37.9654972519551,-21.2337236115523,6.16441400296896));
#22350=CARTESIAN_POINT('Ctrl Pts',(38.928130432958,-19.412641782988,6.16441400296896));
#22351=CARTESIAN_POINT('Ctrl Pts',(38.995429164002,-19.2776877767616,6.70062138560751));
#22352=CARTESIAN_POINT('Ctrl Pts',(39.0582800036543,-19.1499264822817,7.2178432770462));
#22353=CARTESIAN_POINT('Ctrl Pts',(39.1785890639852,-18.9025677509498,8.28373602794626));
#22354=CARTESIAN_POINT('Ctrl Pts',(39.2338127233339,-18.7875327406115,8.81321169230958));
#22355=CARTESIAN_POINT('Ctrl Pts',(39.2836174223951,-18.6828103402806,9.34999999998855));
#22356=CARTESIAN_POINT('Origin',(-1.73472347597681E-15,-1.73472347597681E-15,
11.35));
#22357=CARTESIAN_POINT('Ctrl Pts',(34.3082751850227,-26.7430786153868,9.34999999998854));
#22358=CARTESIAN_POINT('Ctrl Pts',(34.3450161735614,-26.6959441787169,8.81613492202567));
#22359=CARTESIAN_POINT('Ctrl Pts',(34.385444543797,-26.6438769140362,8.29345816614794));
#22360=CARTESIAN_POINT('Ctrl Pts',(34.4718824493404,-26.5319495391969,7.21621981188585));
#22361=CARTESIAN_POINT('Ctrl Pts',(34.5158098676116,-26.4747712115684,6.68773441334903));
#22362=CARTESIAN_POINT('Ctrl Pts',(34.557189289939,-26.4206485230648,6.16441400296897));
#22363=CARTESIAN_POINT('Ctrl Pts',(35.7691912190764,-24.755099667203,6.16441400296895));
#22364=CARTESIAN_POINT('Ctrl Pts',(35.8550109036455,-24.631096906197,6.70062138560717));
#22365=CARTESIAN_POINT('Ctrl Pts',(35.9354043403351,-24.5135806445587,7.21784327704611));
#22366=CARTESIAN_POINT('Ctrl Pts',(36.0896916457482,-24.2858614329137,8.28373602794642));
#22367=CARTESIAN_POINT('Ctrl Pts',(36.1607243967626,-24.1798564592629,8.81321169230963));
#22368=CARTESIAN_POINT('Ctrl Pts',(36.2249257072666,-24.0832879296623,9.34999999998854));
#22369=CARTESIAN_POINT('Origin',(-1.73472347597681E-15,-1.73472347597681E-15,
11.35));
#22370=CARTESIAN_POINT('Ctrl Pts',(40.4529448929862,-15.9940379355879,9.34999999998854));
#22371=CARTESIAN_POINT('Ctrl Pts',(40.4749183079745,-15.9384616421459,8.81613492202553));
#22372=CARTESIAN_POINT('Ctrl Pts',(40.499040001544,-15.877113479414,8.29345816614729));
#22373=CARTESIAN_POINT('Ctrl Pts',(40.5504429790727,-15.7453675775639,7.21621981188599));
#22374=CARTESIAN_POINT('Ctrl Pts',(40.5764820318144,-15.6781295900963,6.68773441334888));
#22375=CARTESIAN_POINT('Ctrl Pts',(40.6009371733745,-15.6145413203111,6.16441400296896));
#22376=CARTESIAN_POINT('Ctrl Pts',(41.2946051706827,-13.6749984935074,6.16441400296896));
#22377=CARTESIAN_POINT('Ctrl Pts',(41.3420129401109,-13.5318405164523,6.70062138560745));
#22378=CARTESIAN_POINT('Ctrl Pts',(41.3860417208775,-13.3964350406532,7.2178432770462));
#22379=CARTESIAN_POINT('Ctrl Pts',(41.4699233906006,-13.1344723000805,8.28373602794641));
#22380=CARTESIAN_POINT('Ctrl Pts',(41.508213763831,-13.0127490341317,8.81321169230963));
#22381=CARTESIAN_POINT('Ctrl Pts',(41.5426079714016,-12.9020046091468,9.34999999998855));
#22382=CARTESIAN_POINT('Origin',(-1.73472347597681E-15,-1.73472347597681E-15,
11.35));
#22383=CARTESIAN_POINT('Ctrl Pts',(42.3173811644455,-10.0741873807785,9.34999999998854));
#22384=CARTESIAN_POINT('Ctrl Pts',(42.3312215905392,-10.016049630869,8.81613492202556));
#22385=CARTESIAN_POINT('Ctrl Pts',(42.3463670061913,-9.95189302905774,8.29345816614737));
#22386=CARTESIAN_POINT('Ctrl Pts',(42.3784973788108,-9.81417270409282,7.21621981188622));
#22387=CARTESIAN_POINT('Ctrl Pts',(42.3947024282284,-9.74391335880868,6.68773441334868));
#22388=CARTESIAN_POINT('Ctrl Pts',(42.4098590973783,-9.67749199640711,6.16441400296896));
#22389=CARTESIAN_POINT('Ctrl Pts',(42.8204408309399,-7.65897167013824,6.16441400296896));
#22390=CARTESIAN_POINT('Ctrl Pts',(42.8469925532796,-7.51052400583368,6.70062138560742));
#22391=CARTESIAN_POINT('Ctrl Pts',(42.8713029761526,-7.37023081372545,7.21784327704618));
#22392=CARTESIAN_POINT('Ctrl Pts',(42.917049666367,-7.09899686987205,8.2837360279463));
#22393=CARTESIAN_POINT('Ctrl Pts',(42.9376272719005,-6.97306328298636,8.8132116923096));
#22394=CARTESIAN_POINT('Ctrl Pts',(42.955910821099,-6.85855127047957,9.34999999998855));
#22395=CARTESIAN_POINT('Origin',(-1.73472347597681E-15,-1.73472347597681E-15,
11.35));
#22396=CARTESIAN_POINT('Ctrl Pts',(43.3203575886467,-3.94925542245386,9.34999999998855));
#22397=CARTESIAN_POINT('Ctrl Pts',(43.3257832746831,-3.88973973300951,8.81613492202556));
#22398=CARTESIAN_POINT('Ctrl Pts',(43.3316440954308,-3.82408073551946,8.29345816614743));
#22399=CARTESIAN_POINT('Ctrl Pts',(43.3438477814109,-3.68318957610333,7.21621981188594));
#22400=CARTESIAN_POINT('Ctrl Pts',(43.3498889394299,-3.61133915066155,6.6877344133489));
#22401=CARTESIAN_POINT('Ctrl Pts',(43.3554385900939,-3.54343684303868,6.16441400296896));
#22402=CARTESIAN_POINT('Ctrl Pts',(43.4745757998335,-1.48703027021543,6.16441400296896));
#22403=CARTESIAN_POINT('Ctrl Pts',(43.4797309585866,-1.33631488501896,6.70062138560747));
#22404=CARTESIAN_POINT('Ctrl Pts',(43.4838281334618,-1.19398994142081,7.21784327704619));
#22405=CARTESIAN_POINT('Ctrl Pts',(43.4905085734774,-0.919006335209355,
8.28373602794638));
#22406=CARTESIAN_POINT('Ctrl Pts',(43.4929545106062,-0.791426072053404,
8.81321169230962));
#22407=CARTESIAN_POINT('Ctrl Pts',(43.4947552010963,-0.675477606374008,
9.34999999998855));
#22408=CARTESIAN_POINT('Origin',(-1.73472347597681E-15,-1.73472347597681E-15,
11.35));
#22409=CARTESIAN_POINT('Ctrl Pts',(43.4414565156357,2.25607087657594,9.35000993791518));
#22410=CARTESIAN_POINT('Ctrl Pts',(43.4383570102934,2.31575293774707,8.81614485995222));
#22411=CARTESIAN_POINT('Ctrl Pts',(43.4348138690301,2.38157881405584,8.29345816614752));
#22412=CARTESIAN_POINT('Ctrl Pts',(43.4268424365168,2.52277267021401,7.21621981188581));
#22413=CARTESIAN_POINT('Ctrl Pts',(43.4225967225812,2.59475150835097,6.6877344133491));
#22414=CARTESIAN_POINT('Ctrl Pts',(43.4184263798756,2.66275246602603,6.16441400296896));
#22415=CARTESIAN_POINT('Ctrl Pts',(43.2436937757663,4.71518277776774,6.16441400296896));
#22416=CARTESIAN_POINT('Ctrl Pts',(43.2273474267669,4.86509775324073,6.70062138560733));
#22417=CARTESIAN_POINT('Ctrl Pts',(43.211147946979,5.00655712290845,7.21784327704615));
#22418=CARTESIAN_POINT('Ctrl Pts',(43.1786261423019,5.2796925182427,8.28373602794632));
#22419=CARTESIAN_POINT('Ctrl Pts',(43.1628906187996,5.40632229142219,8.8132116923096));
#22420=CARTESIAN_POINT('Ctrl Pts',(43.1481717937157,5.52134683388074,9.34999999998855));
#22421=CARTESIAN_POINT('Origin',(-1.73472347597681E-15,-1.73472347597681E-15,
11.35));
#22422=CARTESIAN_POINT('Ctrl Pts',(42.6782125485618,8.41547227788107,9.34999999998855));
#22423=CARTESIAN_POINT('Ctrl Pts',(42.6666509488314,8.47410575612239,8.81613492202559));
#22424=CARTESIAN_POINT('Ctrl Pts',(42.6537760879159,8.53875628688309,8.29345816614751));
#22425=CARTESIAN_POINT('Ctrl Pts',(42.6257917236771,8.67737897897861,7.21621640088911));
#22426=CARTESIAN_POINT('Ctrl Pts',(42.6113457422261,8.74802009690499,6.68773764820129));
#22427=CARTESIAN_POINT('Ctrl Pts',(42.5975402169653,8.81473581362641,6.16441400296896));
#22428=CARTESIAN_POINT('Ctrl Pts',(42.1324948509395,10.8214083018598,6.16441400296896));
#22429=CARTESIAN_POINT('Ctrl Pts',(42.0949797587143,10.9674710310278,6.7006213856072));
#22430=CARTESIAN_POINT('Ctrl Pts',(42.0588133989564,11.1051851219338,7.2178432770461));
#22431=CARTESIAN_POINT('Ctrl Pts',(41.9877513997447,11.3709120573994,8.2837360279465));
#22432=CARTESIAN_POINT('Ctrl Pts',(41.9541547454921,11.4940135235905,8.81321169230966));
#22433=CARTESIAN_POINT('Ctrl Pts',(41.9232160376674,11.6057725748471,9.34999999998855));
#22434=CARTESIAN_POINT('Origin',(-1.73472347597681E-15,-1.73472347597681E-15,
11.35));
#22435=CARTESIAN_POINT('Ctrl Pts',(41.0461633054984,14.4035578208427,9.34999999998854));
#22436=CARTESIAN_POINT('Ctrl Pts',(41.0263749722095,14.4599491076222,8.8161349220256));
#22437=CARTESIAN_POINT('Ctrl Pts',(41.0044304289846,14.5221093054492,8.29345816614753));
#22438=CARTESIAN_POINT('Ctrl Pts',(40.9570029893926,14.6553380062868,7.2162198118858));
#22439=CARTESIAN_POINT('Ctrl Pts',(40.9326504745967,14.7232050398854,6.6877344133491));
#22440=CARTESIAN_POINT('Ctrl Pts',(40.9094909763996,14.7872765596604,6.16441400296896));
#22441=CARTESIAN_POINT('Ctrl Pts',(40.1635998310295,16.7073411592907,6.16441400296896));
#22442=CARTESIAN_POINT('Ctrl Pts',(40.1056796946715,16.8465782261981,6.70062138560777));
#22443=CARTESIAN_POINT('Ctrl Pts',(40.0502826977332,16.977743576586,7.2178432770462));
#22444=CARTESIAN_POINT('Ctrl Pts',(39.9421271213649,17.2306526180698,8.2837360279462));
#22445=CARTESIAN_POINT('Ctrl Pts',(39.8913532673581,17.3477197864164,8.81321169230956));
#22446=CARTESIAN_POINT('Ctrl Pts',(39.8448244996638,17.453938254474,9.34999999998855));
#22447=CARTESIAN_POINT('Origin',(-1.73472347597681E-15,-1.73472347597681E-15,
11.35));
#22448=CARTESIAN_POINT('Ctrl Pts',(38.5785325448955,20.0984284630028,9.34999999998854));
#22449=CARTESIAN_POINT('Ctrl Pts',(38.550920311449,20.1514295943407,8.81613492202552));
#22450=CARTESIAN_POINT('Ctrl Pts',(38.5203528135319,20.2098340568614,8.29345816614715));
#22451=CARTESIAN_POINT('Ctrl Pts',(38.4544476958772,20.3349570532291,7.21621981188606));
#22452=CARTESIAN_POINT('Ctrl Pts',(38.4206845686578,20.3986675740772,6.68773441334892));
#22453=CARTESIAN_POINT('Ctrl Pts',(38.3886424727845,20.4587909979239,6.16441400296896));
#22454=CARTESIAN_POINT('Ctrl Pts',(37.3770911258214,22.2531584044164,6.16440437643718));
#22455=CARTESIAN_POINT('Ctrl Pts',(37.2999450322789,22.3827353439075,6.70061175907635));
#22456=CARTESIAN_POINT('Ctrl Pts',(37.2264437362621,22.5046841317884,7.21784327704632));
#22457=CARTESIAN_POINT('Ctrl Pts',(37.0833963183771,22.7396267805354,8.28373602794611));
#22458=CARTESIAN_POINT('Ctrl Pts',(37.0164788738639,22.8482765010836,8.81321169230953));
#22459=CARTESIAN_POINT('Ctrl Pts',(36.9553072378326,22.9467920842413,9.34999999998855));
#22460=CARTESIAN_POINT('Origin',(-1.73472347597681E-15,-1.73472347597681E-15,
11.35));
#22461=CARTESIAN_POINT('Ctrl Pts',(35.3255541129795,25.3841530607377,9.34999999998854));
#22462=CARTESIAN_POINT('Ctrl Pts',(35.2906800848213,25.4326850864426,8.8161349220256));
#22463=CARTESIAN_POINT('Ctrl Pts',(35.2521118983203,25.4861448672246,8.29345816614758));
#22464=CARTESIAN_POINT('Ctrl Pts',(35.1690707407436,25.6006150157413,7.21621981188613));
#22465=CARTESIAN_POINT('Ctrl Pts',(35.126584321006,25.6588720613604,6.6877344133489));
#22466=CARTESIAN_POINT('Ctrl Pts',(35.0863119121266,25.713823449751,6.16441400296896));
#22467=CARTESIAN_POINT('Ctrl Pts',(33.8296898901082,27.3459701224717,6.16441400296896));
#22468=CARTESIAN_POINT('Ctrl Pts',(33.7348883113749,27.4632491217274,6.70062138560785));
#22469=CARTESIAN_POINT('Ctrl Pts',(33.6447817325195,27.5734942162174,7.21784327704626));
#22470=CARTESIAN_POINT('Ctrl Pts',(33.4697545060313,27.7856877174178,8.28373602794632));
#22471=CARTESIAN_POINT('Ctrl Pts',(33.388055717208,27.8837081951773,8.81321169230959));
#22472=CARTESIAN_POINT('Ctrl Pts',(33.3134864909448,27.9725154002575,9.34999999998854));
#22473=CARTESIAN_POINT('Origin',(-1.73472347597681E-15,-1.73472347597681E-15,
11.35));
#22474=CARTESIAN_POINT('Ctrl Pts',(31.3534492698091,30.1531295040086,9.34999999998854));
#22475=CARTESIAN_POINT('Ctrl Pts',(31.312023381584,30.1962044519919,8.81613492202545));
#22476=CARTESIAN_POINT('Ctrl Pts',(31.2662396435547,30.2436312640639,8.29345816614677));
#22477=CARTESIAN_POINT('Ctrl Pts',(31.1677529245535,30.3451182826104,7.21621981188611));
#22478=CARTESIAN_POINT('Ctrl Pts',(31.1174081132829,30.396735907551,6.68773441334884));
#22479=CARTESIAN_POINT('Ctrl Pts',(31.0697252215062,30.4453966086846,6.16441400296896));
#22480=CARTESIAN_POINT('Ctrl Pts',(29.593615110006,31.882094421804,6.16441400296896));
#22481=CARTESIAN_POINT('Ctrl Pts',(29.4830879328398,31.9846880186041,6.70062138560775));
#22482=CARTESIAN_POINT('Ctrl Pts',(29.3782089962414,32.0809874737954,7.21784327704626));
#22483=CARTESIAN_POINT('Ctrl Pts',(29.1747650107445,32.2661121796802,8.28373602794619));
#22484=CARTESIAN_POINT('Ctrl Pts',(29.0799480293516,32.3515080003914,8.81321169230955));
#22485=CARTESIAN_POINT('Ctrl Pts',(28.9934992272633,32.4287989687975,9.34999999998855));
#22486=CARTESIAN_POINT('Origin',(-1.73472347597681E-15,-1.73472347597681E-15,
11.35));
#22487=CARTESIAN_POINT('Ctrl Pts',(26.7430786153867,34.3082751850228,9.34999999998854));
#22488=CARTESIAN_POINT('Ctrl Pts',(26.6959441787167,34.3450161735616,8.81613492202541));
#22489=CARTESIAN_POINT('Ctrl Pts',(26.6438769140359,34.3854445437972,8.29345816614648));
#22490=CARTESIAN_POINT('Ctrl Pts',(26.5319495391968,34.4718824493405,7.21621981188615));
#22491=CARTESIAN_POINT('Ctrl Pts',(26.4747712115682,34.5158098676118,6.68773441334885));
#22492=CARTESIAN_POINT('Ctrl Pts',(26.4206485230647,34.5571892899391,6.16441400296896));
#22493=CARTESIAN_POINT('Ctrl Pts',(24.7550996672029,35.7691912190764,6.16441400296896));
#22494=CARTESIAN_POINT('Ctrl Pts',(24.6310969061966,35.8550109036457,6.70062138560821));
#22495=CARTESIAN_POINT('Ctrl Pts',(24.5135806445585,35.9354043403352,7.21784327704631));
#22496=CARTESIAN_POINT('Ctrl Pts',(24.2858614329136,36.0896916457482,8.28373602794605));
#22497=CARTESIAN_POINT('Ctrl Pts',(24.1798564592628,36.1607243967627,8.81321169230951));
#22498=CARTESIAN_POINT('Ctrl Pts',(24.0832879296622,36.2249257072667,9.34999999998855));
#22499=CARTESIAN_POINT('Origin',(-1.73472347597681E-15,-1.73472347597681E-15,
11.35));
#22500=CARTESIAN_POINT('Ctrl Pts',(21.5882960010253,37.7650033201656,9.34999999998854));
#22501=CARTESIAN_POINT('Ctrl Pts',(21.5364125371165,37.7946624086854,8.81613492202566));
#22502=CARTESIAN_POINT('Ctrl Pts',(21.4791216851438,37.8272693320525,8.29345816614794));
#22503=CARTESIAN_POINT('Ctrl Pts',(21.3560321730463,37.896898498102,7.21621981188577));
#22504=CARTESIAN_POINT('Ctrl Pts',(21.2931843149217,37.9322414741441,6.6877344133491));
#22505=CARTESIAN_POINT('Ctrl Pts',(21.2337236115522,37.9654972519551,6.16441400296897));
#22506=CARTESIAN_POINT('Ctrl Pts',(19.4126417829879,38.9281304329581,6.16441400296896));
#22507=CARTESIAN_POINT('Ctrl Pts',(19.2776877767614,38.9954291640021,6.70062138560747));
#22508=CARTESIAN_POINT('Ctrl Pts',(19.1499264822816,39.0582800036544,7.21784327704618));
#22509=CARTESIAN_POINT('Ctrl Pts',(18.9025677509496,39.1785890639853,8.28373602794654));
#22510=CARTESIAN_POINT('Ctrl Pts',(18.7875327406113,39.2338127233339,8.81321169230967));
#22511=CARTESIAN_POINT('Ctrl Pts',(18.6828103402805,39.2836174223952,9.34999999998855));
#22512=CARTESIAN_POINT('Origin',(-1.73472347597681E-15,-1.73472347597681E-15,
11.35));
#22513=CARTESIAN_POINT('Ctrl Pts',(15.9940379355878,40.4529448929863,9.34999999998854));
#22514=CARTESIAN_POINT('Ctrl Pts',(15.9384616421457,40.4749183079745,8.81613492202557));
#22515=CARTESIAN_POINT('Ctrl Pts',(15.8771134794139,40.4990400015441,8.29345816614744));
#22516=CARTESIAN_POINT('Ctrl Pts',(15.7453671603999,40.5504431418366,7.2162164008887));
#22517=CARTESIAN_POINT('Ctrl Pts',(15.6781299831607,40.5764818806474,6.68773764820152));
#22518=CARTESIAN_POINT('Ctrl Pts',(15.6145413203109,40.6009371733745,6.16441400296895));
#22519=CARTESIAN_POINT('Ctrl Pts',(13.6749984935073,41.2946051706827,6.16441400296896));
#22520=CARTESIAN_POINT('Ctrl Pts',(13.5318405164522,41.342012940111,6.70062138560718));
#22521=CARTESIAN_POINT('Ctrl Pts',(13.396435040653,41.3860417208776,7.21784327704614));
#22522=CARTESIAN_POINT('Ctrl Pts',(13.1344723000804,41.4699233906007,8.28373602794635));
#22523=CARTESIAN_POINT('Ctrl Pts',(13.0127490341315,41.508213763831,8.81321169230961));
#22524=CARTESIAN_POINT('Ctrl Pts',(12.9020046091466,41.5426079714016,9.34999999998854));
#22525=CARTESIAN_POINT('Origin',(-1.73472347597681E-15,-1.73472347597681E-15,
11.35));
#22526=CARTESIAN_POINT('Ctrl Pts',(10.0741873807783,42.3173811644455,9.34999999998854));
#22527=CARTESIAN_POINT('Ctrl Pts',(10.0160496308688,42.3312215905392,8.81613492202556));
#22528=CARTESIAN_POINT('Ctrl Pts',(9.95189302905758,42.3463670061913,8.2934581661474));
#22529=CARTESIAN_POINT('Ctrl Pts',(9.81417270409262,42.3784973788108,7.21621981188586));
#22530=CARTESIAN_POINT('Ctrl Pts',(9.74391335880857,42.3947024282284,6.68773441334904));
#22531=CARTESIAN_POINT('Ctrl Pts',(9.67749199640696,42.4098590973783,6.16441400296896));
#22532=CARTESIAN_POINT('Ctrl Pts',(7.65897167013808,42.8204408309399,6.16441400296896));
#22533=CARTESIAN_POINT('Ctrl Pts',(7.51052400583346,42.8469925532796,6.70062138560763));
#22534=CARTESIAN_POINT('Ctrl Pts',(7.37023081372529,42.8713029761526,7.2178432770462));
#22535=CARTESIAN_POINT('Ctrl Pts',(7.09899686987191,42.9170496663671,8.28373602794623));
#22536=CARTESIAN_POINT('Ctrl Pts',(6.97306328298622,42.9376272719005,8.81321169230957));
#22537=CARTESIAN_POINT('Ctrl Pts',(6.85855127047942,42.955910821099,9.34999999998854));
#22538=CARTESIAN_POINT('Origin',(-1.73472347597681E-15,-1.73472347597681E-15,
11.35));
#22539=CARTESIAN_POINT('Ctrl Pts',(3.9492554224537,43.3203575886467,9.34999999998854));
#22540=CARTESIAN_POINT('Ctrl Pts',(3.88973973300936,43.3257832746831,8.81613492202564));
#22541=CARTESIAN_POINT('Ctrl Pts',(3.82408073551934,43.3316440954308,8.29345816614775));
#22542=CARTESIAN_POINT('Ctrl Pts',(3.68318912998151,43.343847820053,7.21621640088861));
#22543=CARTESIAN_POINT('Ctrl Pts',(3.6113395703927,43.3498889051253,6.68773764820155));
#22544=CARTESIAN_POINT('Ctrl Pts',(3.54343684303852,43.3554385900939,6.16441400296896));
#22545=CARTESIAN_POINT('Ctrl Pts',(1.48703027021497,43.4745757998335,6.16441400296896));
#22546=CARTESIAN_POINT('Ctrl Pts',(1.33631488501848,43.4797309585866,6.70062138560754));
#22547=CARTESIAN_POINT('Ctrl Pts',(1.19398994142034,43.4838281334618,7.21784327704621));
#22548=CARTESIAN_POINT('Ctrl Pts',(0.9190063352089,43.4905085734774,8.28373602794634));
#22549=CARTESIAN_POINT('Ctrl Pts',(0.791426072052943,43.4929545106062,8.8132116923096));
#22550=CARTESIAN_POINT('Ctrl Pts',(0.675477606373541,43.4947552010963,9.34999999998854));
#22551=CARTESIAN_POINT('Origin',(-1.73472347597681E-15,-1.73472347597681E-15,
11.35));
#22552=CARTESIAN_POINT('Ctrl Pts',(-2.25607087657641,43.4414565156357,9.35000993791518));
#22553=CARTESIAN_POINT('Ctrl Pts',(-2.31575293774753,43.4383570102934,8.81614485995224));
#22554=CARTESIAN_POINT('Ctrl Pts',(-2.38157881405629,43.4348138690301,8.29345816614757));
#22555=CARTESIAN_POINT('Ctrl Pts',(-2.52277267021449,43.4268424365167,7.21621981188565));
#22556=CARTESIAN_POINT('Ctrl Pts',(-2.59475150835141,43.4225967225811,6.68773441334928));
#22557=CARTESIAN_POINT('Ctrl Pts',(-2.66275246602649,43.4184263798755,6.16441400296896));
#22558=CARTESIAN_POINT('Ctrl Pts',(-4.7151827777679,43.2436937757662,6.16441400296896));
#22559=CARTESIAN_POINT('Ctrl Pts',(-4.86509775324099,43.2273474267669,6.70062138560767));
#22560=CARTESIAN_POINT('Ctrl Pts',(-5.00655712290862,43.211147946979,7.21784327704619));
#22561=CARTESIAN_POINT('Ctrl Pts',(-5.27969251824286,43.1786261423019,8.28373602794632));
#22562=CARTESIAN_POINT('Ctrl Pts',(-5.40632229142235,43.1628906187995,8.8132116923096));
#22563=CARTESIAN_POINT('Ctrl Pts',(-5.5213468338809,43.1481717937156,9.34999999998855));
#22564=CARTESIAN_POINT('Origin',(-1.73472347597681E-15,-1.73472347597681E-15,
11.35));
#22565=CARTESIAN_POINT('Ctrl Pts',(-8.41547227788122,42.6782125485618,9.34999999998854));
#22566=CARTESIAN_POINT('Ctrl Pts',(-8.47410575612254,42.6666509488314,8.8161349220256));
#22567=CARTESIAN_POINT('Ctrl Pts',(-8.53875628688322,42.6537760879159,8.29345816614766));
#22568=CARTESIAN_POINT('Ctrl Pts',(-8.67737854004153,42.6257918122873,7.21621981188561));
#22569=CARTESIAN_POINT('Ctrl Pts',(-8.74802050929902,42.6113456568892,6.68773441334929));
#22570=CARTESIAN_POINT('Ctrl Pts',(-8.81473581362657,42.5975402169653,6.16441400296896));
#22571=CARTESIAN_POINT('Ctrl Pts',(-10.82140830186,42.1324948509394,6.16441400296896));
#22572=CARTESIAN_POINT('Ctrl Pts',(-10.9674710310281,42.0949797587142,6.70062138560754));
#22573=CARTESIAN_POINT('Ctrl Pts',(-11.105185121934,42.0588133989564,7.21784327704616));
#22574=CARTESIAN_POINT('Ctrl Pts',(-11.3709120573995,41.9877513997446,8.28373602794637));
#22575=CARTESIAN_POINT('Ctrl Pts',(-11.4940135235907,41.9541547454921,8.81321169230963));
#22576=CARTESIAN_POINT('Ctrl Pts',(-11.6057725748473,41.9232160376673,9.34999999998855));
#22577=CARTESIAN_POINT('Origin',(-1.73472347597681E-15,-1.73472347597681E-15,
11.35));
#22578=CARTESIAN_POINT('Ctrl Pts',(-14.4035578208429,41.0461633054983,9.34999999998854));
#22579=CARTESIAN_POINT('Ctrl Pts',(-14.4599491076224,41.0263749722094,8.81613492202563));
#22580=CARTESIAN_POINT('Ctrl Pts',(-14.5221093054493,41.0044304289846,8.29345816614773));
#22581=CARTESIAN_POINT('Ctrl Pts',(-14.655338006287,40.9570029893926,7.2162198118857));
#22582=CARTESIAN_POINT('Ctrl Pts',(-14.7232050398856,40.9326504745966,6.68773441334913));
#22583=CARTESIAN_POINT('Ctrl Pts',(-14.7872765596605,40.9094909763996,6.16441400296896));
#22584=CARTESIAN_POINT('Ctrl Pts',(-16.7073411592909,40.1635998310295,6.16441400296896));
#22585=CARTESIAN_POINT('Ctrl Pts',(-16.8465782261982,40.1056796946715,6.70062138560753));
#22586=CARTESIAN_POINT('Ctrl Pts',(-16.9777435765862,40.0502826977332,7.21784327704622));
#22587=CARTESIAN_POINT('Ctrl Pts',(-17.23065261807,39.9421271213648,8.28373602794643));
#22588=CARTESIAN_POINT('Ctrl Pts',(-17.3477197864166,39.891353267358,8.81321169230964));
#22589=CARTESIAN_POINT('Ctrl Pts',(-17.4539382544742,39.8448244996638,9.34999999998855));
#22590=CARTESIAN_POINT('Origin',(-1.73472347597681E-15,-1.73472347597681E-15,
11.35));
#22591=CARTESIAN_POINT('Ctrl Pts',(-20.0984284630029,38.5785325448954,9.34999999998854));
#22592=CARTESIAN_POINT('Ctrl Pts',(-20.1514295943409,38.5509203114489,8.8161349220255));
#22593=CARTESIAN_POINT('Ctrl Pts',(-20.2098340568615,38.5203528135319,8.29345816614704));
#22594=CARTESIAN_POINT('Ctrl Pts',(-20.3349570532293,38.4544476958771,7.21621981188546));
#22595=CARTESIAN_POINT('Ctrl Pts',(-20.3986675740773,38.4206845686577,6.68773441334931));
#22596=CARTESIAN_POINT('Ctrl Pts',(-20.458790997924,38.3886424727844,6.16441400296896));
#22597=CARTESIAN_POINT('Ctrl Pts',(-22.2531607307118,37.3770897408173,6.16441400296896));
#22598=CARTESIAN_POINT('Ctrl Pts',(-22.3827376702031,37.2999436472748,6.70062138560852));
#22599=CARTESIAN_POINT('Ctrl Pts',(-22.5046841317886,37.226443736262,7.21784327704636));
#22600=CARTESIAN_POINT('Ctrl Pts',(-22.7396267805356,37.083396318377,8.28373602794636));
#22601=CARTESIAN_POINT('Ctrl Pts',(-22.8482765010838,37.0164788738638,8.81321169230961));
#22602=CARTESIAN_POINT('Ctrl Pts',(-22.9467920842415,36.9553072378325,9.34999999998855));
#22603=CARTESIAN_POINT('Origin',(-1.73472347597681E-15,-1.73472347597681E-15,
11.35));
#22604=CARTESIAN_POINT('Ctrl Pts',(-25.3841530607378,35.3255541129794,9.34999999998854));
#22605=CARTESIAN_POINT('Ctrl Pts',(-25.4326850864427,35.2906800848212,8.8161349220256));
#22606=CARTESIAN_POINT('Ctrl Pts',(-25.4861448672247,35.2521118983202,8.29345816614765));
#22607=CARTESIAN_POINT('Ctrl Pts',(-25.6006150157415,35.1690707407435,7.21621981188596));
#22608=CARTESIAN_POINT('Ctrl Pts',(-25.6588720613605,35.1265843210059,6.68773441334894));
#22609=CARTESIAN_POINT('Ctrl Pts',(-25.7138234497511,35.0863119121265,6.16441400296896));
#22610=CARTESIAN_POINT('Ctrl Pts',(-27.3459701224718,33.8296898901081,6.16441400296896));
#22611=CARTESIAN_POINT('Ctrl Pts',(-27.4632491217274,33.7348883113749,6.70062138560753));
#22612=CARTESIAN_POINT('Ctrl Pts',(-27.5734942162175,33.6447817325194,7.2178432770462));
#22613=CARTESIAN_POINT('Ctrl Pts',(-27.785687717418,33.4697545060312,8.28373602794646));
#22614=CARTESIAN_POINT('Ctrl Pts',(-27.8837081951774,33.3880557172079,8.81321169230965));
#22615=CARTESIAN_POINT('Ctrl Pts',(-27.9725154002576,33.3134864909447,9.34999999998855));
#22616=CARTESIAN_POINT('Origin',(-1.73472347597681E-15,-1.73472347597681E-15,
11.35));
#22617=CARTESIAN_POINT('Ctrl Pts',(-30.1531295040087,31.353449269809,9.34999999998854));
#22618=CARTESIAN_POINT('Ctrl Pts',(-30.196204451992,31.3120233815839,8.81613492202546));
#22619=CARTESIAN_POINT('Ctrl Pts',(-30.243631264064,31.2662396435546,8.29345816614692));
#22620=CARTESIAN_POINT('Ctrl Pts',(-30.3451182826105,31.1677529245534,7.21621981188656));
#22621=CARTESIAN_POINT('Ctrl Pts',(-30.3967359075512,31.1174081132828,6.68773441334847));
#22622=CARTESIAN_POINT('Ctrl Pts',(-30.4453966086847,31.0697252215061,6.16441400296896));
#22623=CARTESIAN_POINT('Ctrl Pts',(-31.8820944218041,29.5936151100059,6.16441400296896));
#22624=CARTESIAN_POINT('Ctrl Pts',(-31.9846880186042,29.4830879328396,6.70062138560796));
#22625=CARTESIAN_POINT('Ctrl Pts',(-32.0809874737955,29.3782089962413,7.21784327704624));
#22626=CARTESIAN_POINT('Ctrl Pts',(-32.2661121796803,29.1747650107444,8.2837360279461));
#22627=CARTESIAN_POINT('Ctrl Pts',(-32.3515080003915,29.0799480293515,8.81321169230952));
#22628=CARTESIAN_POINT('Ctrl Pts',(-32.4287989687976,28.9934992272632,9.34999999998854));
#22629=CARTESIAN_POINT('Origin',(-1.73472347597681E-15,-1.73472347597681E-15,
11.35));
#22630=CARTESIAN_POINT('Ctrl Pts',(-37.7650033201657,21.5882960010252,9.34999999998855));
#22631=CARTESIAN_POINT('Ctrl Pts',(-37.7946624086854,21.5364125371163,8.81613492202542));
#22632=CARTESIAN_POINT('Ctrl Pts',(-37.8272693320526,21.4791216851435,8.29345816614661));
#22633=CARTESIAN_POINT('Ctrl Pts',(-37.896898498102,21.3560321730462,7.21621981188615));
#22634=CARTESIAN_POINT('Ctrl Pts',(-37.9322414741442,21.2931843149215,6.68773441334878));
#22635=CARTESIAN_POINT('Ctrl Pts',(-37.9654972519552,21.2337236115521,6.16441400296896));
#22636=CARTESIAN_POINT('Ctrl Pts',(-38.9281304329582,19.4126417829877,6.16441400296896));
#22637=CARTESIAN_POINT('Ctrl Pts',(-38.9954291640021,19.2776877767614,6.70062138560718));
#22638=CARTESIAN_POINT('Ctrl Pts',(-39.0582800036545,19.1499264822814,7.21784327704614));
#22639=CARTESIAN_POINT('Ctrl Pts',(-39.1785890639854,18.9025677509495,8.28373602794646));
#22640=CARTESIAN_POINT('Ctrl Pts',(-39.233812723334,18.7875327406112,8.81321169230965));
#22641=CARTESIAN_POINT('Ctrl Pts',(-39.2836174223953,18.6828103402803,9.34999999998855));
#22642=CARTESIAN_POINT('Origin',(-1.73472347597681E-15,-1.73472347597681E-15,
11.35));
#22643=CARTESIAN_POINT('Ctrl Pts',(-34.3082751850229,26.7430786153866,9.34999999998854));
#22644=CARTESIAN_POINT('Ctrl Pts',(-34.3450161735616,26.6959441787166,8.81613492202578));
#22645=CARTESIAN_POINT('Ctrl Pts',(-34.3854445437971,26.643876914036,8.29345816614856));
#22646=CARTESIAN_POINT('Ctrl Pts',(-34.4718824493406,26.5319495391966,7.21621981188526));
#22647=CARTESIAN_POINT('Ctrl Pts',(-34.5158098676118,26.4747712115682,6.68773441334945));
#22648=CARTESIAN_POINT('Ctrl Pts',(-34.5571892899392,26.4206485230645,6.16441400296896));
#22649=CARTESIAN_POINT('Ctrl Pts',(-35.7691912190765,24.7550996672027,6.16441400296896));
#22650=CARTESIAN_POINT('Ctrl Pts',(-35.8550109036458,24.6310969061965,6.7006213856079));
#22651=CARTESIAN_POINT('Ctrl Pts',(-35.9354043403353,24.5135806445584,7.21784327704629));
#22652=CARTESIAN_POINT('Ctrl Pts',(-36.0896916457483,24.2858614329134,8.28373602794633));
#22653=CARTESIAN_POINT('Ctrl Pts',(-36.1607243967628,24.1798564592627,8.8132116923096));
#22654=CARTESIAN_POINT('Ctrl Pts',(-36.2249257072668,24.0832879296621,9.34999999998854));
#22655=CARTESIAN_POINT('Origin',(-1.73472347597681E-15,-1.73472347597681E-15,
11.35));
#22656=CARTESIAN_POINT('Ctrl Pts',(-40.4529448929863,15.9940379355876,9.34999999998855));
#22657=CARTESIAN_POINT('Ctrl Pts',(-40.4749183079746,15.9384616421456,8.8161349220257));
#22658=CARTESIAN_POINT('Ctrl Pts',(-40.4990400015441,15.8771134794139,8.29345816614812));
#22659=CARTESIAN_POINT('Ctrl Pts',(-40.5504429790729,15.7453675775636,7.2162198118858));
#22660=CARTESIAN_POINT('Ctrl Pts',(-40.5764820318145,15.678129590096,6.68773441334901));
#22661=CARTESIAN_POINT('Ctrl Pts',(-40.6009371733746,15.6145413203108,6.16441400296896));
#22662=CARTESIAN_POINT('Ctrl Pts',(-41.2946051706828,13.6749984935071,6.16441400296895));
#22663=CARTESIAN_POINT('Ctrl Pts',(-41.3420129401111,13.5318405164519,6.70062138560768));
#22664=CARTESIAN_POINT('Ctrl Pts',(-41.3860417208777,13.3964350406529,7.21784327704624));
#22665=CARTESIAN_POINT('Ctrl Pts',(-41.4699233906007,13.1344723000802,8.28373602794634));
#22666=CARTESIAN_POINT('Ctrl Pts',(-41.5082137638311,13.0127490341314,8.81321169230959));
#22667=CARTESIAN_POINT('Ctrl Pts',(-41.5426079714017,12.9020046091465,9.34999999998854));
#22668=CARTESIAN_POINT('Origin',(-1.73472347597681E-15,-1.73472347597681E-15,
11.35));
#22669=CARTESIAN_POINT('Ctrl Pts',(-42.3173809068055,10.0741884630147,9.35000993791518));
#22670=CARTESIAN_POINT('Ctrl Pts',(-42.3312213328992,10.0160507131051,8.81614485995214));
#22671=CARTESIAN_POINT('Ctrl Pts',(-42.3463670061913,9.95189302905741,8.29345816614713));
#22672=CARTESIAN_POINT('Ctrl Pts',(-42.3784973788108,9.81417270409247,7.2162198118858));
#22673=CARTESIAN_POINT('Ctrl Pts',(-42.3947024282285,9.74391335880843,6.68773441334909));
#22674=CARTESIAN_POINT('Ctrl Pts',(-42.4098590973783,9.67749199640681,6.16441400296896));
#22675=CARTESIAN_POINT('Ctrl Pts',(-42.8204408309399,7.65897167013792,6.16441400296896));
#22676=CARTESIAN_POINT('Ctrl Pts',(-42.8469925532797,7.51052400583325,6.7006213856078));
#22677=CARTESIAN_POINT('Ctrl Pts',(-42.8713029761526,7.37023081372511,7.21784327704623));
#22678=CARTESIAN_POINT('Ctrl Pts',(-42.9170496663671,7.09899686987174,8.28373602794625));
#22679=CARTESIAN_POINT('Ctrl Pts',(-42.9376272719005,6.97306328298604,8.81321169230957));
#22680=CARTESIAN_POINT('Ctrl Pts',(-42.955910821099,6.85855127047925,9.34999999998854));
#22681=CARTESIAN_POINT('Origin',(-1.73472347597681E-15,-1.73472347597681E-15,
11.35));
#22682=CARTESIAN_POINT('Ctrl Pts',(-43.3203574876474,3.94925653034038,9.35000993791518));
#22683=CARTESIAN_POINT('Ctrl Pts',(-43.3257831736837,3.88974084089603,8.81614485995219));
#22684=CARTESIAN_POINT('Ctrl Pts',(-43.3316440954308,3.82408073551913,8.29345816614738));
#22685=CARTESIAN_POINT('Ctrl Pts',(-43.343847820053,3.68318912998135,7.21621640088867));
#22686=CARTESIAN_POINT('Ctrl Pts',(-43.3498889051253,3.61133957039253,6.68773764820154));
#22687=CARTESIAN_POINT('Ctrl Pts',(-43.3554385900939,3.54343684303836,6.16441400296897));
#22688=CARTESIAN_POINT('Ctrl Pts',(-43.4745757998335,1.48703027021514,6.16441400296896));
#22689=CARTESIAN_POINT('Ctrl Pts',(-43.4797309585866,1.33631488501862,6.70062138560764));
#22690=CARTESIAN_POINT('Ctrl Pts',(-43.4838281334618,1.19398994142049,7.21784327704629));
#22691=CARTESIAN_POINT('Ctrl Pts',(-43.4905085734774,0.919006335208971,
8.28373602794674));
#22692=CARTESIAN_POINT('Ctrl Pts',(-43.4929545106062,0.79142607205295,8.81321169231029));
#22693=CARTESIAN_POINT('Ctrl Pts',(-43.4947552010963,0.675477606373505,
9.34999999998951));
#22694=CARTESIAN_POINT('Origin',(-1.73472347597681E-15,-1.73472347597681E-15,
11.35));
#22695=CARTESIAN_POINT('Ctrl Pts',(-43.4414564579383,-2.25607198755999,
9.3499999999895));
#22696=CARTESIAN_POINT('Ctrl Pts',(-43.438356952596,-2.31575404873114,8.81613492202627));
#22697=CARTESIAN_POINT('Ctrl Pts',(-43.4348138690301,-2.38157881405607,
8.29345816614802));
#22698=CARTESIAN_POINT('Ctrl Pts',(-43.4268424112758,-2.52277311729442,
7.21621640088862));
#22699=CARTESIAN_POINT('Ctrl Pts',(-43.4225967483597,-2.59475108801018,
6.68773764820165));
#22700=CARTESIAN_POINT('Ctrl Pts',(-43.4184263798756,-2.66275246602632,
6.16441400296896));
#22701=CARTESIAN_POINT('Ctrl Pts',(-43.2436937757662,-4.71518277776806,
6.16441400296896));
#22702=CARTESIAN_POINT('Ctrl Pts',(-43.2273474267669,-4.86509775324113,
6.70062138560761));
#22703=CARTESIAN_POINT('Ctrl Pts',(-43.211147946979,-5.00655712290883,7.21784327704638));
#22704=CARTESIAN_POINT('Ctrl Pts',(-43.1786261423019,-5.27969251824321,
8.2837360279471));
#22705=CARTESIAN_POINT('Ctrl Pts',(-43.1628906187995,-5.40632229142282,
8.81321169231093));
#22706=CARTESIAN_POINT('Ctrl Pts',(-43.1481717937156,-5.52134683388146,
9.34999999999046));
#22707=CARTESIAN_POINT('Origin',(-1.73472347597681E-15,-1.73472347597681E-15,
11.35));
#22708=CARTESIAN_POINT('Ctrl Pts',(-42.6782127637814,-8.41547118641672,
9.3500099379171));
#22709=CARTESIAN_POINT('Ctrl Pts',(-42.666651164051,-8.47410466465809,8.81614485995349));
#22710=CARTESIAN_POINT('Ctrl Pts',(-42.6537760879159,-8.53875628688335,
8.29345816614791));
#22711=CARTESIAN_POINT('Ctrl Pts',(-42.6257917236771,-8.6773789789789,7.2162164008893));
#22712=CARTESIAN_POINT('Ctrl Pts',(-42.6113457422261,-8.74802009690531,
6.68773764820119));
#22713=CARTESIAN_POINT('Ctrl Pts',(-42.5975402169652,-8.81473581362672,
6.16441400296896));
#22714=CARTESIAN_POINT('Ctrl Pts',(-42.1324948509394,-10.8214083018602,
6.16441400296896));
#22715=CARTESIAN_POINT('Ctrl Pts',(-42.0949797587142,-10.9674710310282,
6.70062138560751));
#22716=CARTESIAN_POINT('Ctrl Pts',(-42.0588133989563,-11.1051851219342,
7.21784327704638));
#22717=CARTESIAN_POINT('Ctrl Pts',(-41.9877513997445,-11.3709120573999,
8.28373602794749));
#22718=CARTESIAN_POINT('Ctrl Pts',(-41.9541547454919,-11.4940135235913,
8.81321169231162));
#22719=CARTESIAN_POINT('Ctrl Pts',(-41.9232160376671,-11.605772574848,9.34999999999142));
#22720=CARTESIAN_POINT('Origin',(-1.73472347597681E-15,-1.73472347597681E-15,
11.35));
#22721=CARTESIAN_POINT('Ctrl Pts',(-41.0461633054984,-14.4035578208427,
9.34999999999141));
#22722=CARTESIAN_POINT('Ctrl Pts',(-41.0263749722095,-14.4599491076223,
8.81613492202769));
#22723=CARTESIAN_POINT('Ctrl Pts',(-41.0044304289846,-14.5221093054493,
8.29345816614916));
#22724=CARTESIAN_POINT('Ctrl Pts',(-40.9570029893925,-14.6553380062871,
7.21621981188594));
#22725=CARTESIAN_POINT('Ctrl Pts',(-40.9326504745966,-14.7232050398857,
6.68773441334922));
#22726=CARTESIAN_POINT('Ctrl Pts',(-40.9094909763995,-14.7872765596607,
6.16441400296896));
#22727=CARTESIAN_POINT('Ctrl Pts',(-40.1636008708697,-16.7073386595674,
6.16440437643718));
#22728=CARTESIAN_POINT('Ctrl Pts',(-40.1056807345117,-16.8465757264749,
6.70061175907592));
#22729=CARTESIAN_POINT('Ctrl Pts',(-40.0502826977331,-16.9777435765864,
7.21784327704649));
#22730=CARTESIAN_POINT('Ctrl Pts',(-39.9421271213646,-17.2306526180706,
8.28373602794814));
#22731=CARTESIAN_POINT('Ctrl Pts',(-39.8913532673577,-17.3477197864173,
8.81321169231236));
#22732=CARTESIAN_POINT('Ctrl Pts',(-39.8448244996634,-17.4539382544751,
9.34999999999236));
#22733=CARTESIAN_POINT('Origin',(-1.73472347597681E-15,-1.73472347597681E-15,
11.35));
#22734=CARTESIAN_POINT('Ctrl Pts',(-38.5785325448956,-20.0984284630027,
9.34999999999236));
#22735=CARTESIAN_POINT('Ctrl Pts',(-38.550920311449,-20.1514295943407,8.81613492202805));
#22736=CARTESIAN_POINT('Ctrl Pts',(-38.5203528135318,-20.2098340568616,
8.29345816614786));
#22737=CARTESIAN_POINT('Ctrl Pts',(-38.4544476958771,-20.3349570532293,
7.21621981188626));
#22738=CARTESIAN_POINT('Ctrl Pts',(-38.4206845686576,-20.3986675740774,
6.68773441334922));
#22739=CARTESIAN_POINT('Ctrl Pts',(-38.3886424727843,-20.4587909979242,
6.16441400296896));
#22740=CARTESIAN_POINT('Ctrl Pts',(-37.3770897408172,-22.253160730712,6.16441400296896));
#22741=CARTESIAN_POINT('Ctrl Pts',(-37.2999436472748,-22.382737670203,6.7006213856076));
#22742=CARTESIAN_POINT('Ctrl Pts',(-37.2264437362619,-22.5046841317887,
7.21784327704656));
#22743=CARTESIAN_POINT('Ctrl Pts',(-37.0833963183767,-22.7396267805362,
8.28373602794849));
#22744=CARTESIAN_POINT('Ctrl Pts',(-37.0164788738633,-22.8482765010846,
8.81321169231301));
#22745=CARTESIAN_POINT('Ctrl Pts',(-36.9553072378319,-22.9467920842425,
9.34999999999332));
#22746=CARTESIAN_POINT('Origin',(-1.73472347597681E-15,-1.73472347597681E-15,
11.35));
#22747=CARTESIAN_POINT('Ctrl Pts',(-35.3255541129796,-25.3841530607375,
9.34999999999331));
#22748=CARTESIAN_POINT('Ctrl Pts',(-35.2906800848214,-25.4326850864425,
8.81613492202895));
#22749=CARTESIAN_POINT('Ctrl Pts',(-35.2521118983203,-25.4861448672246,
8.29345816614959));
#22750=CARTESIAN_POINT('Ctrl Pts',(-35.1690707407434,-25.6006150157417,
7.21621981188549));
#22751=CARTESIAN_POINT('Ctrl Pts',(-35.1265843210059,-25.6588720613605,
6.68773441334979));
#22752=CARTESIAN_POINT('Ctrl Pts',(-35.0863119121265,-25.7138234497512,
6.16441400296896));
#22753=CARTESIAN_POINT('Ctrl Pts',(-33.829691592081,-27.3459680169616,6.16440437643717));
#22754=CARTESIAN_POINT('Ctrl Pts',(-33.7348900133477,-27.4632470162174,
6.70061175907647));
#22755=CARTESIAN_POINT('Ctrl Pts',(-33.6447817325192,-27.5734942162178,
7.21784327704671));
#22756=CARTESIAN_POINT('Ctrl Pts',(-33.4697545060307,-27.7856877174186,
8.283736027949));
#22757=CARTESIAN_POINT('Ctrl Pts',(-33.3880557172072,-27.8837081951783,
8.81321169231373));
#22758=CARTESIAN_POINT('Ctrl Pts',(-33.3134864909438,-27.9725154002586,
9.34999999999427));
#22759=CARTESIAN_POINT('Origin',(-1.73472347597681E-15,-1.73472347597681E-15,
11.35));
#22760=CARTESIAN_POINT('Ctrl Pts',(-31.3534492698093,-30.1531295040083,
9.34999999999427));
#22761=CARTESIAN_POINT('Ctrl Pts',(-31.3120233815842,-30.1962044519918,
8.81613492202955));
#22762=CARTESIAN_POINT('Ctrl Pts',(-31.2662396435547,-30.2436312640638,
8.29345816614953));
#22763=CARTESIAN_POINT('Ctrl Pts',(-31.1677526127023,-30.3451186039619,
7.21621640088924));
#22764=CARTESIAN_POINT('Ctrl Pts',(-31.1174084080297,-30.39673560676,6.68773764820165));
#22765=CARTESIAN_POINT('Ctrl Pts',(-31.069725221506,-30.4453966086848,6.16441400296896));
#22766=CARTESIAN_POINT('Ctrl Pts',(-29.5936151100058,-31.8820944218042,
6.16441400296896));
#22767=CARTESIAN_POINT('Ctrl Pts',(-29.4830879328395,-31.9846880186044,
6.70062138560807));
#22768=CARTESIAN_POINT('Ctrl Pts',(-29.3782089962411,-32.0809874737957,
7.21784327704683));
#22769=CARTESIAN_POINT('Ctrl Pts',(-29.1747650107437,-32.266112179681,8.28373602794916));
#22770=CARTESIAN_POINT('Ctrl Pts',(-29.0799480293506,-32.3515080003924,
8.81321169231431));
#22771=CARTESIAN_POINT('Ctrl Pts',(-28.993499227262,-32.4287989687987,9.34999999999522));
#22772=CARTESIAN_POINT('Origin',(-1.73472347597681E-15,-1.73472347597681E-15,
11.35));
#22773=CARTESIAN_POINT('Ctrl Pts',(-26.7430794927964,-34.3082745010876,
9.35000993792185));
#22774=CARTESIAN_POINT('Ctrl Pts',(-26.6959450561263,-34.3450154896264,
8.81614485995699));
#22775=CARTESIAN_POINT('Ctrl Pts',(-26.6438769140361,-34.3854445437971,
8.29345816615072));
#22776=CARTESIAN_POINT('Ctrl Pts',(-26.5319495391965,-34.4718824493407,
7.21621981188563));
#22777=CARTESIAN_POINT('Ctrl Pts',(-26.4747712115681,-34.5158098676118,
6.68773441334982));
#22778=CARTESIAN_POINT('Ctrl Pts',(-26.4206485230644,-34.5571892899393,
6.16441400296896));
#22779=CARTESIAN_POINT('Ctrl Pts',(-24.7550996672026,-35.7691912190766,
6.16441400296896));
#22780=CARTESIAN_POINT('Ctrl Pts',(-24.6310969061966,-35.8550109036457,
6.7006213856071));
#22781=CARTESIAN_POINT('Ctrl Pts',(-24.5135806445582,-35.9354043403354,
7.21784327704669));
#22782=CARTESIAN_POINT('Ctrl Pts',(-24.2858614329126,-36.0896916457489,
8.28373602794951));
#22783=CARTESIAN_POINT('Ctrl Pts',(-24.1798564592615,-36.1607243967636,
8.81321169231496));
#22784=CARTESIAN_POINT('Ctrl Pts',(-24.0832879296606,-36.2249257072678,
9.34999999999617));
#22785=CARTESIAN_POINT('Origin',(-1.73472347597681E-15,-1.73472347597681E-15,
11.35));
#22786=CARTESIAN_POINT('Ctrl Pts',(-21.5882960010258,-37.7650033201653,
9.34999999999617));
#22787=CARTESIAN_POINT('Ctrl Pts',(-21.5364125371168,-37.7946624086852,
8.81613492203093));
#22788=CARTESIAN_POINT('Ctrl Pts',(-21.4791216851438,-37.8272693320525,
8.29345816615057));
#22789=CARTESIAN_POINT('Ctrl Pts',(-21.3560317832921,-37.8968987185778,
7.21621640088953));
#22790=CARTESIAN_POINT('Ctrl Pts',(-21.2931846824718,-37.932241268577,6.6877376482016));
#22791=CARTESIAN_POINT('Ctrl Pts',(-21.2337236115519,-37.9654972519553,
6.16441400296896));
#22792=CARTESIAN_POINT('Ctrl Pts',(-19.4126417829876,-38.9281304329582,
6.16441400296896));
#22793=CARTESIAN_POINT('Ctrl Pts',(-19.277687776761,-38.9954291640023,6.70062138560802));
#22794=CARTESIAN_POINT('Ctrl Pts',(-19.1499264822811,-39.0582800036546,
7.21784327704692));
#22795=CARTESIAN_POINT('Ctrl Pts',(-18.9025677509485,-39.1785890639858,
8.28373602794993));
#22796=CARTESIAN_POINT('Ctrl Pts',(-18.7875327406098,-39.2338127233347,
8.81321169231564));
#22797=CARTESIAN_POINT('Ctrl Pts',(-18.6828103402785,-39.2836174223961,
9.34999999999711));
#22798=CARTESIAN_POINT('Origin',(-1.73472347597681E-15,-1.73472347597681E-15,
11.35));
#22799=CARTESIAN_POINT('Ctrl Pts',(-15.9940379355884,-40.452944892986,9.34999999999712));
#22800=CARTESIAN_POINT('Ctrl Pts',(-15.9384616421462,-40.4749183079744,
8.81613492203165));
#22801=CARTESIAN_POINT('Ctrl Pts',(-15.8771134794141,-40.499040001544,8.29345816615128));
#22802=CARTESIAN_POINT('Ctrl Pts',(-15.7453675775635,-40.5504429790729,
7.21621981188616));
#22803=CARTESIAN_POINT('Ctrl Pts',(-15.678129590096,-40.5764820318145,6.68773441334964));
#22804=CARTESIAN_POINT('Ctrl Pts',(-15.6145413203107,-40.6009371733746,
6.16441400296896));
#22805=CARTESIAN_POINT('Ctrl Pts',(-13.674998493507,-41.2946051706828,6.16441400296896));
#22806=CARTESIAN_POINT('Ctrl Pts',(-13.5318405164519,-41.3420129401111,
6.70062138560741));
#22807=CARTESIAN_POINT('Ctrl Pts',(-13.3964350406525,-41.3860417208777,
7.21784327704686));
#22808=CARTESIAN_POINT('Ctrl Pts',(-13.1344723000791,-41.4699233906011,
8.28373602795046));
#22809=CARTESIAN_POINT('Ctrl Pts',(-13.0127490341297,-41.5082137638316,
8.81321169231636));
#22810=CARTESIAN_POINT('Ctrl Pts',(-12.9020046091443,-41.5426079714023,
9.34999999999807));
#22811=CARTESIAN_POINT('Origin',(-1.73472347597681E-15,-1.73472347597681E-15,
11.35));
#22812=CARTESIAN_POINT('Ctrl Pts',(-10.0741873807791,-42.3173811644454,
9.34999999999807));
#22813=CARTESIAN_POINT('Ctrl Pts',(-10.0160496308693,-42.3312215905391,
8.81613492203228));
#22814=CARTESIAN_POINT('Ctrl Pts',(-9.95189302905782,-42.3463670061912,
8.29345816615143));
#22815=CARTESIAN_POINT('Ctrl Pts',(-9.81417226801106,-42.3784974805493,
7.21621640088982));
#22816=CARTESIAN_POINT('Ctrl Pts',(-9.74391376938527,-42.3947023345391,
6.68773764820157));
#22817=CARTESIAN_POINT('Ctrl Pts',(-9.67749199640667,-42.4098590973784,
6.16441400296896));
#22818=CARTESIAN_POINT('Ctrl Pts',(-7.65897167013777,-42.82044083094,6.16441400296896));
#22819=CARTESIAN_POINT('Ctrl Pts',(-7.51052400583302,-42.8469925532797,
6.70062138560811));
#22820=CARTESIAN_POINT('Ctrl Pts',(-7.37023081372475,-42.8713029761527,
7.21784327704703));
#22821=CARTESIAN_POINT('Ctrl Pts',(-7.09899686987048,-42.9170496663673,
8.28373602795068));
#22822=CARTESIAN_POINT('Ctrl Pts',(-6.97306328298415,-42.9376272719008,
8.81321169231697));
#22823=CARTESIAN_POINT('Ctrl Pts',(-6.85855127047687,-42.9559108210994,
9.34999999999902));
#22824=CARTESIAN_POINT('Origin',(-1.73472347597681E-15,-1.73472347597681E-15,
11.35));
#22825=CARTESIAN_POINT('Ctrl Pts',(-3.94925542245455,-43.3203575886467,
9.34999999999902));
#22826=CARTESIAN_POINT('Ctrl Pts',(-3.88973973300997,-43.3257832746831,
8.81613492203305));
#22827=CARTESIAN_POINT('Ctrl Pts',(-3.82408073551961,-43.3316440954307,
8.29345816615224));
#22828=CARTESIAN_POINT('Ctrl Pts',(-3.68318957610294,-43.3438477814109,
7.21621981188656));
#22829=CARTESIAN_POINT('Ctrl Pts',(-3.61133915066117,-43.3498889394299,
6.68773441334963));
#22830=CARTESIAN_POINT('Ctrl Pts',(-3.54343684303821,-43.3554385900939,
6.16441400296896));
#22831=CARTESIAN_POINT('Ctrl Pts',(-1.48703027021498,-43.4745757998335,
6.16441400296896));
#22832=CARTESIAN_POINT('Ctrl Pts',(-1.33631488501835,-43.4797309585866,
6.70062138560807));
#22833=CARTESIAN_POINT('Ctrl Pts',(-1.19398994142009,-43.4838281334618,
7.21784327704716));
#22834=CARTESIAN_POINT('Ctrl Pts',(-0.919006335207703,-43.4905085734775,
8.2837360279511));
#22835=CARTESIAN_POINT('Ctrl Pts',(-0.791426072051028,-43.4929545106062,
8.81321169231764));
#22836=CARTESIAN_POINT('Ctrl Pts',(-0.675477606371082,-43.4947552010963,
9.34999999999997));
#22837=CARTESIAN_POINT('Origin',(-1.73472347597681E-15,-1.73472347597681E-15,
11.35));
#22838=CARTESIAN_POINT('',(-5.00000000000001,19.,11.35));
#22839=CARTESIAN_POINT('',(-5.00000000000001,19.,11.35));
#22840=CARTESIAN_POINT('',(5.00000000000001,19.,11.35));
#22841=CARTESIAN_POINT('',(-5.00000000000001,19.,11.35));
#22842=CARTESIAN_POINT('',(5.00000000000001,19.,11.35));
#22843=CARTESIAN_POINT('Origin',(-3.46944695195361E-15,1.73472347597681E-15,
-11.35));
#22844=CARTESIAN_POINT('',(-5.00000000000001,19.,-11.35));
#22845=CARTESIAN_POINT('',(-5.00000000000001,19.,-11.35));
#22846=CARTESIAN_POINT('',(5.,19.,-11.35));
#22847=CARTESIAN_POINT('',(5.,19.,-11.35));
#22848=CARTESIAN_POINT('',(-5.00000000000001,19.,-11.35));
#22849=CARTESIAN_POINT('Origin',(-5.00000000000001,19.,11.35));
#22850=CARTESIAN_POINT('',(-5.00000000000001,19.,11.35));
#22851=CARTESIAN_POINT('Origin',(5.00000000000001,19.,11.35));
#22852=CARTESIAN_POINT('',(5.00000000000001,19.,11.35));
#22853=CARTESIAN_POINT('Origin',(-5.00000000000001,19.,11.35));
#22854=CARTESIAN_POINT('Ctrl Pts',(1.19058808997907,-37.7800000000001,0.));
#22855=CARTESIAN_POINT('Ctrl Pts',(1.40487380426479,-37.7800000000001,3.24562220582793));
#22856=CARTESIAN_POINT('Ctrl Pts',(1.6191595185505,-39.1882226984277,6.16982677025167));
#22857=CARTESIAN_POINT('Ctrl Pts',(1.83344523283622,-40.5964453968553,9.09403133467541));
#22858=CARTESIAN_POINT('Ctrl Pts',(2.04773094712193,-43.1339750175689,11.1176436806954));
#22859=CARTESIAN_POINT('Ctrl Pts',(2.26201666140765,-45.6715046382825,13.1412560267153));
#22860=CARTESIAN_POINT('Ctrl Pts',(2.47630237569335,-48.8357523191413,13.8634749112255));
#22861=CARTESIAN_POINT('Ctrl Pts',(2.69058808997906,-52.0000000000001,14.5856937957357));
#22862=CARTESIAN_POINT('Ctrl Pts',(2.90487380426478,-55.1642476808588,13.8634749112255));
#22863=CARTESIAN_POINT('Ctrl Pts',(0.476235235991632,-37.1500000000001,
0.));
#22864=CARTESIAN_POINT('Ctrl Pts',(0.690520950277344,-37.1500000000001,
3.38941559469372));
#22865=CARTESIAN_POINT('Ctrl Pts',(0.904806664563056,-38.6206123116491,
6.44317352589573));
#22866=CARTESIAN_POINT('Ctrl Pts',(1.11909237884877,-40.0912246232982,9.49693145709774));
#22867=CARTESIAN_POINT('Ctrl Pts',(1.33337809313448,-42.7411764423979,11.6101975146502));
#22868=CARTESIAN_POINT('Ctrl Pts',(1.5476638074202,-45.3911282614975,13.7234635722027));
#22869=CARTESIAN_POINT('Ctrl Pts',(1.76194952170592,-48.6955641307488,14.4776794959001));
#22870=CARTESIAN_POINT('Ctrl Pts',(1.97623523599162,-52.,15.2318954195974));
#22871=CARTESIAN_POINT('Ctrl Pts',(2.19052095027735,-55.3044358692514,14.4776794959001));
#22872=CARTESIAN_POINT('Ctrl Pts',(-0.476235235991626,-37.1500000000001,
0.));
#22873=CARTESIAN_POINT('Ctrl Pts',(-0.261949521705911,-37.1500000000001,
3.38941559469374));
#22874=CARTESIAN_POINT('Ctrl Pts',(-0.0476638074202001,-38.6206123116491,
6.44317352589574));
#22875=CARTESIAN_POINT('Ctrl Pts',(0.166621906865511,-40.0912246232982,
9.49693145709774));
#22876=CARTESIAN_POINT('Ctrl Pts',(0.380907621151232,-42.7411764423979,
11.6101975146502));
#22877=CARTESIAN_POINT('Ctrl Pts',(0.595193335436941,-45.3911282614975,
13.7234635722027));
#22878=CARTESIAN_POINT('Ctrl Pts',(0.809479049722664,-48.6955641307488,
14.4776794959001));
#22879=CARTESIAN_POINT('Ctrl Pts',(1.02376476400836,-52.,15.2318954195974));
#22880=CARTESIAN_POINT('Ctrl Pts',(1.23805047829409,-55.3044358692514,14.4776794959001));
#22881=CARTESIAN_POINT('Ctrl Pts',(-1.19058808997907,-37.7800000000001,
0.));
#22882=CARTESIAN_POINT('Ctrl Pts',(-0.976302375693358,-37.7800000000001,
3.24562220582793));
#22883=CARTESIAN_POINT('Ctrl Pts',(-0.762016661407643,-39.1882226984277,
6.16982677025167));
#22884=CARTESIAN_POINT('Ctrl Pts',(-0.547730947121919,-40.5964453968553,
9.09403133467541));
#22885=CARTESIAN_POINT('Ctrl Pts',(-0.333445232836209,-43.1339750175689,
11.1176436806954));
#22886=CARTESIAN_POINT('Ctrl Pts',(-0.119159518550487,-45.6715046382825,
13.1412560267153));
#22887=CARTESIAN_POINT('Ctrl Pts',(0.0951261957352154,-48.8357523191413,
13.8634749112255));
#22888=CARTESIAN_POINT('Ctrl Pts',(0.309411910020934,-52.0000000000001,
14.5856937957357));
#22889=CARTESIAN_POINT('Ctrl Pts',(0.523697624306638,-55.1642476808588,
13.8634749112255));
#22890=CARTESIAN_POINT('',(-1.19058808997887,-37.7800000000033,1.58522090049187E-9));
#22891=CARTESIAN_POINT('Ctrl Pts',(-1.19058808977083,-37.7800000000001,
3.15398724759345E-9));
#22892=CARTESIAN_POINT('Ctrl Pts',(-1.17440993602501,-37.7800000000544,
0.245038153359724));
#22893=CARTESIAN_POINT('Ctrl Pts',(-1.15808907769182,-37.7863378834492,
0.49079116054718));
#22894=CARTESIAN_POINT('Ctrl Pts',(-1.1416567390423,-37.7990994960401,0.736766500751943));
#22895=CARTESIAN_POINT('Ctrl Pts',(-1.12527834683773,-37.8118192129736,
0.981934317728601));
#22896=CARTESIAN_POINT('Ctrl Pts',(-1.10878923236178,-37.8309206530838,
1.22732257379415));
#22897=CARTESIAN_POINT('Ctrl Pts',(-1.09222177854598,-37.8564381709177,
1.47243294819272));
#22898=CARTESIAN_POINT('Ctrl Pts',(-1.07567927587712,-37.8819172585049,
1.71717417806026));
#22899=CARTESIAN_POINT('Ctrl Pts',(-1.05905869844395,-37.9137931614489,
1.96163791544663));
#22900=CARTESIAN_POINT('Ctrl Pts',(-1.04239332675412,-37.9520483461932,
2.20532408781658));
#22901=CARTESIAN_POINT('Ctrl Pts',(-1.02574224814004,-37.990270721333,2.44880126245258));
#22902=CARTESIAN_POINT('Ctrl Pts',(-1.00904648207997,-38.0348614248357,
2.69150175434289));
#22903=CARTESIAN_POINT('Ctrl Pts',(-0.992339825173114,-38.0857510285919,
2.93292951870084));
#22904=CARTESIAN_POINT('Ctrl Pts',(-0.975636663332195,-38.1366299861415,
3.17430677588902));
#22905=CARTESIAN_POINT('Ctrl Pts',(-0.958922645775983,-38.1938051285017,
3.41441139321683));
#22906=CARTESIAN_POINT('Ctrl Pts',(-0.942231694696393,-38.2571558430123,
3.65275710617991));
#22907=CARTESIAN_POINT('Ctrl Pts',(-0.925519549713774,-38.3205869992482,
3.89140546672155));
#22908=CARTESIAN_POINT('Ctrl Pts',(-0.908830560429391,-38.3902092841862,
4.12829002084532));
#22909=CARTESIAN_POINT('Ctrl Pts',(-0.892198465543069,-38.4658518732155,
4.36293874381168));
#22910=CARTESIAN_POINT('Ctrl Pts',(-0.875549399287467,-38.5415716478501,
4.59782690204795));
#22911=CARTESIAN_POINT('Ctrl Pts',(-0.858957373411739,-38.6233238148463,
4.83047425898284));
#22912=CARTESIAN_POINT('Ctrl Pts',(-0.842455462103365,-38.7108897721526,
5.06042975962723));
#22913=CARTESIAN_POINT('Ctrl Pts',(-0.825905305674876,-38.7987117379933,
5.29105756001572));
#22914=CARTESIAN_POINT('Ctrl Pts',(-0.809445820257816,-38.8923812869644,
5.51897736308919));
#22915=CARTESIAN_POINT('Ctrl Pts',(-0.79310915730404,-38.9916337971041,
5.74376259357518));
#22916=CARTESIAN_POINT('Ctrl Pts',(-0.782692415217241,-39.0549201489446,
5.887092340753));
#22917=CARTESIAN_POINT('Ctrl Pts',(-0.772325583322888,-39.1204754951866,
6.02914825316372));
#22918=CARTESIAN_POINT('Ctrl Pts',(-0.762016661407643,-39.1882226984277,
6.16982677025167));
#22919=CARTESIAN_POINT('Ctrl Pts',(-0.74585196858537,-39.2944523060397,
6.39041482340753));
#22920=CARTESIAN_POINT('Ctrl Pts',(-0.729544808776673,-39.406692292665,
6.60890054013437));
#22921=CARTESIAN_POINT('Ctrl Pts',(-0.713126327696533,-39.5248066659344,
6.82480412009635));
#22922=CARTESIAN_POINT('Ctrl Pts',(-0.696744912258959,-39.6426543893767,
7.04022028560845));
#22923=CARTESIAN_POINT('Ctrl Pts',(-0.680252704622003,-39.7663499173029,
7.25306552031141));
#22924=CARTESIAN_POINT('Ctrl Pts',(-0.663682105814804,-39.8957079164889,
7.46287566270863));
#22925=CARTESIAN_POINT('Ctrl Pts',(-0.647138159319839,-40.0248578550113,
7.67234834443288));
#22926=CARTESIAN_POINT('Ctrl Pts',(-0.630516102446333,-40.1596519133109,
7.87879526534386));
#22927=CARTESIAN_POINT('Ctrl Pts',(-0.613849224526778,-40.2998572837037,
8.08177334613496));
#22928=CARTESIAN_POINT('Ctrl Pts',(-0.597198339076355,-40.4399281219983,
8.28455666215324));
#22929=CARTESIAN_POINT('Ctrl Pts',(-0.580502748574263,-40.5853996820896,
8.48387739273973));
#22930=CARTESIAN_POINT('Ctrl Pts',(-0.563796248533928,-40.7359942171173,
8.67931873612112));
#22931=CARTESIAN_POINT('Ctrl Pts',(-0.547088944955135,-40.8865959953438,
8.87476947971412));
#22932=CARTESIAN_POINT('Ctrl Pts',(-0.53037076138362,-41.0423209776528,
9.06634009533642));
#22933=CARTESIAN_POINT('Ctrl Pts',(-0.513675645355332,-41.2028492923188,
9.25364450341684));
#22934=CARTESIAN_POINT('Ctrl Pts',(-0.496974404888472,-41.363436495213,
9.44101762227112));
#22935=CARTESIAN_POINT('Ctrl Pts',(-0.480296279392564,-41.5288302394218,
9.62412107875557));
#22936=CARTESIAN_POINT('Ctrl Pts',(-0.463674941839292,-41.6986725382703,
9.80260437466549));
#22937=CARTESIAN_POINT('Ctrl Pts',(-0.447026491441732,-41.8687918850872,
9.98137881379988));
#22938=CARTESIAN_POINT('Ctrl Pts',(-0.43043504426164,-42.0433739554922,
10.1555177270943));
#22939=CARTESIAN_POINT('Ctrl Pts',(-0.413933671136304,-42.2220261712039,
10.3247095747714));
#22940=CARTESIAN_POINT('Ctrl Pts',(-0.409164215743291,-42.2736627087955,
10.3736117457742));
#22941=CARTESIAN_POINT('Ctrl Pts',(-0.404402278730915,-42.3256390786474,
10.4221009095726));
#22942=CARTESIAN_POINT('Ctrl Pts',(-0.399648641329912,-42.3779453595728,
10.4701702229062));
#22943=CARTESIAN_POINT('',(-4.97404252170606E-6,-37.3300000000069,1.04083408558609E-14));
#22944=CARTESIAN_POINT('Origin',(-1.73472347597681E-15,-39.13,1.04083408558608E-14));
#22945=CARTESIAN_POINT('',(1.19058808997907,-37.78,0.));
#22946=CARTESIAN_POINT('Origin',(-1.73472347597681E-15,-39.13,1.04083408558608E-14));
#22947=CARTESIAN_POINT('Ctrl Pts',(1.19058808997907,-37.78,0.));
#22948=CARTESIAN_POINT('Ctrl Pts',(1.40487380426478,-37.7800000000001,3.24562220582793));
#22949=CARTESIAN_POINT('Ctrl Pts',(1.6191595185505,-39.1882226984277,6.16982677025167));
#22950=CARTESIAN_POINT('Ctrl Pts',(1.79805338220529,-40.3638605623321,8.61106394926976));
#22951=CARTESIAN_POINT('Ctrl Pts',(1.97942721139903,-42.3548619717231,10.4489096280657));
#22952=CARTESIAN_POINT('Ctrl Pts',(3.45,-44.43,0.));
#22953=CARTESIAN_POINT('Ctrl Pts',(3.66428571428572,-44.4300000000001,1.72780310113343));
#22954=CARTESIAN_POINT('Ctrl Pts',(3.87857142857143,-45.1796656699787,3.28449990511991));
#22955=CARTESIAN_POINT('Ctrl Pts',(4.09285714285715,-45.9293313399574,4.84119670910639));
#22956=CARTESIAN_POINT('Ctrl Pts',(4.30714285714286,-47.2801821999294,5.91846432228298));
#22957=CARTESIAN_POINT('Ctrl Pts',(4.52142857142857,-48.6310330599015,6.99573193545956));
#22958=CARTESIAN_POINT('Ctrl Pts',(4.73571428571428,-50.3155165299508,7.38020429521639));
#22959=CARTESIAN_POINT('Ctrl Pts',(4.95,-52.0000000000001,7.76467665497322));
#22960=CARTESIAN_POINT('Ctrl Pts',(5.16428571428571,-53.6844834700494,7.38020429521639));
#22961=CARTESIAN_POINT('Ctrl Pts',(2.26368121662725,-42.3765540157191,0.));
#22962=CARTESIAN_POINT('Ctrl Pts',(2.47796693091296,-42.3765540157191,2.19648874705823));
#22963=CARTESIAN_POINT('Ctrl Pts',(2.69225264519868,-43.3295747662224,4.17545672685567));
#22964=CARTESIAN_POINT('Ctrl Pts',(2.90653835948438,-44.2825955167256,6.15442470665314));
#22965=CARTESIAN_POINT('Ctrl Pts',(3.12082407377011,-45.9998795700625,7.5239130403414));
#22966=CARTESIAN_POINT('Ctrl Pts',(3.33510978805582,-47.7171636233994,8.89340137402968));
#22967=CARTESIAN_POINT('Ctrl Pts',(3.54939550234153,-49.8585818116997,9.38216610144961));
#22968=CARTESIAN_POINT('Ctrl Pts',(3.76368121662725,-52.0000000000001,9.87093082886953));
#22969=CARTESIAN_POINT('Ctrl Pts',(3.97796693091296,-54.1414181883004,9.3821661014496));
#22970=CARTESIAN_POINT('Ctrl Pts',(1.50077089879006,-40.1311229851416,0.));
#22971=CARTESIAN_POINT('Ctrl Pts',(1.71505661307578,-40.1311229851416,2.70899372698069));
#22972=CARTESIAN_POINT('Ctrl Pts',(1.92934232736149,-41.30651131265,5.14971273833323));
#22973=CARTESIAN_POINT('Ctrl Pts',(2.1436280416472,-42.4818996401584,7.59043174968577));
#22974=CARTESIAN_POINT('Ctrl Pts',(2.35791375593292,-44.5998762217203,9.27946171175751));
#22975=CARTESIAN_POINT('Ctrl Pts',(2.57219947021862,-46.7178528032822,10.9684916738293));
#22976=CARTESIAN_POINT('Ctrl Pts',(2.78648518450434,-49.3589264016411,11.5712994880388));
#22977=CARTESIAN_POINT('Ctrl Pts',(3.00077089879007,-52.0000000000001,12.1741073022483));
#22978=CARTESIAN_POINT('Ctrl Pts',(3.21505661307576,-54.641073598359,11.5712994880388));
#22979=CARTESIAN_POINT('Ctrl Pts',(1.19058808997907,-37.78,0.));
#22980=CARTESIAN_POINT('Ctrl Pts',(1.40487380426479,-37.7800000000001,3.24562220582793));
#22981=CARTESIAN_POINT('Ctrl Pts',(1.6191595185505,-39.1882226984276,6.16982677025167));
#22982=CARTESIAN_POINT('Ctrl Pts',(1.83344523283622,-40.5964453968553,9.09403133467541));
#22983=CARTESIAN_POINT('Ctrl Pts',(2.04773094712193,-43.1339750175689,11.1176436806954));
#22984=CARTESIAN_POINT('Ctrl Pts',(2.26201666140765,-45.6715046382825,13.1412560267153));
#22985=CARTESIAN_POINT('Ctrl Pts',(2.47630237569336,-48.8357523191413,13.8634749112255));
#22986=CARTESIAN_POINT('Ctrl Pts',(2.69058808997906,-52.0000000000001,14.5856937957357));
#22987=CARTESIAN_POINT('Ctrl Pts',(2.90487380426478,-55.1642476808588,13.8634749112255));
#22988=CARTESIAN_POINT('Origin',(19.0359549110502,-35.425667181256,0.));
#22989=CARTESIAN_POINT('Ctrl Pts',(-1.19058808997907,-37.7800000000001,
0.));
#22990=CARTESIAN_POINT('Ctrl Pts',(-0.976302375693358,-37.7800000000001,
3.24562220582793));
#22991=CARTESIAN_POINT('Ctrl Pts',(-0.762016661407643,-39.1882226984276,
6.16982677025168));
#22992=CARTESIAN_POINT('Ctrl Pts',(-0.547730947121923,-40.5964453968553,
9.09403133467541));
#22993=CARTESIAN_POINT('Ctrl Pts',(-0.333445232836209,-43.1339750175689,
11.1176436806954));
#22994=CARTESIAN_POINT('Ctrl Pts',(-0.119159518550493,-45.6715046382825,
13.1412560267153));
#22995=CARTESIAN_POINT('Ctrl Pts',(0.0951261957352102,-48.8357523191413,
13.8634749112255));
#22996=CARTESIAN_POINT('Ctrl Pts',(0.309411910020934,-52.0000000000001,
14.5856937957357));
#22997=CARTESIAN_POINT('Ctrl Pts',(0.523697624306634,-55.1642476808588,
13.8634749112255));
#22998=CARTESIAN_POINT('Ctrl Pts',(-1.50077089879006,-40.1311229851416,
0.));
#22999=CARTESIAN_POINT('Ctrl Pts',(-1.28648518450434,-40.1311229851416,
2.70899372698069));
#23000=CARTESIAN_POINT('Ctrl Pts',(-1.07219947021864,-41.3065113126499,
5.14971273833323));
#23001=CARTESIAN_POINT('Ctrl Pts',(-0.857913755932923,-42.4818996401584,
7.59043174968577));
#23002=CARTESIAN_POINT('Ctrl Pts',(-0.643628041647201,-44.5998762217203,
9.27946171175751));
#23003=CARTESIAN_POINT('Ctrl Pts',(-0.429342327361493,-46.7178528032822,
10.9684916738293));
#23004=CARTESIAN_POINT('Ctrl Pts',(-0.215056613075784,-49.3589264016411,
11.5712994880388));
#23005=CARTESIAN_POINT('Ctrl Pts',(-0.000770898790054586,-52.0000000000001,
12.1741073022483));
#23006=CARTESIAN_POINT('Ctrl Pts',(0.213514815495646,-54.641073598359,11.5712994880388));
#23007=CARTESIAN_POINT('Ctrl Pts',(-2.26368121662725,-42.3765540157191,
0.));
#23008=CARTESIAN_POINT('Ctrl Pts',(-2.04939550234155,-42.3765540157191,
2.19648874705823));
#23009=CARTESIAN_POINT('Ctrl Pts',(-1.83510978805583,-43.3295747662223,
4.17545672685568));
#23010=CARTESIAN_POINT('Ctrl Pts',(-1.62082407377013,-44.2825955167256,
6.15442470665313));
#23011=CARTESIAN_POINT('Ctrl Pts',(-1.4065383594844,-45.9998795700625,7.5239130403414));
#23012=CARTESIAN_POINT('Ctrl Pts',(-1.19225264519869,-47.7171636233994,
8.89340137402967));
#23013=CARTESIAN_POINT('Ctrl Pts',(-0.977966930912963,-49.8585818116997,
9.3821661014496));
#23014=CARTESIAN_POINT('Ctrl Pts',(-0.763681216627249,-52.0000000000001,
9.87093082886953));
#23015=CARTESIAN_POINT('Ctrl Pts',(-0.549395502341532,-54.1414181883004,
9.3821661014496));
#23016=CARTESIAN_POINT('Ctrl Pts',(-3.45,-44.4300000000001,0.));
#23017=CARTESIAN_POINT('Ctrl Pts',(-3.23571428571428,-44.4300000000001,
1.72780310113343));
#23018=CARTESIAN_POINT('Ctrl Pts',(-3.02142857142857,-45.1796656699788,
3.28449990511991));
#23019=CARTESIAN_POINT('Ctrl Pts',(-2.80714285714286,-45.9293313399574,
4.84119670910638));
#23020=CARTESIAN_POINT('Ctrl Pts',(-2.59285714285715,-47.2801821999294,
5.91846432228297));
#23021=CARTESIAN_POINT('Ctrl Pts',(-2.37857142857143,-48.6310330599014,
6.99573193545956));
#23022=CARTESIAN_POINT('Ctrl Pts',(-2.16428571428571,-50.3155165299508,
7.38020429521639));
#23023=CARTESIAN_POINT('Ctrl Pts',(-1.95000000000001,-52.0000000000001,
7.76467665497322));
#23024=CARTESIAN_POINT('Ctrl Pts',(-1.73571428571428,-53.6844834700494,
7.38020429521639));
#23025=CARTESIAN_POINT('Origin',(-19.0359549110502,-35.425667181256,0.));
#23026=CARTESIAN_POINT('Ctrl Pts',(1.06226042837001,-37.8397258902528,1.59647049649061));
#23027=CARTESIAN_POINT('Ctrl Pts',(1.10262802813221,-37.8163671782172,1.15259151032668));
#23028=CARTESIAN_POINT('Ctrl Pts',(1.14747953738505,-37.7797757625757,0.635572917996464));
#23029=CARTESIAN_POINT('Ctrl Pts',(1.31732736909556,-37.7806592587273,-1.86858636177033));
#23030=CARTESIAN_POINT('Ctrl Pts',(1.43803115336731,-38.1455252315354,-3.71029995869598));
#23031=CARTESIAN_POINT('Ctrl Pts',(1.69365713820689,-39.5779229780087,-7.16936247493924));
#23032=CARTESIAN_POINT('Ctrl Pts',(1.81514228728894,-40.6266263701707,-8.73699595770183));
#23033=CARTESIAN_POINT('Ctrl Pts',(2.0664373721633,-43.2633442117449,-11.373025698218));
#23034=CARTESIAN_POINT('Ctrl Pts',(2.18792249430893,-44.8298904725309,-12.4235805192224));
#23035=CARTESIAN_POINT('Ctrl Pts',(2.44354852690307,-48.2902066278842,-13.85294708216));
#23036=CARTESIAN_POINT('Ctrl Pts',(2.56492073910889,-50.1387215498278,-14.2204718556691));
#23037=CARTESIAN_POINT('Ctrl Pts',(2.69099156569462,-51.9999633056261,-14.2198708430667));
#23038=CARTESIAN_POINT('Ctrl Pts',(0.347755560296868,-37.2107726459064,
1.62964593809825));
#23039=CARTESIAN_POINT('Ctrl Pts',(0.387786383581994,-37.1876088095763,
1.18947011987008));
#23040=CARTESIAN_POINT('Ctrl Pts',(0.433007907800631,-37.1499104513489,
0.664243870396088));
#23041=CARTESIAN_POINT('Ctrl Pts',(0.603323715733815,-37.150263273314,-1.95287905127288));
#23042=CARTESIAN_POINT('Ctrl Pts',(0.72328369871309,-37.5316956084199,-3.87337387078179));
#23043=CARTESIAN_POINT('Ctrl Pts',(0.979785618814997,-39.027330971542,-7.48792130214399));
#23044=CARTESIAN_POINT('Ctrl Pts',(1.10069469072639,-40.1224384633822,-9.12360836231754));
#23045=CARTESIAN_POINT('Ctrl Pts',(1.35224759480683,-42.8765051571252,-11.8774049927137));
#23046=CARTESIAN_POINT('Ctrl Pts',(1.47315665468806,-44.5117551326448,-12.9732563608769));
#23047=CARTESIAN_POINT('Ctrl Pts',(1.72965859378933,-48.126801308994,-14.4676858045579));
#23048=CARTESIAN_POINT('Ctrl Pts',(1.85032539219322,-50.0548871962143,-14.8501851005342));
#23049=CARTESIAN_POINT('Ctrl Pts',(1.97670704765982,-51.9999570907663,-14.8499483202528));
#23050=CARTESIAN_POINT('Ctrl Pts',(-0.604714876209436,-37.2110085708708,
1.62975512103804));
#23051=CARTESIAN_POINT('Ctrl Pts',(-0.564689496472769,-37.1878478844499,
1.18963915964465));
#23052=CARTESIAN_POINT('Ctrl Pts',(-0.519462564176609,-37.1500900231906,
0.664246312466032));
#23053=CARTESIAN_POINT('Ctrl Pts',(-0.34914675626714,-37.1497353315388,
-1.95288623096613));
#23054=CARTESIAN_POINT('Ctrl Pts',(-0.229186815972883,-37.5322524147635,
-3.87317034518711));
#23055=CARTESIAN_POINT('Ctrl Pts',(0.0273151950961837,-39.0266771563425,
-7.48823335804281));
#23056=CARTESIAN_POINT('Ctrl Pts',(0.148224209656984,-40.1225272605589,
-9.12349227713643));
#23057=CARTESIAN_POINT('Ctrl Pts',(0.399777134874542,-42.8763256602578,
-11.8775764776329));
#23058=CARTESIAN_POINT('Ctrl Pts',(0.520686157648162,-44.5120149889529,
-12.9726927515284));
#23059=CARTESIAN_POINT('Ctrl Pts',(0.777188149407483,-48.1265710168792,
-14.4683433355078));
#23060=CARTESIAN_POINT('Ctrl Pts',(0.897861662853934,-50.0549848089201,
-14.8498038985528));
#23061=CARTESIAN_POINT('Ctrl Pts',(1.02423658127911,-51.9999570902567,-14.8500516281495));
#23062=CARTESIAN_POINT('Ctrl Pts',(-1.31891566289573,-37.8403157026637,
1.59674345384007));
#23063=CARTESIAN_POINT('Ctrl Pts',(-1.27856167200511,-37.816964865386,1.15301410976404));
#23064=CARTESIAN_POINT('Ctrl Pts',(-1.23369664255802,-37.7802246921786,
0.635579023171327));
#23065=CARTESIAN_POINT('Ctrl Pts',(-1.06384881090689,-37.7793394042942,
-1.86860431100347));
#23066=CARTESIAN_POINT('Ctrl Pts',(-0.943145133347884,-38.1469172473993,
-3.70979114470452));
#23067=CARTESIAN_POINT('Ctrl Pts',(-0.687518921089859,-39.5762884400051,
-7.17014261469109));
#23068=CARTESIAN_POINT('Ctrl Pts',(-0.566033915384881,-40.6268483631173,
-8.73670574474909));
#23069=CARTESIAN_POINT('Ctrl Pts',(-0.314738777667137,-43.2628954695717,
-11.373454410516));
#23070=CARTESIAN_POINT('Ctrl Pts',(-0.193253748290483,-44.8305401132962,
-12.4221714958367));
#23071=CARTESIAN_POINT('Ctrl Pts',(0.0623724159481351,-48.2896308976019,
-13.8545909095489));
#23072=CARTESIAN_POINT('Ctrl Pts',(0.183762141934924,-50.1389656602283,
-14.2195188100007));
#23073=CARTESIAN_POINT('Ctrl Pts',(0.309815399742843,-51.9999633043522,
-14.2201291128083));
#23074=CARTESIAN_POINT('Ctrl Pts',(1.19058808997907,-37.78,0.));
#23075=CARTESIAN_POINT('Ctrl Pts',(1.31732736909556,-37.7806592587273,-1.86858636177033));
#23076=CARTESIAN_POINT('Ctrl Pts',(1.43803115336731,-38.1455252315354,-3.71029995869598));
#23077=CARTESIAN_POINT('Ctrl Pts',(1.69365713820689,-39.5779229780087,-7.16936247493924));
#23078=CARTESIAN_POINT('Ctrl Pts',(1.81514228728894,-40.6266263701707,-8.73699595770183));
#23079=CARTESIAN_POINT('Ctrl Pts',(1.95357130555244,-42.0790951378326,-10.1890856763505));
#23080=CARTESIAN_POINT('Ctrl Pts',(1.96630970889272,-42.2157732130427,-10.3203928635177));
#23081=CARTESIAN_POINT('Ctrl Pts',(1.97901608230067,-42.3549304887752,-10.4488603766009));
#23082=CARTESIAN_POINT('Ctrl Pts',(-1.19058808997907,-37.7800000000001,
2.1094237467878E-15));
#23083=CARTESIAN_POINT('Ctrl Pts',(-1.06384881090689,-37.7793394042942,
-1.86860431100347));
#23084=CARTESIAN_POINT('Ctrl Pts',(-0.943145133347884,-38.1469172473993,
-3.70979114470452));
#23085=CARTESIAN_POINT('Ctrl Pts',(-0.687518921089859,-39.5762884400051,
-7.17014261469109));
#23086=CARTESIAN_POINT('Ctrl Pts',(-0.566033915384881,-40.6268483631173,
-8.73670574474909));
#23087=CARTESIAN_POINT('Ctrl Pts',(-0.42689829031798,-42.0863595386748,
-10.1966053555719));
#23088=CARTESIAN_POINT('Ctrl Pts',(-0.41345820181274,-42.2307237103642,
-10.3350231942276));
#23089=CARTESIAN_POINT('Ctrl Pts',(-0.400053103665672,-42.3778559173188,
-10.4702558451));
#23090=CARTESIAN_POINT('Ctrl Pts',(3.32327712822012,-44.4799848904464,1.24689064510955));
#23091=CARTESIAN_POINT('Ctrl Pts',(3.36716940899972,-44.4545866217131,0.764254540719014));
#23092=CARTESIAN_POINT('Ctrl Pts',(3.40814518985255,-44.429349685102,0.332948627185772));
#23093=CARTESIAN_POINT('Ctrl Pts',(3.57305327241219,-44.4319119278293,-0.978870002659466));
#23094=CARTESIAN_POINT('Ctrl Pts',(3.70160805588082,-44.6279251367563,-1.98783577088437));
#23095=CARTESIAN_POINT('Ctrl Pts',(3.94798856176874,-45.3861024076399,-3.80852727284065));
#23096=CARTESIAN_POINT('Ctrl Pts',(4.07555420744412,-45.9491021672716,-4.65544360722303));
#23097=CARTESIAN_POINT('Ctrl Pts',(4.32412798456521,-47.3456501222045,-6.04997283343043));
#23098=CARTESIAN_POINT('Ctrl Pts',(4.45169355820317,-48.1894265020396,-6.618321698991));
#23099=CARTESIAN_POINT('Ctrl Pts',(4.69807420295718,-50.013763693226,-7.36768403082578));
#23100=CARTESIAN_POINT('Ctrl Pts',(4.82686758916904,-51.0241709100527,-7.57138648682318));
#23101=CARTESIAN_POINT('Ctrl Pts',(4.94968218283415,-52.0000289040989,-7.56962581969448));
#23102=CARTESIAN_POINT('Ctrl Pts',(2.13646282181016,-42.4296678529921,1.35489302548968));
#23103=CARTESIAN_POINT('Ctrl Pts',(2.17926392766628,-42.4049009926309,0.884255395658553));
#23104=CARTESIAN_POINT('Ctrl Pts',(2.22143926476967,-42.3761273929605,0.426396892757904));
#23105=CARTESIAN_POINT('Ctrl Pts',(2.38787268687497,-42.3778082879602,-1.25360819498149));
#23106=CARTESIAN_POINT('Ctrl Pts',(2.5140031472761,-42.6265178497758,-2.51960912779656));
#23107=CARTESIAN_POINT('Ctrl Pts',(2.76323860082846,-43.5922658248206,-4.8464758678243));
#23108=CARTESIAN_POINT('Ctrl Pts',(2.8889266274111,-44.3056264360906,-5.91572199046689));
#23109=CARTESIAN_POINT('Ctrl Pts',(3.13834072492096,-46.0849874081721,-7.69376028692028));
#23110=CARTESIAN_POINT('Ctrl Pts',(3.26402870377777,-47.1521724801729,-8.41063186554706));
#23111=CARTESIAN_POINT('Ctrl Pts',(3.51326424840899,-49.4814303102184,-9.37059840621927));
#23112=CARTESIAN_POINT('Ctrl Pts',(3.63979023544684,-50.7508064960244,-9.62435378625662));
#23113=CARTESIAN_POINT('Ctrl Pts',(3.76358612954926,-52.0000086477592,-9.62320046360554));
#23114=CARTESIAN_POINT('Ctrl Pts',(1.37301063256244,-40.1875259567355,1.47293173916723));
#23115=CARTESIAN_POINT('Ctrl Pts',(1.41462159884989,-40.1634477706497,1.01538079142922));
#23116=CARTESIAN_POINT('Ctrl Pts',(1.45810560976048,-40.1308402311943,0.52858064812525));
#23117=CARTESIAN_POINT('Ctrl Pts',(1.62620698164419,-40.1319542826288,-1.55402875455442));
#23118=CARTESIAN_POINT('Ctrl Pts',(1.74968648306502,-40.4376784663506,-3.10121432123458));
#23119=CARTESIAN_POINT('Ctrl Pts',(2.00204375396077,-41.6310829191854,-5.98129145450958));
#23120=CARTESIAN_POINT('Ctrl Pts',(2.12567864735027,-42.5084456369459,-7.29389406576053));
#23121=CARTESIAN_POINT('Ctrl Pts',(2.3760116183751,-44.7065608867208,-9.49113593804617));
#23122=CARTESIAN_POINT('Ctrl Pts',(2.49964647926793,-46.0177955705498,-10.3708286017073));
#23123=CARTESIAN_POINT('Ctrl Pts',(2.75200381047715,-48.8994560970608,-11.5604045561349));
#23124=CARTESIAN_POINT('Ctrl Pts',(2.87602039417755,-50.4518266808844,-11.8694761541618));
#23125=CARTESIAN_POINT('Ctrl Pts',(3.000919362602,-51.9999864978575,-11.8687142284813));
#23126=CARTESIAN_POINT('Ctrl Pts',(1.06226042837001,-37.8397258902528,1.59647049649061));
#23127=CARTESIAN_POINT('Ctrl Pts',(1.10262802813221,-37.8163671782172,1.15259151032668));
#23128=CARTESIAN_POINT('Ctrl Pts',(1.14747953738505,-37.7797757625757,0.635572917996464));
#23129=CARTESIAN_POINT('Ctrl Pts',(1.31732736909556,-37.7806592587273,-1.86858636177033));
#23130=CARTESIAN_POINT('Ctrl Pts',(1.43803115336731,-38.1455252315354,-3.71029995869598));
#23131=CARTESIAN_POINT('Ctrl Pts',(1.69365713820689,-39.5779229780087,-7.16936247493924));
#23132=CARTESIAN_POINT('Ctrl Pts',(1.81514228728894,-40.6266263701707,-8.73699595770183));
#23133=CARTESIAN_POINT('Ctrl Pts',(2.0664373721633,-43.2633442117449,-11.373025698218));
#23134=CARTESIAN_POINT('Ctrl Pts',(2.18792249430953,-44.8298904725309,-12.4235805192224));
#23135=CARTESIAN_POINT('Ctrl Pts',(2.44354852690246,-48.2902066278842,-13.85294708216));
#23136=CARTESIAN_POINT('Ctrl Pts',(2.56492073910889,-50.1387215498278,-14.2204718556691));
#23137=CARTESIAN_POINT('Ctrl Pts',(2.69099156569462,-51.9999633056261,-14.2198708430667));
#23138=CARTESIAN_POINT('Ctrl Pts',(-1.31891566289574,-37.8403157026637,
1.59674345384007));
#23139=CARTESIAN_POINT('Ctrl Pts',(-1.27856167200496,-37.816964865386,1.15301410976406));
#23140=CARTESIAN_POINT('Ctrl Pts',(-1.23369664255802,-37.7802246921786,
0.635579023171327));
#23141=CARTESIAN_POINT('Ctrl Pts',(-1.06384881090689,-37.7793394042942,
-1.86860431100347));
#23142=CARTESIAN_POINT('Ctrl Pts',(-0.943145133347888,-38.1469172473993,
-3.70979114470452));
#23143=CARTESIAN_POINT('Ctrl Pts',(-0.687518921089859,-39.5762884400051,
-7.17014261469109));
#23144=CARTESIAN_POINT('Ctrl Pts',(-0.566033915384886,-40.6268483631173,
-8.73670574475149));
#23145=CARTESIAN_POINT('Ctrl Pts',(-0.314738777667137,-43.2628954695717,
-11.3734544105136));
#23146=CARTESIAN_POINT('Ctrl Pts',(-0.193253748290479,-44.830540113301,
-12.4221714958367));
#23147=CARTESIAN_POINT('Ctrl Pts',(0.0623724159481334,-48.2896308975971,
-13.8545909095489));
#23148=CARTESIAN_POINT('Ctrl Pts',(0.183762141935159,-50.1389656602319,
-14.2195188100007));
#23149=CARTESIAN_POINT('Ctrl Pts',(0.309815399742839,-51.9999633043522,
-14.2201291128083));
#23150=CARTESIAN_POINT('Ctrl Pts',(-1.62853105321834,-40.1882694324258,
1.47327580984132));
#23151=CARTESIAN_POINT('Ctrl Pts',(-1.58693724130863,-40.1642011727047,
1.01591349030511));
#23152=CARTESIAN_POINT('Ctrl Pts',(-1.54343618780062,-40.1314061200099,
0.528588343875644));
#23153=CARTESIAN_POINT('Ctrl Pts',(-1.37533481599184,-40.1302905677455,
-1.55405138008459));
#23154=CARTESIAN_POINT('Ctrl Pts',(-1.25185544908537,-40.4394331428107,
-3.10057294640679));
#23155=CARTESIAN_POINT('Ctrl Pts',(-0.99949789152226,-41.6290225365179,
-5.982274843346));
#23156=CARTESIAN_POINT('Ctrl Pts',(-0.875863178863688,-42.5087254655101,
-7.29352824389351));
#23157=CARTESIAN_POINT('Ctrl Pts',(-0.625530141228115,-44.7059952341645,
-9.49167634236414));
#23158=CARTESIAN_POINT('Ctrl Pts',(-0.501895397273558,-46.0186144616128,
-10.369052486768));
#23159=CARTESIAN_POINT('Ctrl Pts',(-0.249537900122174,-48.8987303723102,
-11.5624766483463));
#23160=CARTESIAN_POINT('Ctrl Pts',(-0.125494944833563,-50.4521347865941,
-11.8682745705925));
#23161=CARTESIAN_POINT('Ctrl Pts',(-0.000622417322686238,-51.9999864962518,
-11.8690397849987));
#23162=CARTESIAN_POINT('Ctrl Pts',(-2.39089944281231,-42.4307892712954,
1.35541200298501));
#23163=CARTESIAN_POINT('Ctrl Pts',(-2.34812421168709,-42.4060373833274,
0.885058889676134));
#23164=CARTESIAN_POINT('Ctrl Pts',(-2.30592316845611,-42.3769809488797,
0.426408500609331));
#23165=CARTESIAN_POINT('Ctrl Pts',(-2.13948974646398,-42.3752988308948,
-1.2536423221009));
#23166=CARTESIAN_POINT('Ctrl Pts',(-2.01335948895663,-42.6291645083452,
-2.51864171288184));
#23167=CARTESIAN_POINT('Ctrl Pts',(-1.76412360301132,-43.5891580556313,
-4.84795915807201));
#23168=CARTESIAN_POINT('Ctrl Pts',(-1.63843584903307,-44.306048514286,-5.915170204659));
#23169=CARTESIAN_POINT('Ctrl Pts',(-1.38902165105132,-46.0841342086093,
-7.69457540340395));
#23170=CARTESIAN_POINT('Ctrl Pts',(-1.26333384857794,-47.1534076509294,
-8.40795287035375));
#23171=CARTESIAN_POINT('Ctrl Pts',(-1.01409805364826,-49.4803356664615,
-9.37372383743554));
#23172=CARTESIAN_POINT('Ctrl Pts',(-0.887523067773768,-50.7512717901712,
-9.62254086006318));
#23173=CARTESIAN_POINT('Ctrl Pts',(-0.763776277074748,-52.0000086453373,
-9.62369151535372));
#23174=CARTESIAN_POINT('Ctrl Pts',(-3.5767226147735,-44.4816940061638,1.2476816011619));
#23175=CARTESIAN_POINT('Ctrl Pts',(-3.53286976879601,-44.4563185563517,
0.765479118782407));
#23176=CARTESIAN_POINT('Ctrl Pts',(-3.49185481010397,-44.4306505608144,
0.332966318319628));
#23177=CARTESIAN_POINT('Ctrl Pts',(-3.32694672771567,-44.4280873491762,
-0.978922014648203));
#23178=CARTESIAN_POINT('Ctrl Pts',(-3.19839225347182,-44.6319588195941,
-1.98636136652616));
#23179=CARTESIAN_POINT('Ctrl Pts',(-2.95201108858767,-45.381365961698,-3.81078790535049));
#23180=CARTESIAN_POINT('Ctrl Pts',(-2.82444585837899,-45.9497454423789,
-4.65460264912874));
#23181=CARTESIAN_POINT('Ctrl Pts',(-2.5758719281337,-47.3443497895988,-6.05121512490362));
#23182=CARTESIAN_POINT('Ctrl Pts',(-2.44830662331528,-48.1913089840266,
-6.61423873300174));
#23183=CARTESIAN_POINT('Ctrl Pts',(-2.20192559708918,-50.0120953836876,
-7.37244739486218));
#23184=CARTESIAN_POINT('Ctrl Pts',(-2.07303718495312,-51.024880382195,-7.56862230180471));
#23185=CARTESIAN_POINT('Ctrl Pts',(-1.95031777657922,-52.0000289004077,
-7.57037421505985));
#23186=CARTESIAN_POINT('Ctrl Pts',(-6.55512420987408,-37.2260157227862,
0.));
#23187=CARTESIAN_POINT('Ctrl Pts',(-6.34301961518532,-37.2565117595591,
3.24562220582792));
#23188=CARTESIAN_POINT('Ctrl Pts',(-6.33132600607604,-38.680896818179,6.16982677025167));
#23189=CARTESIAN_POINT('Ctrl Pts',(-6.31963239696676,-40.1052818767989,
9.09403133467541));
#23190=CARTESIAN_POINT('Ctrl Pts',(-6.46865591986352,-42.6474791415621,
11.1176436806954));
#23191=CARTESIAN_POINT('Ctrl Pts',(-6.61767944276027,-45.1896764063252,
13.1412560267153));
#23192=CARTESIAN_POINT('Ctrl Pts',(-6.85589424502954,-48.3522126450341,
13.8634749112255));
#23193=CARTESIAN_POINT('Ctrl Pts',(-7.09410904729881,-51.514748883743,14.5856937957357));
#23194=CARTESIAN_POINT('Ctrl Pts',(-7.33232384956808,-54.6772851224519,
13.8634749112255));
#23195=CARTESIAN_POINT('Ctrl Pts',(-7.19674949232908,-39.5090640497073,
0.));
#23196=CARTESIAN_POINT('Ctrl Pts',(-6.9846448976403,-39.5395600864802,2.70899372698068));
#23197=CARTESIAN_POINT('Ctrl Pts',(-6.93981550268921,-40.7334806923574,
5.14971273833322));
#23198=CARTESIAN_POINT('Ctrl Pts',(-6.89498610773809,-41.9274012982346,
7.59043174968578));
#23199=CARTESIAN_POINT('Ctrl Pts',(-6.9843010077209,-44.0543159688391,9.2794617117575));
#23200=CARTESIAN_POINT('Ctrl Pts',(-7.07361590770374,-46.1812306394436,
10.9684916738292));
#23201=CARTESIAN_POINT('Ctrl Pts',(-7.23737527503327,-48.8259179534578,
11.5712994880388));
#23202=CARTESIAN_POINT('Ctrl Pts',(-7.40113464236278,-51.4706052674719,
12.1741073022483));
#23203=CARTESIAN_POINT('Ctrl Pts',(-7.56489400969232,-54.1152925814861,
11.5712994880388));
#23204=CARTESIAN_POINT('Ctrl Pts',(-8.27145263712698,-41.6230663715377,
0.));
#23205=CARTESIAN_POINT('Ctrl Pts',(-8.05934804243821,-41.6535624083105,
2.19648874705823));
#23206=CARTESIAN_POINT('Ctrl Pts',(-7.98287244172838,-42.627378818489,4.17545672685568));
#23207=CARTESIAN_POINT('Ctrl Pts',(-7.90639684101858,-43.6011952286675,
6.15442470665313));
#23208=CARTESIAN_POINT('Ctrl Pts',(-7.93868724864975,-45.3314958432333,
7.5239130403414));
#23209=CARTESIAN_POINT('Ctrl Pts',(-7.9709776562809,-47.0617964577992,8.89340137402966));
#23210=CARTESIAN_POINT('Ctrl Pts',(-8.06362864473556,-49.2119141333855,
9.3821661014496));
#23211=CARTESIAN_POINT('Ctrl Pts',(-8.15627963319022,-51.3620318089719,
9.87093082886953));
#23212=CARTESIAN_POINT('Ctrl Pts',(-8.24893062164489,-53.5121494845583,
9.3821661014496));
#23213=CARTESIAN_POINT('Ctrl Pts',(-9.7379322389713,-43.4867804707271,0.));
#23214=CARTESIAN_POINT('Ctrl Pts',(-9.52582764428252,-43.5172765074999,
1.72780310113342));
#23215=CARTESIAN_POINT('Ctrl Pts',(-9.42041159817581,-44.2898076986597,
3.28449990511991));
#23216=CARTESIAN_POINT('Ctrl Pts',(-9.31499555206908,-45.0623388898195,
4.84119670910639));
#23217=CARTESIAN_POINT('Ctrl Pts',(-9.29513707904857,-46.4299360725759,
5.91846432228297));
#23218=CARTESIAN_POINT('Ctrl Pts',(-9.27527860602804,-47.7975332553324,
6.99573193545956));
#23219=CARTESIAN_POINT('Ctrl Pts',(-9.30290100395336,-49.495367149254,7.38020429521638));
#23220=CARTESIAN_POINT('Ctrl Pts',(-9.33052340187867,-51.1932010431757,
7.76467665497321));
#23221=CARTESIAN_POINT('Ctrl Pts',(-9.35814579980399,-52.8910349370973,
7.38020429521638));
#23222=CARTESIAN_POINT('',(-6.55512420988052,-37.22601572281,1.57948858047412E-9));
#23223=CARTESIAN_POINT('Origin',(-23.8837944332598,-32.3559861244012,0.));
#23224=CARTESIAN_POINT('Ctrl Pts',(-6.55512420969261,-37.226015722898,3.13104709159877E-9));
#23225=CARTESIAN_POINT('Ctrl Pts',(-6.53911072623215,-37.2283181142836,
0.245038153335359));
#23226=CARTESIAN_POINT('Ctrl Pts',(-6.52385796555383,-37.2369141874759,
0.490791160521495));
#23227=CARTESIAN_POINT('Ctrl Pts',(-6.50940905124972,-37.2518844708665,
0.736766500725045));
#23228=CARTESIAN_POINT('Ctrl Pts',(-6.49500757191982,-37.2668056076575,
0.981934317700707));
#23229=CARTESIAN_POINT('Ctrl Pts',(-6.48140471121339,-37.2880592683071,
1.22732257376537));
#23230=CARTESIAN_POINT('Ctrl Pts',(-6.46863741161224,-37.3156748491109,
1.47243294816315));
#23231=CARTESIAN_POINT('Ctrl Pts',(-6.45588933999698,-37.343248839914,1.71717417802991));
#23232=CARTESIAN_POINT('Ctrl Pts',(-6.44397435004891,-37.3771656469145,
1.96163791541559));
#23233=CARTESIAN_POINT('Ctrl Pts',(-6.43292288824284,-37.4174031787122,
2.20532408778497));
#23234=CARTESIAN_POINT('Ctrl Pts',(-6.42188090473605,-37.457606200743,2.44880126242042));
#23235=CARTESIAN_POINT('Ctrl Pts',(-6.41170099625808,-37.5041190904231,
2.69150175431029));
#23236=CARTESIAN_POINT('Ctrl Pts',(-6.4024067347573,-37.5568683165634,2.93292951866791));
#23237=CARTESIAN_POINT('Ctrl Pts',(-6.39311441763456,-37.6096065074603,
3.17430677585578));
#23238=CARTESIAN_POINT('Ctrl Pts',(-6.38470739581513,-37.6685783420143,
3.41441139318338));
#23239=CARTESIAN_POINT('Ctrl Pts',(-6.37720208124067,-37.7336596075968,
3.65275710614636));
#23240=CARTESIAN_POINT('Ctrl Pts',(-6.36968723653768,-37.7988235123306,
3.89140546668784));
#23241=CARTESIAN_POINT('Ctrl Pts',(-6.36307640132128,-37.8701122336038,
4.12829002081156));
#23242=CARTESIAN_POINT('Ctrl Pts',(-6.35737866000311,-37.9473518840361,
4.36293874377797));
#23243=CARTESIAN_POINT('Ctrl Pts',(-6.35167510471667,-38.0246703497133,
4.59782690201429));
#23244=CARTESIAN_POINT('Ctrl Pts',(-6.34688650816463,-38.1079516890034,
4.83047425894932));
#23245=CARTESIAN_POINT('Ctrl Pts',(-6.34301449757132,-38.196974817961,5.06042975959396));
#23246=CARTESIAN_POINT('Ctrl Pts',(-6.33913116673682,-38.2862582156518,
5.29105755998276));
#23247=CARTESIAN_POINT('Ctrl Pts',(-6.33616978186108,-38.3813167726778,
5.51897736305666));
#23248=CARTESIAN_POINT('Ctrl Pts',(-6.33412450750884,-38.4818839849188,
5.74376259354316));
#23249=CARTESIAN_POINT('Ctrl Pts',(-6.33282037976348,-38.5460086299152,
5.88709234072609));
#23250=CARTESIAN_POINT('Ctrl Pts',(-6.33188856576809,-38.612372071261,6.02914825314187));
#23251=CARTESIAN_POINT('Ctrl Pts',(-6.33132600608609,-38.6808968182129,
6.16982677023484));
#23252=CARTESIAN_POINT('Ctrl Pts',(-6.33044389595582,-38.7883456372328,
6.39041482339097));
#23253=CARTESIAN_POINT('Ctrl Pts',(-6.33027613506487,-38.9017639334401,
6.60890054011818));
#23254=CARTESIAN_POINT('Ctrl Pts',(-6.33083419837773,-39.0210126661744,
6.82480412008061));
#23255=CARTESIAN_POINT('Ctrl Pts',(-6.33139100183133,-39.1399921882013,
7.04022028559308));
#23256=CARTESIAN_POINT('Ctrl Pts',(-6.33267037013978,-39.2647757598683,
7.25306552029648));
#23257=CARTESIAN_POINT('Ctrl Pts',(-6.33467799886863,-39.3951753232291,
7.46287566269424));
#23258=CARTESIAN_POINT('Ctrl Pts',(-6.33668239850791,-39.5253651506641,
7.67234834441885));
#23259=CARTESIAN_POINT('Ctrl Pts',(-6.33941272481299,-39.6611527651412,
7.87879526533028));
#23260=CARTESIAN_POINT('Ctrl Pts',(-6.34286879629103,-39.8023029910568,
8.08177334612192));
#23261=CARTESIAN_POINT('Ctrl Pts',(-6.34632155154412,-39.9433177782516,
8.28455666214124));
#23262=CARTESIAN_POINT('Ctrl Pts',(-6.35049865962759,-40.0896846778747,
8.48387739272885));
#23263=CARTESIAN_POINT('Ctrl Pts',(-6.35539404456574,-40.2411239605253,
8.67931873611141));
#23264=CARTESIAN_POINT('Ctrl Pts',(-6.36028966495896,-40.3925705270046,
8.87476947970524));
#23265=CARTESIAN_POINT('Ctrl Pts',(-6.36590362406253,-40.5490896991202,
9.06634009532846));
#23266=CARTESIAN_POINT('Ctrl Pts',(-6.37222400138258,-40.7103600297418,
9.25364450340987));
#23267=CARTESIAN_POINT('Ctrl Pts',(-6.37854669727067,-40.8716895207925,
9.44101762226479));
#23268=CARTESIAN_POINT('Ctrl Pts',(-6.38557631500248,-41.0377733398943,
9.62412107874998));
#23269=CARTESIAN_POINT('Ctrl Pts',(-6.39329523799166,-41.208252351997,9.80260437466072));
#23270=CARTESIAN_POINT('Ctrl Pts',(-6.40102675214305,-41.3790094506799,
9.98137881379636));
#23271=CARTESIAN_POINT('Ctrl Pts',(-6.40944980108705,-41.5541757364557,
10.1555177270921));
#23272=CARTESIAN_POINT('Ctrl Pts',(-6.41854124933288,-41.7333579204532,
10.3247095747706));
#23273=CARTESIAN_POINT('Ctrl Pts',(-6.421168985615,-41.7851476368183,10.3736117457737));
#23274=CARTESIAN_POINT('Ctrl Pts',(-6.42385252692466,-41.8372726564643,
10.4221009095723));
#23275=CARTESIAN_POINT('Ctrl Pts',(-6.42659123460866,-41.8897230480067,
10.4701702229062));
#23276=CARTESIAN_POINT('Ctrl Pts',(-2.90816428999286,-44.4687528548127,
0.));
#23277=CARTESIAN_POINT('Ctrl Pts',(-2.69605969530409,-44.4992488915856,
1.72780310113342));
#23278=CARTESIAN_POINT('Ctrl Pts',(-2.59064364919737,-45.2717800827454,
3.28449990511991));
#23279=CARTESIAN_POINT('Ctrl Pts',(-2.48522760309065,-46.0443112739052,
4.84119670910638));
#23280=CARTESIAN_POINT('Ctrl Pts',(-2.46536913007014,-47.4119084566616,
5.91846432228298));
#23281=CARTESIAN_POINT('Ctrl Pts',(-2.4455106570496,-48.779505639418,6.99573193545957));
#23282=CARTESIAN_POINT('Ctrl Pts',(-2.47313305497492,-50.4773395333397,
7.38020429521639));
#23283=CARTESIAN_POINT('Ctrl Pts',(-2.50075545290024,-52.1751734272613,
7.76467665497322));
#23284=CARTESIAN_POINT('Ctrl Pts',(-2.52837785082555,-53.873007321183,7.38020429521639));
#23285=CARTESIAN_POINT('Ctrl Pts',(-3.79017222552544,-42.2673772240308,
0.));
#23286=CARTESIAN_POINT('Ctrl Pts',(-3.57806763083667,-42.2978732608037,
2.19648874705823));
#23287=CARTESIAN_POINT('Ctrl Pts',(-3.50159203012685,-43.2716896709822,
4.17545672685568));
#23288=CARTESIAN_POINT('Ctrl Pts',(-3.42511642941705,-44.2455060811606,
6.15442470665314));
#23289=CARTESIAN_POINT('Ctrl Pts',(-3.4574068370482,-45.9758066957265,7.5239130403414));
#23290=CARTESIAN_POINT('Ctrl Pts',(-3.48969724467936,-47.7061073102924,
8.89340137402967));
#23291=CARTESIAN_POINT('Ctrl Pts',(-3.58234823313402,-49.8562249858787,
9.3821661014496));
#23292=CARTESIAN_POINT('Ctrl Pts',(-3.67499922158868,-52.006342661465,9.87093082886954));
#23293=CARTESIAN_POINT('Ctrl Pts',(-3.76765021004335,-54.1564603370514,
9.3821661014496));
#23294=CARTESIAN_POINT('Ctrl Pts',(-4.22575906238243,-39.9362279852004,
0.));
#23295=CARTESIAN_POINT('Ctrl Pts',(-4.01365446769365,-39.9667240219733,
2.70899372698068));
#23296=CARTESIAN_POINT('Ctrl Pts',(-3.96882507274256,-41.1606446278505,
5.14971273833322));
#23297=CARTESIAN_POINT('Ctrl Pts',(-3.92399567779144,-42.3545652337278,
7.59043174968577));
#23298=CARTESIAN_POINT('Ctrl Pts',(-4.01331057777426,-44.4814799043322,
9.2794617117575));
#23299=CARTESIAN_POINT('Ctrl Pts',(-4.10262547775709,-46.6083945749367,
10.9684916738292));
#23300=CARTESIAN_POINT('Ctrl Pts',(-4.26638484508662,-49.2530818889509,
11.5712994880388));
#23301=CARTESIAN_POINT('Ctrl Pts',(-4.43014421241612,-51.897769202965,12.1741073022483));
#23302=CARTESIAN_POINT('Ctrl Pts',(-4.59390357974567,-54.5424565169792,
11.5712994880388));
#23303=CARTESIAN_POINT('Ctrl Pts',(-4.19818497005538,-37.5648924257372,
0.));
#23304=CARTESIAN_POINT('Ctrl Pts',(-3.98608037536661,-37.59538846251,3.24562220582793));
#23305=CARTESIAN_POINT('Ctrl Pts',(-3.97438676625733,-39.0197735211299,
6.16982677025167));
#23306=CARTESIAN_POINT('Ctrl Pts',(-3.96269315714806,-40.4441585797499,
9.09403133467541));
#23307=CARTESIAN_POINT('Ctrl Pts',(-4.11171668004481,-42.986355844513,11.1176436806954));
#23308=CARTESIAN_POINT('Ctrl Pts',(-4.26074020294156,-45.5285531092762,
13.1412560267153));
#23309=CARTESIAN_POINT('Ctrl Pts',(-4.49895500521084,-48.6910893479851,
13.8634749112255));
#23310=CARTESIAN_POINT('Ctrl Pts',(-4.7371698074801,-51.853625586694,14.5856937957357));
#23311=CARTESIAN_POINT('Ctrl Pts',(-4.97538460974937,-55.0161618254029,
13.8634749112255));
#23312=CARTESIAN_POINT('',(-4.19818497005538,-37.5648924257372,0.));
#23313=CARTESIAN_POINT('Ctrl Pts',(-4.19818497005538,-37.5648924257372,
0.));
#23314=CARTESIAN_POINT('Ctrl Pts',(-3.98608037536661,-37.59538846251,3.24562220582793));
#23315=CARTESIAN_POINT('Ctrl Pts',(-3.97438676625733,-39.0197735211299,
6.16982677025167));
#23316=CARTESIAN_POINT('Ctrl Pts',(-3.96462449666041,-40.2089043379837,
8.61106394926975));
#23317=CARTESIAN_POINT('Ctrl Pts',(-4.06844583510776,-42.2054524109828,
10.4489096280657));
#23318=CARTESIAN_POINT('Origin',(13.8005982420124,-37.7741838134885,0.));
#23319=CARTESIAN_POINT('Ctrl Pts',(-4.19818497005538,-37.5648924257372,
0.));
#23320=CARTESIAN_POINT('Ctrl Pts',(-3.98608037536661,-37.59538846251,3.24562220582793));
#23321=CARTESIAN_POINT('Ctrl Pts',(-3.97438676625733,-39.0197735211299,
6.16982677025167));
#23322=CARTESIAN_POINT('Ctrl Pts',(-3.96269315714806,-40.4441585797499,
9.09403133467541));
#23323=CARTESIAN_POINT('Ctrl Pts',(-4.11171668004481,-42.986355844513,11.1176436806954));
#23324=CARTESIAN_POINT('Ctrl Pts',(-4.26074020294156,-45.5285531092762,
13.1412560267153));
#23325=CARTESIAN_POINT('Ctrl Pts',(-4.49895500521085,-48.6910893479851,
13.8634749112255));
#23326=CARTESIAN_POINT('Ctrl Pts',(-4.7371698074801,-51.853625586694,14.5856937957357));
#23327=CARTESIAN_POINT('Ctrl Pts',(-4.97538460974937,-55.0161618254029,
13.8634749112255));
#23328=CARTESIAN_POINT('Ctrl Pts',(-4.81560839388882,-36.8396419064669,
0.));
#23329=CARTESIAN_POINT('Ctrl Pts',(-4.60350379920004,-36.8701379432397,
3.38941559469373));
#23330=CARTESIAN_POINT('Ctrl Pts',(-4.60068915780633,-38.3562775787769,
6.44317352589573));
#23331=CARTESIAN_POINT('Ctrl Pts',(-4.59787451641258,-39.8424172143141,
9.49693145709774));
#23332=CARTESIAN_POINT('Ctrl Pts',(-4.76289738629099,-42.4958923815832,
11.6101975146502));
#23333=CARTESIAN_POINT('Ctrl Pts',(-4.92792025616937,-45.1493675488523,
13.7234635722027));
#23334=CARTESIAN_POINT('Ctrl Pts',(-5.18608591779754,-48.4506650623305,
14.4776794959001));
#23335=CARTESIAN_POINT('Ctrl Pts',(-5.44425157942571,-51.7519625758087,
15.2318954195974));
#23336=CARTESIAN_POINT('Ctrl Pts',(-5.70241724105386,-55.0532600892869,
14.4776794959001));
#23337=CARTESIAN_POINT('Ctrl Pts',(-5.7583840898163,-36.7040912252865,0.));
#23338=CARTESIAN_POINT('Ctrl Pts',(-5.54627949512753,-36.7345872620594,
3.38941559469373));
#23339=CARTESIAN_POINT('Ctrl Pts',(-5.54346485373381,-38.2207268975965,
6.44317352589573));
#23340=CARTESIAN_POINT('Ctrl Pts',(-5.54065021234007,-39.7068665331337,
9.49693145709774));
#23341=CARTESIAN_POINT('Ctrl Pts',(-5.70567308221847,-42.3603417004028,
11.6101975146502));
#23342=CARTESIAN_POINT('Ctrl Pts',(-5.87069595209686,-45.0138168676719,
13.7234635722027));
#23343=CARTESIAN_POINT('Ctrl Pts',(-6.12886161372502,-48.3151143811501,
14.4776794959001));
#23344=CARTESIAN_POINT('Ctrl Pts',(-6.3870272753532,-51.6164118946283,15.2318954195974));
#23345=CARTESIAN_POINT('Ctrl Pts',(-6.64519293698135,-54.9177094081065,
14.4776794959001));
#23346=CARTESIAN_POINT('Ctrl Pts',(-6.55512420987408,-37.2260157227862,
0.));
#23347=CARTESIAN_POINT('Ctrl Pts',(-6.34301961518532,-37.2565117595591,
3.24562220582792));
#23348=CARTESIAN_POINT('Ctrl Pts',(-6.33132600607604,-38.680896818179,6.16982677025167));
#23349=CARTESIAN_POINT('Ctrl Pts',(-6.31963239696676,-40.1052818767989,
9.09403133467541));
#23350=CARTESIAN_POINT('Ctrl Pts',(-6.46865591986352,-42.6474791415621,
11.1176436806954));
#23351=CARTESIAN_POINT('Ctrl Pts',(-6.61767944276027,-45.1896764063252,
13.1412560267153));
#23352=CARTESIAN_POINT('Ctrl Pts',(-6.85589424502954,-48.3522126450341,
13.8634749112255));
#23353=CARTESIAN_POINT('Ctrl Pts',(-7.0941090472988,-51.514748883743,14.5856937957357));
#23354=CARTESIAN_POINT('Ctrl Pts',(-7.33232384956808,-54.6772851224519,
13.8634749112255));
#23355=CARTESIAN_POINT('',(-5.31261783616131,-36.9500337175413,1.04083408558609E-14));
#23356=CARTESIAN_POINT('Origin',(-5.56877962163367,-38.7317130208009,1.04083408558608E-14));
#23357=CARTESIAN_POINT('Origin',(-5.56877962163367,-38.7317130208009,1.04083408558608E-14));
#23358=CARTESIAN_POINT('Ctrl Pts',(-11.7862169042733,-35.914217116421,0.));
#23359=CARTESIAN_POINT('Ctrl Pts',(-11.5806112670702,-35.9745883786013,
3.24562220582792));
#23360=CARTESIAN_POINT('Ctrl Pts',(-11.7717478112972,-37.3861394252073,
6.16982677025168));
#23361=CARTESIAN_POINT('Ctrl Pts',(-11.9628843555243,-38.7976904718134,
9.09403133467542));
#23362=CARTESIAN_POINT('Ctrl Pts',(-12.4721834264256,-41.2928035754071,
11.1176436806954));
#23363=CARTESIAN_POINT('Ctrl Pts',(-12.9814824973271,-43.7879166790007,
13.1412560267153));
#23364=CARTESIAN_POINT('Ctrl Pts',(-13.6673484497319,-46.884361357741,13.8634749112255));
#23365=CARTESIAN_POINT('Ctrl Pts',(-14.3532144021367,-49.9808060364813,
14.5856937957357));
#23366=CARTESIAN_POINT('Ctrl Pts',(-15.0390803545415,-53.0772507152216,
13.8634749112255));
#23367=CARTESIAN_POINT('Ctrl Pts',(-12.746223019916,-38.0827145049533,0.));
#23368=CARTESIAN_POINT('Ctrl Pts',(-12.5406173827129,-38.1430857671336,
2.70899372698069));
#23369=CARTESIAN_POINT('Ctrl Pts',(-12.6661569043003,-39.3312338708267,
5.14971273833323));
#23370=CARTESIAN_POINT('Ctrl Pts',(-12.7916964258877,-40.5193819745198,
7.59043174968578));
#23371=CARTESIAN_POINT('Ctrl Pts',(-13.1827937463383,-42.6119368849888,
9.27946171175752));
#23372=CARTESIAN_POINT('Ctrl Pts',(-13.5738910667889,-44.7044917954578,
10.9684916738293));
#23373=CARTESIAN_POINT('Ctrl Pts',(-14.1123618472579,-47.2989546180623,
11.5712994880388));
#23374=CARTESIAN_POINT('Ctrl Pts',(-14.6508326277268,-49.8934174406667,
12.1741073022483));
#23375=CARTESIAN_POINT('Ctrl Pts',(-15.1893034081958,-52.4878802632712,
11.5712994880388));
#23376=CARTESIAN_POINT('Ctrl Pts',(-14.1108411348345,-40.0222531270433,
0.));
#23377=CARTESIAN_POINT('Ctrl Pts',(-13.9052354976314,-40.0826243892237,
2.19648874705824));
#23378=CARTESIAN_POINT('Ctrl Pts',(-13.9681268331905,-41.0574123652206,
4.17545672685568));
#23379=CARTESIAN_POINT('Ctrl Pts',(-14.0310181687496,-42.0322003412177,
6.15442470665314));
#23380=CARTESIAN_POINT('Ctrl Pts',(-14.3092273587161,-43.7402935862749,
7.5239130403414));
#23381=CARTESIAN_POINT('Ctrl Pts',(-14.5874365486826,-45.4483868313322,
8.89340137402967));
#23382=CARTESIAN_POINT('Ctrl Pts',(-14.9851381329361,-47.563433798757,9.38216610144961));
#23383=CARTESIAN_POINT('Ctrl Pts',(-15.3828397171896,-49.6784807661818,
9.87093082886954));
#23384=CARTESIAN_POINT('Ctrl Pts',(-15.7805413014431,-51.7935277336065,
9.38216610144961));
#23385=CARTESIAN_POINT('Ctrl Pts',(-15.8276282594348,-41.6582954965892,
0.));
#23386=CARTESIAN_POINT('Ctrl Pts',(-15.6220226222317,-41.7186667587696,
1.72780310113343));
#23387=CARTESIAN_POINT('Ctrl Pts',(-15.6276222110079,-42.4983369638544,
3.28449990511991));
#23388=CARTESIAN_POINT('Ctrl Pts',(-15.6332217997841,-43.2780071689393,
4.84119670910638));
#23389=CARTESIAN_POINT('Ctrl Pts',(-15.8081948292724,-44.6345103396638,
5.91846432228298));
#23390=CARTESIAN_POINT('Ctrl Pts',(-15.9831678587607,-45.9910135103884,
6.99573193545956));
#23391=CARTESIAN_POINT('Ctrl Pts',(-16.2521360565317,-47.6676348262508,
7.38020429521639));
#23392=CARTESIAN_POINT('Ctrl Pts',(-16.5211042543027,-49.3442561421131,
7.76467665497322));
#23393=CARTESIAN_POINT('Ctrl Pts',(-16.7900724520737,-51.0208774579755,
7.38020429521639));
#23394=CARTESIAN_POINT('',(-11.7862169043636,-35.9142171164879,1.5794896091565E-9));
#23395=CARTESIAN_POINT('Origin',(-28.2454287759838,-28.6276304970125,0.));
#23396=CARTESIAN_POINT('Ctrl Pts',(-11.7862169041096,-35.9142171165575,
3.13105415629025E-9));
#23397=CARTESIAN_POINT('Ctrl Pts',(-11.7706940792789,-35.9187750292274,
0.245038153335357));
#23398=CARTESIAN_POINT('Ctrl Pts',(-11.7568199184777,-35.9294543009582,
0.490791160521484));
#23399=CARTESIAN_POINT('Ctrl Pts',(-11.7446485667473,-35.9463285033518,
0.736766500725023));
#23400=CARTESIAN_POINT('Ctrl Pts',(-11.732517172881,-35.9631473086865,0.981934317700669));
#23401=CARTESIAN_POINT('Ctrl Pts',(-11.7220774809609,-35.9861205266374,
1.22732257376532));
#23402=CARTESIAN_POINT('Ctrl Pts',(-11.7133702409767,-36.0152719968249,
1.47243294816308));
#23403=CARTESIAN_POINT('Ctrl Pts',(-11.704676114391,-36.0443795639103,1.71717417802986));
#23404=CARTESIAN_POINT('Ctrl Pts',(-11.6977092667636,-36.079646826587,1.96163791541557));
#23405=CARTESIAN_POINT('Ctrl Pts',(-11.6924966907341,-36.1210475853283,
2.20532408778498));
#23406=CARTESIAN_POINT('Ctrl Pts',(-11.6872885852766,-36.1624128366599,
2.44880126242047));
#23407=CARTESIAN_POINT('Ctrl Pts',(-11.6838317679612,-36.2099010442177,
2.69150175431038));
#23408=CARTESIAN_POINT('Ctrl Pts',(-11.6821391062285,-36.2634360706163,
2.93292951866803));
#23409=CARTESIAN_POINT('Ctrl Pts',(-11.6804467986039,-36.3169598973807,
3.17430677585587));
#23410=CARTESIAN_POINT('Ctrl Pts',(-11.6805179152419,-36.3765279276398,
3.41441139318343));
#23411=CARTESIAN_POINT('Ctrl Pts',(-11.6823510237341,-36.442014877408,3.65275710614637));
#23412=CARTESIAN_POINT('Ctrl Pts',(-11.6841864598781,-36.5075849814587,
3.89140546668792));
#23413=CARTESIAN_POINT('Ctrl Pts',(-11.6877883562709,-36.5790889062839,
4.12829002081172));
#23414=CARTESIAN_POINT('Ctrl Pts',(-11.6931409581034,-36.6563532415795,
4.3629387437782));
#23415=CARTESIAN_POINT('Ctrl Pts',(-11.6984990217243,-36.7336964173083,
4.59782690201463));
#23416=CARTESIAN_POINT('Ctrl Pts',(-11.7056113365129,-36.8168115609901,
4.83047425894977));
#23417=CARTESIAN_POINT('Ctrl Pts',(-11.7144480496046,-36.9054796074171,
5.06042975959451));
#23418=CARTESIAN_POINT('Ctrl Pts',(-11.7233105977815,-36.994406884455,5.29105755998321));
#23419=CARTESIAN_POINT('Ctrl Pts',(-11.7339075987035,-37.0889193314433,
5.51897736305701));
#23420=CARTESIAN_POINT('Ctrl Pts',(-11.7461953488408,-37.1887539873582,
5.7437625935434));
#23421=CARTESIAN_POINT('Ctrl Pts',(-11.7540303837175,-37.2524115326579,
5.88709234072625));
#23422=CARTESIAN_POINT('Ctrl Pts',(-11.7625525566674,-37.318232100817,6.02914825314195));
#23423=CARTESIAN_POINT('Ctrl Pts',(-11.771747811312,-37.3861394252394,6.16982677023483));
#23424=CARTESIAN_POINT('Ctrl Pts',(-11.7861662410924,-37.4926201075707,
6.39041482339093));
#23425=CARTESIAN_POINT('Ctrl Pts',(-11.8021412942474,-37.6049078439223,
6.60890054011811));
#23426=CARTESIAN_POINT('Ctrl Pts',(-11.8196645413938,-37.7228633758097,
6.82480412008051));
#23427=CARTESIAN_POINT('Ctrl Pts',(-11.8371482288262,-37.8405526164633,
7.04022028559307));
#23428=CARTESIAN_POINT('Ctrl Pts',(-11.8561731288309,-37.9638839982,7.25306552029657));
#23429=CARTESIAN_POINT('Ctrl Pts',(-11.8767181155647,-38.0926705666685,
7.46287566269442));
#23430=CARTESIAN_POINT('Ctrl Pts',(-11.897230057542,-38.2212499935681,7.67234834441907));
#23431=CARTESIAN_POINT('Ctrl Pts',(-11.9192571854559,-38.3552669199728,
7.87879526533054));
#23432=CARTESIAN_POINT('Ctrl Pts',(-11.9427658506829,-38.494488589857,8.08177334612222));
#23433=CARTESIAN_POINT('Ctrl Pts',(-11.9662519584997,-38.6335766715389,
8.28455666214102));
#23434=CARTESIAN_POINT('Ctrl Pts',(-11.9912167312942,-38.7778593027057,
8.48387739272812));
#23435=CARTESIAN_POINT('Ctrl Pts',(-12.0176143452908,-38.9270604659002,
8.6793187361102));
#23436=CARTESIAN_POINT('Ctrl Pts',(-12.0440132289428,-39.076268805276,8.87476947970396));
#23437=CARTESIAN_POINT('Ctrl Pts',(-12.0718450467037,-39.2303958882196,
9.06634009532711));
#23438=CARTESIAN_POINT('Ctrl Pts',(-12.1010522527165,-39.3891252359318,
9.25364450340846));
#23439=CARTESIAN_POINT('Ctrl Pts',(-12.1302701731047,-39.547912811939,9.44101762226378));
#23440=CARTESIAN_POINT('Ctrl Pts',(-12.1608644313192,-39.7113057183252,
9.62412107874935));
#23441=CARTESIAN_POINT('Ctrl Pts',(-12.1927664798385,-39.8789509826187,
9.80260437466046));
#23442=CARTESIAN_POINT('Ctrl Pts',(-12.2247205672069,-40.0468697110623,
9.98137881379621));
#23443=CARTESIAN_POINT('Ctrl Pts',(-12.2579866432888,-40.2190543317698,
10.1555177270921));
#23444=CARTESIAN_POINT('Ctrl Pts',(-12.2924858372373,-40.3951188515068,
10.3247095747706));
#23445=CARTESIAN_POINT('Ctrl Pts',(-12.3024572720617,-40.4460074573699,
10.3736117457737));
#23446=CARTESIAN_POINT('Ctrl Pts',(-12.3125316625311,-40.4972200117265,
10.4221009095723));
#23447=CARTESIAN_POINT('Ctrl Pts',(-12.3227069631095,-40.5487467751691,
10.4701702229062));
#23448=CARTESIAN_POINT('Ctrl Pts',(-9.20712674149475,-43.6022501387951,
0.));
#23449=CARTESIAN_POINT('Ctrl Pts',(-9.00152110429164,-43.6626214009754,
1.72780310113343));
#23450=CARTESIAN_POINT('Ctrl Pts',(-9.00712069306788,-44.4422916060603,
3.28449990511991));
#23451=CARTESIAN_POINT('Ctrl Pts',(-9.01272028184411,-45.2219618111451,
4.84119670910639));
#23452=CARTESIAN_POINT('Ctrl Pts',(-9.18769331133237,-46.5784649818697,
5.91846432228298));
#23453=CARTESIAN_POINT('Ctrl Pts',(-9.36266634082062,-47.9349681525942,
6.99573193545956));
#23454=CARTESIAN_POINT('Ctrl Pts',(-9.63163453859162,-49.6115894684566,
7.38020429521639));
#23455=CARTESIAN_POINT('Ctrl Pts',(-9.90060273636263,-51.288210784319,7.76467665497322));
#23456=CARTESIAN_POINT('Ctrl Pts',(-10.1695709341336,-52.9648321001814,
7.38020429521639));
#23457=CARTESIAN_POINT('Ctrl Pts',(-9.76686869112056,-41.297758521112,0.));
#23458=CARTESIAN_POINT('Ctrl Pts',(-9.56126305391744,-41.3581297832923,
2.19648874705824));
#23459=CARTESIAN_POINT('Ctrl Pts',(-9.62415438947656,-42.3329177592893,
4.17545672685568));
#23460=CARTESIAN_POINT('Ctrl Pts',(-9.68704572503569,-43.3077057352863,
6.15442470665314));
#23461=CARTESIAN_POINT('Ctrl Pts',(-9.96525491500219,-45.0157989803436,
7.5239130403414));
#23462=CARTESIAN_POINT('Ctrl Pts',(-10.2434641049687,-46.7238922254008,
8.89340137402967));
#23463=CARTESIAN_POINT('Ctrl Pts',(-10.6411656892222,-48.8389391928256,
9.38216610144961));
#23464=CARTESIAN_POINT('Ctrl Pts',(-11.0388672734757,-50.9539861602504,
9.87093082886954));
#23465=CARTESIAN_POINT('Ctrl Pts',(-11.4365688577292,-53.0690331276752,
9.38216610144961));
#23466=CARTESIAN_POINT('Ctrl Pts',(-9.86626475512766,-38.9283465500519,
0.));
#23467=CARTESIAN_POINT('Ctrl Pts',(-9.66065911792456,-38.9887178122322,
2.70899372698069));
#23468=CARTESIAN_POINT('Ctrl Pts',(-9.78619863951197,-40.1768659159253,
5.14971273833323));
#23469=CARTESIAN_POINT('Ctrl Pts',(-9.91173816109936,-41.3650140196185,
7.59043174968578));
#23470=CARTESIAN_POINT('Ctrl Pts',(-10.30283548155,-43.4575689300875,9.27946171175752));
#23471=CARTESIAN_POINT('Ctrl Pts',(-10.6939328020006,-45.5501238405564,
10.9684916738293));
#23472=CARTESIAN_POINT('Ctrl Pts',(-11.2324035824695,-48.1445866631609,
11.5712994880388));
#23473=CARTESIAN_POINT('Ctrl Pts',(-11.7708743629385,-50.7390494857654,
12.1741073022483));
#23474=CARTESIAN_POINT('Ctrl Pts',(-12.3093451434074,-53.3335123083699,
11.5712994880388));
#23475=CARTESIAN_POINT('Ctrl Pts',(-9.50149509066523,-36.5850719698905,
0.));
#23476=CARTESIAN_POINT('Ctrl Pts',(-9.29588945346213,-36.6454432320708,
3.24562220582793));
#23477=CARTESIAN_POINT('Ctrl Pts',(-9.48702599768917,-38.0569942786768,
6.16982677025168));
#23478=CARTESIAN_POINT('Ctrl Pts',(-9.67816254191622,-39.4685453252829,
9.09403133467541));
#23479=CARTESIAN_POINT('Ctrl Pts',(-10.1874616128176,-41.9636584288766,
11.1176436806954));
#23480=CARTESIAN_POINT('Ctrl Pts',(-10.696760683719,-44.4587715324702,13.1412560267153));
#23481=CARTESIAN_POINT('Ctrl Pts',(-11.3826266361238,-47.5552162112105,
13.8634749112255));
#23482=CARTESIAN_POINT('Ctrl Pts',(-12.0684925885286,-50.6516608899508,
14.5856937957357));
#23483=CARTESIAN_POINT('Ctrl Pts',(-12.7543585409334,-53.7481055686911,
13.8634749112255));
#23484=CARTESIAN_POINT('',(-9.50149509066523,-36.5850719698905,3.46944695195361E-15));
#23485=CARTESIAN_POINT('Ctrl Pts',(-9.50149509066523,-36.5850719698905,
3.46944695195361E-15));
#23486=CARTESIAN_POINT('Ctrl Pts',(-9.29588945346213,-36.6454432320708,
3.24562220582793));
#23487=CARTESIAN_POINT('Ctrl Pts',(-9.48702599768917,-38.0569942786769,
6.16982677025168));
#23488=CARTESIAN_POINT('Ctrl Pts',(-9.64659405380704,-39.235410774219,8.61106394926974));
#23489=CARTESIAN_POINT('Ctrl Pts',(-10.0334970568407,-41.1968615496291,
10.4489096280657));
#23490=CARTESIAN_POINT('Origin',(8.28430119040622,-39.3537269950291,0.));
#23491=CARTESIAN_POINT('Ctrl Pts',(-9.50149509066523,-36.5850719698905,
0.));
#23492=CARTESIAN_POINT('Ctrl Pts',(-9.29588945346213,-36.6454432320708,
3.24562220582793));
#23493=CARTESIAN_POINT('Ctrl Pts',(-9.48702599768917,-38.0569942786769,
6.16982677025168));
#23494=CARTESIAN_POINT('Ctrl Pts',(-9.67816254191622,-39.4685453252829,
9.0940313346754));
#23495=CARTESIAN_POINT('Ctrl Pts',(-10.1874616128176,-41.9636584288766,
11.1176436806954));
#23496=CARTESIAN_POINT('Ctrl Pts',(-10.696760683719,-44.4587715324702,13.1412560267153));
#23497=CARTESIAN_POINT('Ctrl Pts',(-11.3826266361238,-47.5552162112105,
13.8634749112255));
#23498=CARTESIAN_POINT('Ctrl Pts',(-12.0684925885286,-50.6516608899508,
14.5856937957357));
#23499=CARTESIAN_POINT('Ctrl Pts',(-12.7543585409334,-53.7481055686911,
13.8634749112255));
#23500=CARTESIAN_POINT('Ctrl Pts',(-10.0094201239375,-35.7793349404725,
0.));
#23501=CARTESIAN_POINT('Ctrl Pts',(-9.80381448673444,-35.8397062026528,
3.38941559469372));
#23502=CARTESIAN_POINT('Ctrl Pts',(-10.0125282162147,-37.3111196447714,
6.44317352589574));
#23503=CARTESIAN_POINT('Ctrl Pts',(-10.221241945695,-38.78253308689,9.49693145709774));
#23504=CARTESIAN_POINT('Ctrl Pts',(-10.7622140099934,-41.3855144999134,
11.6101975146502));
#23505=CARTESIAN_POINT('Ctrl Pts',(-11.3031860742919,-43.9884959129367,
13.7234635722027));
#23506=CARTESIAN_POINT('Ctrl Pts',(-12.0285476034514,-47.2194501734234,
14.4776794959001));
#23507=CARTESIAN_POINT('Ctrl Pts',(-12.753909132611,-50.45040443391,15.2318954195974));
#23508=CARTESIAN_POINT('Ctrl Pts',(-13.4792706617706,-53.6813586943966,
14.4776794959001));
#23509=CARTESIAN_POINT('Ctrl Pts',(-10.9233088493808,-35.5109929990847,
6.24500451351651E-15));
#23510=CARTESIAN_POINT('Ctrl Pts',(-10.7177032121776,-35.571364261265,3.38941559469372));
#23511=CARTESIAN_POINT('Ctrl Pts',(-10.9264169416579,-37.0427777033836,
6.44317352589573));
#23512=CARTESIAN_POINT('Ctrl Pts',(-11.1351306711382,-38.5141911455021,
9.49693145709774));
#23513=CARTESIAN_POINT('Ctrl Pts',(-11.6761027354366,-41.1171725585255,
11.6101975146502));
#23514=CARTESIAN_POINT('Ctrl Pts',(-12.2170747997351,-43.7201539715489,
13.7234635722027));
#23515=CARTESIAN_POINT('Ctrl Pts',(-12.9424363288947,-46.9511082320356,
14.4776794959001));
#23516=CARTESIAN_POINT('Ctrl Pts',(-13.6677978580543,-50.1820624925222,
15.2318954195974));
#23517=CARTESIAN_POINT('Ctrl Pts',(-14.3931593872138,-53.4130167530088,
14.4776794959001));
#23518=CARTESIAN_POINT('Ctrl Pts',(-11.7862169042733,-35.914217116421,0.));
#23519=CARTESIAN_POINT('Ctrl Pts',(-11.5806112670702,-35.9745883786013,
3.24562220582792));
#23520=CARTESIAN_POINT('Ctrl Pts',(-11.7717478112972,-37.3861394252073,
6.16982677025167));
#23521=CARTESIAN_POINT('Ctrl Pts',(-11.9628843555243,-38.7976904718134,
9.09403133467541));
#23522=CARTESIAN_POINT('Ctrl Pts',(-12.4721834264257,-41.2928035754071,
11.1176436806954));
#23523=CARTESIAN_POINT('Ctrl Pts',(-12.9814824973271,-43.7879166790007,
13.1412560267153));
#23524=CARTESIAN_POINT('Ctrl Pts',(-13.6673484497319,-46.884361357741,13.8634749112255));
#23525=CARTESIAN_POINT('Ctrl Pts',(-14.3532144021367,-49.9808060364813,
14.5856937957357));
#23526=CARTESIAN_POINT('Ctrl Pts',(-15.0390803545415,-53.0772507152216,
13.8634749112255));
#23527=CARTESIAN_POINT('',(-10.5170811194434,-35.8178713036885,1.00239475044027E-29));
#23528=CARTESIAN_POINT('Origin',(-11.0241949492052,-37.5449600575353,0.));
#23529=CARTESIAN_POINT('Origin',(-11.0241949492052,-37.5449600575353,0.));
#23530=CARTESIAN_POINT('Ctrl Pts',(-16.7773762111443,-33.8713086176152,
1.04083408558608E-14));
#23531=CARTESIAN_POINT('Ctrl Pts',(-16.5824550692826,-33.9603261204013,
3.24562220582793));
#23532=CARTESIAN_POINT('Ctrl Pts',(-16.9725307779978,-35.3303080462616,
6.16982677025167));
#23533=CARTESIAN_POINT('Ctrl Pts',(-17.362606486713,-36.700289972122,9.0940313346754));
#23534=CARTESIAN_POINT('Ctrl Pts',(-18.2218132452327,-39.097525607069,11.1176436806954));
#23535=CARTESIAN_POINT('Ctrl Pts',(-19.0810200037525,-41.4947612420161,
13.1412560267153));
#23536=CARTESIAN_POINT('Ctrl Pts',(-20.2005748533759,-44.4620796765377,
13.8634749112255));
#23537=CARTESIAN_POINT('Ctrl Pts',(-21.3201297029994,-47.4293981110593,
14.5856937957357));
#23538=CARTESIAN_POINT('Ctrl Pts',(-22.4396845526228,-50.3967165455809,
13.8634749112255));
#23539=CARTESIAN_POINT('Ctrl Pts',(-18.0362202038893,-35.8811107143582,
0.));
#23540=CARTESIAN_POINT('Ctrl Pts',(-17.8412990620276,-35.9701282171443,
2.70899372698069));
#23541=CARTESIAN_POINT('Ctrl Pts',(-18.1346518775201,-37.1283165495983,
5.14971273833323));
#23542=CARTESIAN_POINT('Ctrl Pts',(-18.4280046930126,-38.2865048820523,
7.59043174968578));
#23543=CARTESIAN_POINT('Ctrl Pts',(-19.1129228203181,-40.3021016488387,
9.27946171175752));
#23544=CARTESIAN_POINT('Ctrl Pts',(-19.7978409476237,-42.3176984156251,
10.9684916738293));
#23545=CARTESIAN_POINT('Ctrl Pts',(-20.7000614289633,-44.8091209655646,
11.5712994880388));
#23546=CARTESIAN_POINT('Ctrl Pts',(-21.6022819103028,-47.3005435155041,
12.1741073022483));
#23547=CARTESIAN_POINT('Ctrl Pts',(-22.5045023916423,-49.7919660654436,
11.5712994880388));
#23548=CARTESIAN_POINT('Ctrl Pts',(-19.6629735993423,-37.6067022235297,
0.));
#23549=CARTESIAN_POINT('Ctrl Pts',(-19.4680524574806,-37.6957197263158,
2.19648874705823));
#23550=CARTESIAN_POINT('Ctrl Pts',(-19.6690304430803,-38.6516353959965,
4.17545672685568));
#23551=CARTESIAN_POINT('Ctrl Pts',(-19.87000842868,-39.6075510656772,6.15442470665313));
#23552=CARTESIAN_POINT('Ctrl Pts',(-20.3884728641632,-41.2586650884906,
7.5239130403414));
#23553=CARTESIAN_POINT('Ctrl Pts',(-20.9069372996464,-42.909779111304,8.89340137402967));
#23554=CARTESIAN_POINT('Ctrl Pts',(-21.60159342232,-44.9466991136023,9.3821661014496));
#23555=CARTESIAN_POINT('Ctrl Pts',(-22.2962495449936,-46.9836191159005,
9.87093082886953));
#23556=CARTESIAN_POINT('Ctrl Pts',(-22.9909056676672,-49.0205391181987,
9.3821661014496));
#23557=CARTESIAN_POINT('Ctrl Pts',(-21.595119411647,-38.9817677587448,0.));
#23558=CARTESIAN_POINT('Ctrl Pts',(-21.4001982697853,-39.0707852615309,
1.72780310113343));
#23559=CARTESIAN_POINT('Ctrl Pts',(-21.5166995019649,-39.8417226435485,
3.28449990511991));
#23560=CARTESIAN_POINT('Ctrl Pts',(-21.6332007341444,-40.6126600255661,
4.84119670910639));
#23561=CARTESIAN_POINT('Ctrl Pts',(-21.9994433198417,-41.930454691535,5.91846432228297));
#23562=CARTESIAN_POINT('Ctrl Pts',(-22.3656859055389,-43.2482493575038,
6.99573193545956));
#23563=CARTESIAN_POINT('Ctrl Pts',(-22.8705244862892,-44.8695269202926,
7.38020429521639));
#23564=CARTESIAN_POINT('Ctrl Pts',(-23.3753630670395,-46.4908044830813,
7.76467665497322));
#23565=CARTESIAN_POINT('Ctrl Pts',(-23.8802016477898,-48.1120820458701,
7.38020429521639));
#23566=CARTESIAN_POINT('',(-16.7773762107575,-33.8713086176117,-2.44187790973619E-9));
#23567=CARTESIAN_POINT('Origin',(-32.0320676419192,-24.3164988679737,0.));
#23568=CARTESIAN_POINT('Ctrl Pts',(-16.7773762111443,-33.8713086176152,
1.04083408558608E-14));
#23569=CARTESIAN_POINT('Ctrl Pts',(-16.5824550692826,-33.9603261204013,
3.24562220582793));
#23570=CARTESIAN_POINT('Ctrl Pts',(-16.9725307779978,-35.3303080462616,
6.16982677025167));
#23571=CARTESIAN_POINT('Ctrl Pts',(-17.3001355482564,-36.4808862649314,
8.62571762198518));
#23572=CARTESIAN_POINT('Ctrl Pts',(-17.9679679135938,-38.3823149509186,
10.4701702229062));
#23573=CARTESIAN_POINT('Ctrl Pts',(-15.3186586437008,-41.8481313484578,
0.));
#23574=CARTESIAN_POINT('Ctrl Pts',(-15.1237375018391,-41.9371488512439,
1.72780310113342));
#23575=CARTESIAN_POINT('Ctrl Pts',(-15.2402387340187,-42.7080862332615,
3.28449990511991));
#23576=CARTESIAN_POINT('Ctrl Pts',(-15.3567399661983,-43.4790236152791,
4.84119670910639));
#23577=CARTESIAN_POINT('Ctrl Pts',(-15.7229825518955,-44.796818281248,5.91846432228298));
#23578=CARTESIAN_POINT('Ctrl Pts',(-16.0892251375927,-46.1146129472168,
6.99573193545956));
#23579=CARTESIAN_POINT('Ctrl Pts',(-16.594063718343,-47.7358905100056,7.38020429521639));
#23580=CARTESIAN_POINT('Ctrl Pts',(-17.0989022990933,-49.3571680727943,
7.76467665497322));
#23581=CARTESIAN_POINT('Ctrl Pts',(-17.6037408798436,-50.9784456355831,
7.38020429521639));
#23582=CARTESIAN_POINT('Ctrl Pts',(-15.5447398754879,-39.4874365476044,
0.));
#23583=CARTESIAN_POINT('Ctrl Pts',(-15.3498187336262,-39.5764540503905,
2.19648874705823));
#23584=CARTESIAN_POINT('Ctrl Pts',(-15.5507967192259,-40.5323697200712,
4.17545672685568));
#23585=CARTESIAN_POINT('Ctrl Pts',(-15.7517747048257,-41.4882853897519,
6.15442470665314));
#23586=CARTESIAN_POINT('Ctrl Pts',(-16.2702391403089,-43.1393994125653,
7.5239130403414));
#23587=CARTESIAN_POINT('Ctrl Pts',(-16.788703575792,-44.7905134353787,8.89340137402967));
#23588=CARTESIAN_POINT('Ctrl Pts',(-17.4833596984656,-46.8274334376769,
9.3821661014496));
#23589=CARTESIAN_POINT('Ctrl Pts',(-18.1780158211392,-48.8643534399752,
9.87093082886954));
#23590=CARTESIAN_POINT('Ctrl Pts',(-18.8726719438128,-50.9012734422734,
9.3821661014496));
#23591=CARTESIAN_POINT('Ctrl Pts',(-15.3059217494165,-37.1279962392256,
0.));
#23592=CARTESIAN_POINT('Ctrl Pts',(-15.1110006075549,-37.2170137420117,
2.70899372698069));
#23593=CARTESIAN_POINT('Ctrl Pts',(-15.4043534230473,-38.3752020744657,
5.14971273833323));
#23594=CARTESIAN_POINT('Ctrl Pts',(-15.6977062385398,-39.5333904069197,
7.59043174968577));
#23595=CARTESIAN_POINT('Ctrl Pts',(-16.3826243658454,-41.5489871737062,
9.27946171175751));
#23596=CARTESIAN_POINT('Ctrl Pts',(-17.0675424931509,-43.5645839404925,
10.9684916738293));
#23597=CARTESIAN_POINT('Ctrl Pts',(-17.9697629744905,-46.0560064904321,
11.5712994880388));
#23598=CARTESIAN_POINT('Ctrl Pts',(-18.87198345583,-48.5474290403715,12.1741073022483));
#23599=CARTESIAN_POINT('Ctrl Pts',(-19.7742039371695,-51.038851590311,11.5712994880388));
#23600=CARTESIAN_POINT('Ctrl Pts',(-14.6113821712783,-34.8604849513723,
1.04083408558608E-14));
#23601=CARTESIAN_POINT('Ctrl Pts',(-14.4164610294167,-34.9495024541584,
3.24562220582793));
#23602=CARTESIAN_POINT('Ctrl Pts',(-14.8065367381318,-36.3194843800187,
6.16982677025167));
#23603=CARTESIAN_POINT('Ctrl Pts',(-15.196612446847,-37.6894663058791,9.09403133467541));
#23604=CARTESIAN_POINT('Ctrl Pts',(-16.0558192053667,-40.0867019408261,
11.1176436806954));
#23605=CARTESIAN_POINT('Ctrl Pts',(-16.9150259638865,-42.4839375757732,
13.1412560267153));
#23606=CARTESIAN_POINT('Ctrl Pts',(-18.0345808135099,-45.4512560102948,
13.8634749112255));
#23607=CARTESIAN_POINT('Ctrl Pts',(-19.1541356631334,-48.4185744448164,
14.5856937957357));
#23608=CARTESIAN_POINT('Ctrl Pts',(-20.2736905127569,-51.385892879338,13.8634749112255));
#23609=CARTESIAN_POINT('',(-14.6113821712783,-34.8604849513723,1.04083408558608E-14));
#23610=CARTESIAN_POINT('Ctrl Pts',(-14.6113821712783,-34.8604849513723,
1.04083408558608E-14));
#23611=CARTESIAN_POINT('Ctrl Pts',(-14.4164610294167,-34.9495024541584,
3.24562220582793));
#23612=CARTESIAN_POINT('Ctrl Pts',(-14.8065367381318,-36.3194843800187,
6.16982677025167));
#23613=CARTESIAN_POINT('Ctrl Pts',(-15.1321867744982,-37.4631973926725,
8.61106394926976));
#23614=CARTESIAN_POINT('Ctrl Pts',(-15.7942952127126,-39.3496213890633,
10.4489096280657));
#23615=CARTESIAN_POINT('Origin',(2.59935965651522,-40.1321417817282,0.));
#23616=CARTESIAN_POINT('Ctrl Pts',(-14.6113821712783,-34.8604849513723,
1.04083408558608E-14));
#23617=CARTESIAN_POINT('Ctrl Pts',(-14.4164610294167,-34.9495024541584,
3.24562220582793));
#23618=CARTESIAN_POINT('Ctrl Pts',(-14.8065367381318,-36.3194843800187,
6.16982677025167));
#23619=CARTESIAN_POINT('Ctrl Pts',(-15.196612446847,-37.6894663058791,9.09403133467541));
#23620=CARTESIAN_POINT('Ctrl Pts',(-16.0558192053667,-40.0867019408261,
11.1176436806954));
#23621=CARTESIAN_POINT('Ctrl Pts',(-16.9150259638865,-42.4839375757732,
13.1412560267153));
#23622=CARTESIAN_POINT('Ctrl Pts',(-18.0345808135099,-45.4512560102947,
13.8634749112255));
#23623=CARTESIAN_POINT('Ctrl Pts',(-19.1541356631334,-48.4185744448164,
14.5856937957357));
#23624=CARTESIAN_POINT('Ctrl Pts',(-20.2736905127569,-51.385892879338,13.8634749112255));
#23625=CARTESIAN_POINT('Ctrl Pts',(-14.9994689250469,-33.9906638941718,
0.));
#23626=CARTESIAN_POINT('Ctrl Pts',(-14.8045477831852,-34.0796813969579,
3.38941559469372));
#23627=CARTESIAN_POINT('Ctrl Pts',(-15.220541073888,-35.5064149111823,6.44317352589573));
#23628=CARTESIAN_POINT('Ctrl Pts',(-15.6365343645908,-36.9331484254067,
9.49693145709774));
#23629=CARTESIAN_POINT('Ctrl Pts',(-16.5424429921147,-39.4326468889938,
11.6101975146502));
#23630=CARTESIAN_POINT('Ctrl Pts',(-17.4483516196387,-41.9321453525809,
13.7234635722027));
#23631=CARTESIAN_POINT('Ctrl Pts',(-18.626142747366,-45.0269834486351,14.4776794959001));
#23632=CARTESIAN_POINT('Ctrl Pts',(-19.8039338750932,-48.1218215446893,
15.2318954195974));
#23633=CARTESIAN_POINT('Ctrl Pts',(-20.9817250028204,-51.2166596407435,
14.4776794959001));
#23634=CARTESIAN_POINT('Ctrl Pts',(-15.8658665409933,-33.594993360669,0.));
#23635=CARTESIAN_POINT('Ctrl Pts',(-15.6709453991316,-33.6840108634551,
3.38941559469372));
#23636=CARTESIAN_POINT('Ctrl Pts',(-16.0869386898344,-35.1107443776795,
6.44317352589574));
#23637=CARTESIAN_POINT('Ctrl Pts',(-16.5029319805371,-36.5374778919039,
9.49693145709774));
#23638=CARTESIAN_POINT('Ctrl Pts',(-17.4088406080611,-39.036976355491,11.6101975146502));
#23639=CARTESIAN_POINT('Ctrl Pts',(-18.3147492355851,-41.536474819078,13.7234635722027));
#23640=CARTESIAN_POINT('Ctrl Pts',(-19.4925403633123,-44.6313129151322,
14.4776794959001));
#23641=CARTESIAN_POINT('Ctrl Pts',(-20.6703314910396,-47.7261510111864,
15.2318954195974));
#23642=CARTESIAN_POINT('Ctrl Pts',(-21.8481226187668,-50.8209891072406,
14.4776794959001));
#23643=CARTESIAN_POINT('Ctrl Pts',(-16.7773762111443,-33.8713086176152,
1.04083408558608E-14));
#23644=CARTESIAN_POINT('Ctrl Pts',(-16.5824550692826,-33.9603261204013,
3.24562220582793));
#23645=CARTESIAN_POINT('Ctrl Pts',(-16.9725307779978,-35.3303080462616,
6.16982677025167));
#23646=CARTESIAN_POINT('Ctrl Pts',(-17.362606486713,-36.700289972122,9.0940313346754));
#23647=CARTESIAN_POINT('Ctrl Pts',(-18.2218132452327,-39.097525607069,11.1176436806954));
#23648=CARTESIAN_POINT('Ctrl Pts',(-19.0810200037525,-41.4947612420161,
13.1412560267153));
#23649=CARTESIAN_POINT('Ctrl Pts',(-20.2005748533759,-44.4620796765377,
13.8634749112255));
#23650=CARTESIAN_POINT('Ctrl Pts',(-21.3201297029994,-47.4293981110593,
14.5856937957357));
#23651=CARTESIAN_POINT('Ctrl Pts',(-22.4396845526228,-50.3967165455809,
13.8634749112255));
#23652=CARTESIAN_POINT('',(-15.5074469599351,-33.9565603202878,7.60754902664041E-30));
#23653=CARTESIAN_POINT('Origin',(-16.2551894587639,-35.5938999782223,0.));
#23654=CARTESIAN_POINT('Origin',(-16.2551894587639,-35.5938999782223,0.));
#23655=CARTESIAN_POINT('Ctrl Pts',(-21.4269965203142,-31.1388779521429,
0.));
#23656=CARTESIAN_POINT('Ctrl Pts',(-21.246727906136,-31.2547295558833,3.24562220582792));
#23657=CARTESIAN_POINT('Ctrl Pts',(-21.8278019627954,-32.5552534796891,
6.16982677025168));
#23658=CARTESIAN_POINT('Ctrl Pts',(-22.4088760194547,-33.8557774034949,
9.09403133467542));
#23659=CARTESIAN_POINT('Ctrl Pts',(-23.600499493737,-36.1063347653245,11.1176436806954));
#23660=CARTESIAN_POINT('Ctrl Pts',(-24.7921229680193,-38.356892127154,13.1412560267153));
#23661=CARTESIAN_POINT('Ctrl Pts',(-26.3225758066526,-41.1346782711698,
13.8634749112255));
#23662=CARTESIAN_POINT('Ctrl Pts',(-27.853028645286,-43.9124644151856,14.5856937957357));
#23663=CARTESIAN_POINT('Ctrl Pts',(-29.3834814839194,-46.6902505592015,
13.8634749112255));
#23664=CARTESIAN_POINT('Ctrl Pts',(-22.9590519566755,-32.9490709821975,
0.));
#23665=CARTESIAN_POINT('Ctrl Pts',(-22.7787833424974,-33.064922585938,2.7089937269807));
#23666=CARTESIAN_POINT('Ctrl Pts',(-23.2339776345312,-34.1695737726435,
5.14971273833323));
#23667=CARTESIAN_POINT('Ctrl Pts',(-23.689171926565,-35.2742249593489,7.59043174968578));
#23668=CARTESIAN_POINT('Ctrl Pts',(-24.6539679027943,-37.1718318447821,
9.27946171175752));
#23669=CARTESIAN_POINT('Ctrl Pts',(-25.6187638790236,-39.0694387302152,
10.9684916738293));
#23670=CARTESIAN_POINT('Ctrl Pts',(-26.8663674540227,-41.4071028290423,
11.5712994880388));
#23671=CARTESIAN_POINT('Ctrl Pts',(-28.1139710290218,-43.7447669278694,
12.1741073022483));
#23672=CARTESIAN_POINT('Ctrl Pts',(-29.3615746040208,-46.0824310266965,
11.5712994880388));
#23673=CARTESIAN_POINT('Ctrl Pts',(-24.814824624701,-34.4255873115188,0.));
#23674=CARTESIAN_POINT('Ctrl Pts',(-24.6345560105229,-34.5414389152593,
2.19648874705823));
#23675=CARTESIAN_POINT('Ctrl Pts',(-24.969529313949,-35.4590225922221,4.17545672685568));
#23676=CARTESIAN_POINT('Ctrl Pts',(-25.3045026173751,-36.3766062691848,
6.15442470665313));
#23677=CARTESIAN_POINT('Ctrl Pts',(-26.0526678575965,-37.9371291496696,
7.5239130403414));
#23678=CARTESIAN_POINT('Ctrl Pts',(-26.8008330978179,-39.4976520301544,
8.89340137402968));
#23679=CARTESIAN_POINT('Ctrl Pts',(-27.7783025634768,-41.4149792500715,
9.3821661014496));
#23680=CARTESIAN_POINT('Ctrl Pts',(-28.7557720291356,-43.3323064699886,
9.87093082886954));
#23681=CARTESIAN_POINT('Ctrl Pts',(-29.7332414947946,-45.2496336899057,
9.3821661014496));
#23682=CARTESIAN_POINT('Ctrl Pts',(-26.9229962078199,-35.5116836434676,
0.));
#23683=CARTESIAN_POINT('Ctrl Pts',(-26.7427275936418,-35.6275352472081,
1.72780310113343));
#23684=CARTESIAN_POINT('Ctrl Pts',(-26.9677588400993,-36.3740457442604,
3.28449990511992));
#23685=CARTESIAN_POINT('Ctrl Pts',(-27.1927900865569,-37.1205562413127,
4.84119670910638));
#23686=CARTESIAN_POINT('Ctrl Pts',(-27.7428465855746,-38.3728159033327,
5.91846432228298));
#23687=CARTESIAN_POINT('Ctrl Pts',(-28.2929030845924,-39.6250755653527,
6.99573193545956));
#23688=CARTESIAN_POINT('Ctrl Pts',(-29.0233349906522,-41.1580048392678,
7.38020429521639));
#23689=CARTESIAN_POINT('Ctrl Pts',(-29.753766896712,-42.690934113183,7.76467665497321));
#23690=CARTESIAN_POINT('Ctrl Pts',(-30.4841988027718,-44.2238633870982,
7.38020429521638));
#23691=CARTESIAN_POINT('',(-21.4269965203187,-31.1388779521589,1.57949798001058E-9));
#23692=CARTESIAN_POINT('Origin',(-35.1666259835202,-19.5103534449751,0.));
#23693=CARTESIAN_POINT('Ctrl Pts',(-21.4269965201955,-31.1388779523199,
3.13107077675564E-9));
#23694=CARTESIAN_POINT('Ctrl Pts',(-21.4133865912302,-31.14762452263,0.245038153335643));
#23695=CARTESIAN_POINT('Ctrl Pts',(-21.4030831299566,-31.1617800116156,
0.49079116052204));
#23696=CARTESIAN_POINT('Ctrl Pts',(-21.3961588156768,-31.1813997562909,
0.736766500725851));
#23697=CARTESIAN_POINT('Ctrl Pts',(-21.389257233532,-31.2009550904461,0.981934317701482));
#23698=CARTESIAN_POINT('Ctrl Pts',(-21.3857127259201,-31.2259389327486,
1.22732257376611));
#23699=CARTESIAN_POINT('Ctrl Pts',(-21.3855711085673,-31.2563626765479,
1.47243294816386));
#23700=CARTESIAN_POINT('Ctrl Pts',(-21.385429704495,-31.2867406011578,1.71717417803062));
#23701=CARTESIAN_POINT('Ctrl Pts',(-21.388680999235,-31.3225420796899,1.96163791541631));
#23702=CARTESIAN_POINT('Ctrl Pts',(-21.3953435107757,-31.363734369177,2.2053240877857));
#23703=CARTESIAN_POINT('Ctrl Pts',(-21.4020003082054,-31.4048913300483,
2.4488012624211));
#23704=CARTESIAN_POINT('Ctrl Pts',(-21.4120624904153,-31.4514298295104,
2.69150175431092));
#23705=CARTESIAN_POINT('Ctrl Pts',(-21.4255209532439,-31.5032731891,2.93292951866849));
#23706=CARTESIAN_POINT('Ctrl Pts',(-21.4389766005352,-31.5551057029553,
3.17430677585639));
#23707=CARTESIAN_POINT('Ctrl Pts',(-21.4558270899206,-31.6122407735689,
3.41441139318401));
#23708=CARTESIAN_POINT('Ctrl Pts',(-21.4760357504366,-31.6745585953924,
3.65275710614701));
#23709=CARTESIAN_POINT('Ctrl Pts',(-21.4962700715869,-31.7369555473905,
3.89140546668857));
#23710=CARTESIAN_POINT('Ctrl Pts',(-21.5198710494326,-31.8045482893659,
4.12829002081237));
#23711=CARTESIAN_POINT('Ctrl Pts',(-21.546774712017,-31.877174873993,4.36293874377885));
#23712=CARTESIAN_POINT('Ctrl Pts',(-21.5737058270658,-31.9498755666981,
4.5978269020151));
#23713=CARTESIAN_POINT('Ctrl Pts',(-21.6039462850732,-32.0276201924313,
4.83047425895007));
#23714=CARTESIAN_POINT('Ctrl Pts',(-21.6374057246246,-32.1102069701887,
5.06042975959465));
#23715=CARTESIAN_POINT('Ctrl Pts',(-21.6709629864615,-32.1930351993112,
5.29105755998335));
#23716=CARTESIAN_POINT('Ctrl Pts',(-21.7077579677309,-32.280733707951,5.51897736305714));
#23717=CARTESIAN_POINT('Ctrl Pts',(-21.7476746505214,-32.3730624995606,
5.74376259354354));
#23718=CARTESIAN_POINT('Ctrl Pts',(-21.7731267144332,-32.4319340825843,
5.88709234072634));
#23719=CARTESIAN_POINT('Ctrl Pts',(-21.7998474764587,-32.4926874816773,
6.029148253142));
#23720=CARTESIAN_POINT('Ctrl Pts',(-21.8278019628186,-32.5552534797158,
6.16982677023484));
#23721=CARTESIAN_POINT('Ctrl Pts',(-21.8716354197709,-32.6533588051506,
6.39041482339092));
#23722=CARTESIAN_POINT('Ctrl Pts',(-21.9185984820905,-32.756597406632,6.60890054011809));
#23723=CARTESIAN_POINT('Ctrl Pts',(-21.9686438281945,-32.8648380414542,
6.82480412008047));
#23724=CARTESIAN_POINT('Ctrl Pts',(-22.0185761941209,-32.972834316968,7.04022028559303));
#23725=CARTESIAN_POINT('Ctrl Pts',(-22.0715769175146,-33.0858099774485,
7.25306552029652));
#23726=CARTESIAN_POINT('Ctrl Pts',(-22.1275730571501,-33.2035915933472,
7.46287566269437));
#23727=CARTESIAN_POINT('Ctrl Pts',(-22.1834791320502,-33.3211837681497,
7.67234834441909));
#23728=CARTESIAN_POINT('Ctrl Pts',(-22.2423709378485,-33.4435663083135,
7.87879526533063));
#23729=CARTESIAN_POINT('Ctrl Pts',(-22.3041506139772,-33.5705253659799,
8.08177334612238));
#23730=CARTESIAN_POINT('Ctrl Pts',(-22.3658710102834,-33.6973626018617,
8.28455666214124));
#23731=CARTESIAN_POINT('Ctrl Pts',(-22.430473648954,-33.8287673834107,8.4838773927284));
#23732=CARTESIAN_POINT('Ctrl Pts',(-22.4978367992944,-33.9644877838652,
8.67931873611054));
#23733=CARTESIAN_POINT('Ctrl Pts',(-22.5652031896243,-34.1002147121119,
8.87476947970437));
#23734=CARTESIAN_POINT('Ctrl Pts',(-22.635330240365,-34.2402574360607,9.0663400953276));
#23735=CARTESIAN_POINT('Ctrl Pts',(-22.70807357429,-34.3843285090689,9.25364450340901));
#23736=CARTESIAN_POINT('Ctrl Pts',(-22.7808435933891,-34.5284524331283,
9.44101762226399));
#23737=CARTESIAN_POINT('Ctrl Pts',(-22.8562316704646,-34.6766073801526,
9.62412107874924));
#23738=CARTESIAN_POINT('Ctrl Pts',(-22.9340725908145,-34.8284739876038,
9.80260437466002));
#23739=CARTESIAN_POINT('Ctrl Pts',(-23.0120404858285,-34.9805883209477,
9.98137881379545));
#23740=CARTESIAN_POINT('Ctrl Pts',(-23.0924690655294,-35.13642611801,10.155517727091));
#23741=CARTESIAN_POINT('Ctrl Pts',(-23.1751739070328,-35.2956392414801,
10.3247095747693));
#23742=CARTESIAN_POINT('Ctrl Pts',(-23.1990784057277,-35.3416572234148,
10.3736117457728));
#23743=CARTESIAN_POINT('Ctrl Pts',(-23.223172956478,-35.3879570256956,10.4221009095719));
#23744=CARTESIAN_POINT('Ctrl Pts',(-23.2474528526981,-35.4345298797237,
10.4701702229062));
#23745=CARTESIAN_POINT('Ctrl Pts',(-21.1183468312847,-39.2421052839112,
0.));
#23746=CARTESIAN_POINT('Ctrl Pts',(-20.9380782171066,-39.3579568876517,
1.72780310113342));
#23747=CARTESIAN_POINT('Ctrl Pts',(-21.1631094635642,-40.104467384704,3.28449990511991));
#23748=CARTESIAN_POINT('Ctrl Pts',(-21.3881407100217,-40.8509778817563,
4.84119670910639));
#23749=CARTESIAN_POINT('Ctrl Pts',(-21.9381972090395,-42.1032375437763,
5.91846432228299));
#23750=CARTESIAN_POINT('Ctrl Pts',(-22.4882537080573,-43.3554972057963,
6.99573193545957));
#23751=CARTESIAN_POINT('Ctrl Pts',(-23.218685614117,-44.8884264797115,7.3802042952164));
#23752=CARTESIAN_POINT('Ctrl Pts',(-23.9491175201768,-46.4213557536267,
7.76467665497322));
#23753=CARTESIAN_POINT('Ctrl Pts',(-24.6795494262366,-47.9542850275418,
7.38020429521639));
#23754=CARTESIAN_POINT('Ctrl Pts',(-21.0061649833184,-36.8732642383513,
0.));
#23755=CARTESIAN_POINT('Ctrl Pts',(-20.8258963691403,-36.9891158420918,
2.19648874705823));
#23756=CARTESIAN_POINT('Ctrl Pts',(-21.1608696725665,-37.9066995190545,
4.17545672685567));
#23757=CARTESIAN_POINT('Ctrl Pts',(-21.4958429759926,-38.8242831960173,
6.15442470665314));
#23758=CARTESIAN_POINT('Ctrl Pts',(-22.244008216214,-40.3848060765021,7.5239130403414));
#23759=CARTESIAN_POINT('Ctrl Pts',(-22.9921734564354,-41.9453289569869,
8.89340137402967));
#23760=CARTESIAN_POINT('Ctrl Pts',(-23.9696429220943,-43.862656176904,9.38216610144961));
#23761=CARTESIAN_POINT('Ctrl Pts',(-24.9471123877531,-45.7799833968211,
9.87093082886954));
#23762=CARTESIAN_POINT('Ctrl Pts',(-25.924581853412,-47.6973106167382,9.3821661014496));
#23763=CARTESIAN_POINT('Ctrl Pts',(-20.4339943155208,-34.5718269932684,
0.));
#23764=CARTESIAN_POINT('Ctrl Pts',(-20.2537257013426,-34.6876785970089,
2.70899372698069));
#23765=CARTESIAN_POINT('Ctrl Pts',(-20.7089199933764,-35.7923297837143,
5.14971273833323));
#23766=CARTESIAN_POINT('Ctrl Pts',(-21.1641142854102,-36.8969809704198,
7.59043174968578));
#23767=CARTESIAN_POINT('Ctrl Pts',(-22.1289102616396,-38.7945878558529,
9.27946171175752));
#23768=CARTESIAN_POINT('Ctrl Pts',(-23.0937062378689,-40.6921947412861,
10.9684916738293));
#23769=CARTESIAN_POINT('Ctrl Pts',(-24.341309812868,-43.0298588401132,11.5712994880388));
#23770=CARTESIAN_POINT('Ctrl Pts',(-25.588913387867,-45.3675229389403,12.1741073022483));
#23771=CARTESIAN_POINT('Ctrl Pts',(-26.8365169628661,-47.7051870377674,
11.5712994880388));
#23772=CARTESIAN_POINT('Ctrl Pts',(-19.4238236466309,-32.4262389885812,
0.));
#23773=CARTESIAN_POINT('Ctrl Pts',(-19.2435550324528,-32.5420905923217,
3.24562220582793));
#23774=CARTESIAN_POINT('Ctrl Pts',(-19.8246290891121,-33.8426145161275,
6.16982677025168));
#23775=CARTESIAN_POINT('Ctrl Pts',(-20.4057031457714,-35.1431384399332,
9.09403133467541));
#23776=CARTESIAN_POINT('Ctrl Pts',(-21.5973266200537,-37.3936958017628,
11.1176436806954));
#23777=CARTESIAN_POINT('Ctrl Pts',(-22.788950094336,-39.6442531635924,13.1412560267153));
#23778=CARTESIAN_POINT('Ctrl Pts',(-24.3194029329694,-42.4220393076082,
13.8634749112255));
#23779=CARTESIAN_POINT('Ctrl Pts',(-25.8498557716028,-45.199825451624,14.5856937957357));
#23780=CARTESIAN_POINT('Ctrl Pts',(-27.3803086102361,-47.9776115956398,
13.8634749112255));
#23781=CARTESIAN_POINT('',(-19.4238236466309,-32.4262389885812,0.));
#23782=CARTESIAN_POINT('Ctrl Pts',(-19.4238236466309,-32.4262389885812,
0.));
#23783=CARTESIAN_POINT('Ctrl Pts',(-19.2435550324528,-32.5420905923217,
3.24562220582793));
#23784=CARTESIAN_POINT('Ctrl Pts',(-19.8246290891121,-33.8426145161275,
6.16982677025168));
#23785=CARTESIAN_POINT('Ctrl Pts',(-20.3097318100837,-34.9283413471513,
8.61106394926976));
#23786=CARTESIAN_POINT('Ctrl Pts',(-21.2335670650398,-36.7013364119537,
10.4489096280657));
#23787=CARTESIAN_POINT('Origin',(-3.13849734404819,-40.0935818932913,0.));
#23788=CARTESIAN_POINT('Ctrl Pts',(-19.4238236466309,-32.4262389885812,
0.));
#23789=CARTESIAN_POINT('Ctrl Pts',(-19.2435550324528,-32.5420905923217,
3.24562220582793));
#23790=CARTESIAN_POINT('Ctrl Pts',(-19.8246290891121,-33.8426145161275,
6.16982677025168));
#23791=CARTESIAN_POINT('Ctrl Pts',(-20.4057031457715,-35.1431384399332,
9.09403133467541));
#23792=CARTESIAN_POINT('Ctrl Pts',(-21.5973266200537,-37.3936958017628,
11.1176436806954));
#23793=CARTESIAN_POINT('Ctrl Pts',(-22.7889500943361,-39.6442531635924,
13.1412560267153));
#23794=CARTESIAN_POINT('Ctrl Pts',(-24.3194029329694,-42.4220393076082,
13.8634749112255));
#23795=CARTESIAN_POINT('Ctrl Pts',(-25.8498557716028,-45.199825451624,14.5856937957357));
#23796=CARTESIAN_POINT('Ctrl Pts',(-27.3803086102362,-47.9776115956398,
13.8634749112255));
#23797=CARTESIAN_POINT('Ctrl Pts',(-19.6841717937389,-31.5100409519661,
6.24500451351651E-15));
#23798=CARTESIAN_POINT('Ctrl Pts',(-19.5039031795608,-31.6258925557066,
3.38941559469372));
#23799=CARTESIAN_POINT('Ctrl Pts',(-20.1187076077129,-32.9789019620468,
6.44317352589573));
#23800=CARTESIAN_POINT('Ctrl Pts',(-20.733512035865,-34.3319113683871,9.49693145709774));
#23801=CARTESIAN_POINT('Ctrl Pts',(-21.9859155393829,-36.6770443017776,
11.6101975146502));
#23802=CARTESIAN_POINT('Ctrl Pts',(-23.2383190429008,-39.0221772351682,
13.7234635722027));
#23803=CARTESIAN_POINT('Ctrl Pts',(-24.8445633383042,-41.9178971879303,
14.4776794959001));
#23804=CARTESIAN_POINT('Ctrl Pts',(-26.4508076337078,-44.8136171406925,
15.2318954195974));
#23805=CARTESIAN_POINT('Ctrl Pts',(-28.0570519291113,-47.7093370934547,
14.4776794959001));
#23806=CARTESIAN_POINT('Ctrl Pts',(-20.4854409432122,-30.9950965373907,
6.24500451351651E-15));
#23807=CARTESIAN_POINT('Ctrl Pts',(-20.3051723290341,-31.1109481411312,
3.38941559469371));
#23808=CARTESIAN_POINT('Ctrl Pts',(-20.9199767571862,-32.4639575474715,
6.44317352589574));
#23809=CARTESIAN_POINT('Ctrl Pts',(-21.5347811853383,-33.8169669538118,
9.49693145709774));
#23810=CARTESIAN_POINT('Ctrl Pts',(-22.7871846888562,-36.1620998872023,
11.6101975146502));
#23811=CARTESIAN_POINT('Ctrl Pts',(-24.0395881923741,-38.5072328205928,
13.7234635722027));
#23812=CARTESIAN_POINT('Ctrl Pts',(-25.6458324877776,-41.402952773355,14.4776794959001));
#23813=CARTESIAN_POINT('Ctrl Pts',(-27.2520767831811,-44.2986727261172,
15.2318954195974));
#23814=CARTESIAN_POINT('Ctrl Pts',(-28.8583210785846,-47.1943926788794,
14.4776794959001));
#23815=CARTESIAN_POINT('Ctrl Pts',(-21.4269965203142,-31.1388779521429,
0.));
#23816=CARTESIAN_POINT('Ctrl Pts',(-21.246727906136,-31.2547295558833,3.24562220582792));
#23817=CARTESIAN_POINT('Ctrl Pts',(-21.8278019627954,-32.5552534796891,
6.16982677025168));
#23818=CARTESIAN_POINT('Ctrl Pts',(-22.4088760194547,-33.8557774034949,
9.09403133467542));
#23819=CARTESIAN_POINT('Ctrl Pts',(-23.600499493737,-36.1063347653245,11.1176436806954));
#23820=CARTESIAN_POINT('Ctrl Pts',(-24.7921229680193,-38.356892127154,13.1412560267153));
#23821=CARTESIAN_POINT('Ctrl Pts',(-26.3225758066526,-41.1346782711698,
13.8634749112255));
#23822=CARTESIAN_POINT('Ctrl Pts',(-27.853028645286,-43.9124644151856,14.5856937957357));
#23823=CARTESIAN_POINT('Ctrl Pts',(-29.3834814839194,-46.6902505592015,
13.8634749112255));
#23824=CARTESIAN_POINT('',(-20.1821259000655,-31.4039916914148,5.03628278864507E-30));
#23825=CARTESIAN_POINT('Origin',(-21.1552751870376,-32.9182507396841,0.));
#23826=CARTESIAN_POINT('Origin',(-21.1552751870376,-32.9182507396841,0.));
#23827=CARTESIAN_POINT('Ctrl Pts',(-25.6404249706859,-27.7725495286737,
0.));
#23828=CARTESIAN_POINT('Ctrl Pts',(-25.4784786333242,-27.9128768288048,
3.24562220582792));
#23829=CARTESIAN_POINT('Ctrl Pts',(-26.2387220458134,-29.1174678338686,
6.16982677025167));
#23830=CARTESIAN_POINT('Ctrl Pts',(-26.9989654583024,-30.3220588389324,
9.09403133467541));
#23831=CARTESIAN_POINT('Ctrl Pts',(-28.4987476307692,-32.3801230698292,
11.1176436806954));
#23832=CARTESIAN_POINT('Ctrl Pts',(-29.998529803236,-34.4381873007259,13.1412560267153));
#23833=CARTESIAN_POINT('Ctrl Pts',(-31.9087250245462,-36.9698934388175,
13.8634749112255));
#23834=CARTESIAN_POINT('Ctrl Pts',(-33.8189202458565,-39.5015995769091,
14.5856937957357));
#23835=CARTESIAN_POINT('Ctrl Pts',(-35.7291154671667,-42.0333057150007,
13.8634749112255));
#23836=CARTESIAN_POINT('Ctrl Pts',(-27.4145036200622,-29.3462831821137,
0.));
#23837=CARTESIAN_POINT('Ctrl Pts',(-27.2525572827006,-29.4866104822448,
2.70899372698068));
#23838=CARTESIAN_POINT('Ctrl Pts',(-27.8603266081618,-30.5152370105914,
5.14971273833322));
#23839=CARTESIAN_POINT('Ctrl Pts',(-28.4680959336231,-31.543863538938,7.59043174968577));
#23840=CARTESIAN_POINT('Ctrl Pts',(-29.693129294942,-33.2848507390768,9.27946171175751));
#23841=CARTESIAN_POINT('Ctrl Pts',(-30.9181626562609,-35.0258379392156,
10.9684916738293));
#23842=CARTESIAN_POINT('Ctrl Pts',(-32.4857517139242,-37.1621554871448,
11.5712994880388));
#23843=CARTESIAN_POINT('Ctrl Pts',(-34.0533407715874,-39.298473035074,12.1741073022483));
#23844=CARTESIAN_POINT('Ctrl Pts',(-35.6209298292506,-41.4347905830031,
11.5712994880388));
#23845=CARTESIAN_POINT('Ctrl Pts',(-29.4615173807456,-30.5436667170412,
0.));
#23846=CARTESIAN_POINT('Ctrl Pts',(-29.299571043384,-30.6839940171723,2.19648874705824));
#23847=CARTESIAN_POINT('Ctrl Pts',(-29.761720574162,-31.5445663438471,4.17545672685568));
#23848=CARTESIAN_POINT('Ctrl Pts',(-30.2238701049401,-32.4051386705218,
6.15442470665313));
#23849=CARTESIAN_POINT('Ctrl Pts',(-31.1865056631392,-33.8433026630077,
7.5239130403414));
#23850=CARTESIAN_POINT('Ctrl Pts',(-32.1491412213383,-35.2814666554935,
8.89340137402967));
#23851=CARTESIAN_POINT('Ctrl Pts',(-33.3895255704508,-37.0401698399471,
9.3821661014496));
#23852=CARTESIAN_POINT('Ctrl Pts',(-34.6299099195633,-38.7988730244007,
9.87093082886953));
#23853=CARTESIAN_POINT('Ctrl Pts',(-35.8702942686759,-40.5575762088543,
9.3821661014496));
#23854=CARTESIAN_POINT('Ctrl Pts',(-31.7027984407113,-31.3186840564485,
1.04083408558608E-14));
#23855=CARTESIAN_POINT('Ctrl Pts',(-31.5408521033497,-31.4590113565796,
1.72780310113343));
#23856=CARTESIAN_POINT('Ctrl Pts',(-31.8698323768439,-32.1658981677051,
3.28449990511992));
#23857=CARTESIAN_POINT('Ctrl Pts',(-32.1988126503381,-32.8727849788306,
4.84119670910638));
#23858=CARTESIAN_POINT('Ctrl Pts',(-32.9214854985883,-34.0340172414017,
5.91846432228298));
#23859=CARTESIAN_POINT('Ctrl Pts',(-33.6441583468386,-35.1952495039728,
6.99573193545955));
#23860=CARTESIAN_POINT('Ctrl Pts',(-34.5853140909922,-36.6086244696004,
7.38020429521639));
#23861=CARTESIAN_POINT('Ctrl Pts',(-35.5264698351457,-38.0219994352281,
7.76467665497322));
#23862=CARTESIAN_POINT('Ctrl Pts',(-36.4676255792993,-39.4353744008558,
7.38020429521639));
#23863=CARTESIAN_POINT('',(-25.6404249706926,-27.7725495286889,1.57950248445926E-9));
#23864=CARTESIAN_POINT('Origin',(-37.5852932322717,-14.3070334890501,0.));
#23865=CARTESIAN_POINT('Ctrl Pts',(-25.6404249705937,-27.7725495288658,
3.13107430880991E-9));
#23866=CARTESIAN_POINT('Ctrl Pts',(-25.6281983378204,-27.7831439665413,
0.245038153335578));
#23867=CARTESIAN_POINT('Ctrl Pts',(-25.6200142870519,-27.7986217084844,
0.490791160521907));
#23868=CARTESIAN_POINT('Ctrl Pts',(-25.6159526330979,-27.819027185115,0.736766500725649));
#23869=CARTESIAN_POINT('Ctrl Pts',(-25.6119043133257,-27.8393656717118,
0.981934317701287));
#23870=CARTESIAN_POINT('Ctrl Pts',(-25.6119514551673,-27.8645996505509,
1.22732257376593));
#23871=CARTESIAN_POINT('Ctrl Pts',(-25.6161410294534,-27.8947338787563,
1.47243294816368));
#23872=CARTESIAN_POINT('Ctrl Pts',(-25.6203242940986,-27.9248227237928,
1.71717417803043));
#23873=CARTESIAN_POINT('Ctrl Pts',(-25.6286375769734,-27.9597970874098,
1.96163791541611));
#23874=CARTESIAN_POINT('Ctrl Pts',(-25.6410945477695,-27.9996219245319,
2.20532408778548));
#23875=CARTESIAN_POINT('Ctrl Pts',(-25.6535408348299,-28.0394126058353,
2.44880126242092));
#23876=CARTESIAN_POINT('Ctrl Pts',(-25.6701237175578,-28.084045412642,2.69150175431078));
#23877=CARTESIAN_POINT('Ctrl Pts',(-25.6908232719758,-28.1334457426221,
2.93292951866838));
#23878=CARTESIAN_POINT('Ctrl Pts',(-25.7115184960058,-28.1828357379546,
3.17430677585629));
#23879=CARTESIAN_POINT('Ctrl Pts',(-25.7363286400398,-28.2369911812595,
3.41441139318393));
#23880=CARTESIAN_POINT('Ctrl Pts',(-25.7652003562646,-28.2957987052587,
3.65275710614695));
#23881=CARTESIAN_POINT('Ctrl Pts',(-25.7941087333334,-28.3546809021123,
3.89140546668845));
#23882=CARTESIAN_POINT('Ctrl Pts',(-25.8270889373971,-28.4182268780899,
4.12829002081219));
#23883=CARTESIAN_POINT('Ctrl Pts',(-25.8640546001338,-28.4862854384147,
4.36293874377862));
#23884=CARTESIAN_POINT('Ctrl Pts',(-25.9010579825875,-28.5544134456112,
4.59782690201492));
#23885=CARTESIAN_POINT('Ctrl Pts',(-25.9420548501734,-28.6270630772623,
4.83047425894992));
#23886=CARTESIAN_POINT('Ctrl Pts',(-25.9869270447948,-28.7040474659739,
5.06042975959454));
#23887=CARTESIAN_POINT('Ctrl Pts',(-26.0319304281238,-28.7812569268612,
5.2910575599833));
#23888=CARTESIAN_POINT('Ctrl Pts',(-26.0808316886117,-28.8628263193252,
5.51897736305715));
#23889=CARTESIAN_POINT('Ctrl Pts',(-26.1334818341725,-28.9485346007076,
5.74376259354361));
#23890=CARTESIAN_POINT('Ctrl Pts',(-26.1670531325893,-29.0031847495427,
5.88709234072639));
#23891=CARTESIAN_POINT('Ctrl Pts',(-26.2021480259521,-29.0595170057058,
6.02914825314202));
#23892=CARTESIAN_POINT('Ctrl Pts',(-26.2387220458401,-29.1174678338917,
6.16982677023483));
#23893=CARTESIAN_POINT('Ctrl Pts',(-26.2960711849263,-29.2083364372326,
6.39041482339094));
#23894=CARTESIAN_POINT('Ctrl Pts',(-26.35724861586,-29.3038406779899,6.60890054011813));
#23895=CARTESIAN_POINT('Ctrl Pts',(-26.4221888209395,-29.4038573838826,
6.82480412008054));
#23896=CARTESIAN_POINT('Ctrl Pts',(-26.486982419861,-29.503648296448,7.04022028559293));
#23897=CARTESIAN_POINT('Ctrl Pts',(-26.5555217851613,-29.607931238224,7.25306552029626));
#23898=CARTESIAN_POINT('Ctrl Pts',(-26.6277100364533,-29.7165449255437,
7.46287566269394));
#23899=CARTESIAN_POINT('Ctrl Pts',(-26.6997821794599,-29.8249839175527,
7.6723483444186));
#23900=CARTESIAN_POINT('Ctrl Pts',(-26.7754914030011,-29.9377396021008,
7.87879526533007));
#23901=CARTESIAN_POINT('Ctrl Pts',(-26.8547104088648,-30.0546142350031,
8.08177334612175));
#23902=CARTESIAN_POINT('Ctrl Pts',(-26.9338534012417,-30.1713767224895,
8.2845566621408));
#23903=CARTESIAN_POINT('Ctrl Pts',(-27.0164993284344,-30.292250078758,8.48387739272815));
#23904=CARTESIAN_POINT('Ctrl Pts',(-27.1024918458752,-30.4170022653823,
8.67931873611046));
#23905=CARTESIAN_POINT('Ctrl Pts',(-27.1884884993286,-30.5417604522568,
8.87476947970436));
#23906=CARTESIAN_POINT('Ctrl Pts',(-27.2778319154178,-30.670397623316,9.06634009532763));
#23907=CARTESIAN_POINT('Ctrl Pts',(-27.3703382785457,-30.8026498047313,
9.2536445034091));
#23908=CARTESIAN_POINT('Ctrl Pts',(-27.46287857672,-30.9349505015543,9.44101762226428));
#23909=CARTESIAN_POINT('Ctrl Pts',(-27.5585839591968,-31.0708686028431,
9.62412107874973));
#23910=CARTESIAN_POINT('Ctrl Pts',(-27.6572454428935,-31.2101115092135,
9.80260437466071));
#23911=CARTESIAN_POINT('Ctrl Pts',(-27.7560678639057,-31.3495815496055,
9.98137881379635));
#23912=CARTESIAN_POINT('Ctrl Pts',(-27.8578558275196,-31.4923869622807,
10.1555177270921));
#23913=CARTESIAN_POINT('Ctrl Pts',(-27.9623772429048,-31.6382093995775,
10.3247095747706));
#23914=CARTESIAN_POINT('Ctrl Pts',(-27.992587469928,-31.6803570199438,10.3736117457754));
#23915=CARTESIAN_POINT('Ctrl Pts',(-28.0230259217676,-31.722756544904,10.4221009095756));
#23916=CARTESIAN_POINT('Ctrl Pts',(-28.0536866918425,-31.7653999649279,
10.4701702229111));
#23917=CARTESIAN_POINT('Ctrl Pts',(-26.4881263776669,-35.8372231206709,
1.04083408558608E-14));
#23918=CARTESIAN_POINT('Ctrl Pts',(-26.3261800403053,-35.9775504208021,
1.72780310113342));
#23919=CARTESIAN_POINT('Ctrl Pts',(-26.6551603137995,-36.6844372319276,
3.28449990511991));
#23920=CARTESIAN_POINT('Ctrl Pts',(-26.9841405872937,-37.3913240430531,
4.84119670910638));
#23921=CARTESIAN_POINT('Ctrl Pts',(-27.706813435544,-38.5525563056242,5.91846432228298));
#23922=CARTESIAN_POINT('Ctrl Pts',(-28.4294862837942,-39.7137885681952,
6.99573193545957));
#23923=CARTESIAN_POINT('Ctrl Pts',(-29.3706420279478,-41.1271635338229,
7.38020429521639));
#23924=CARTESIAN_POINT('Ctrl Pts',(-30.3117977721014,-42.5405384994506,
7.76467665497322));
#23925=CARTESIAN_POINT('Ctrl Pts',(-31.2529535162549,-43.9539134650783,
7.3802042952164));
#23926=CARTESIAN_POINT('Ctrl Pts',(-26.0399651488661,-33.5084586029185,
0.));
#23927=CARTESIAN_POINT('Ctrl Pts',(-25.8780188115045,-33.6487859030497,
2.19648874705823));
#23928=CARTESIAN_POINT('Ctrl Pts',(-26.3401683422825,-34.5093582297245,
4.17545672685567));
#23929=CARTESIAN_POINT('Ctrl Pts',(-26.8023178730605,-35.3699305563992,
6.15442470665314));
#23930=CARTESIAN_POINT('Ctrl Pts',(-27.7649534312596,-36.808094548885,7.5239130403414));
#23931=CARTESIAN_POINT('Ctrl Pts',(-28.7275889894587,-38.2462585413709,
8.89340137402967));
#23932=CARTESIAN_POINT('Ctrl Pts',(-29.9679733385713,-40.0049617258244,
9.3821661014496));
#23933=CARTESIAN_POINT('Ctrl Pts',(-31.2083576876838,-41.763664910278,9.87093082886954));
#23934=CARTESIAN_POINT('Ctrl Pts',(-32.4487420367963,-43.5223680947316,
9.3821661014496));
#23935=CARTESIAN_POINT('Ctrl Pts',(-25.1460896841345,-31.3118750466445,
-1.05434036998093E-14));
#23936=CARTESIAN_POINT('Ctrl Pts',(-24.9841433467729,-31.4522023467756,
2.70899372698069));
#23937=CARTESIAN_POINT('Ctrl Pts',(-25.5919126722341,-32.4808288751222,
5.14971273833323));
#23938=CARTESIAN_POINT('Ctrl Pts',(-26.1996819976954,-33.5094554034687,
7.59043174968578));
#23939=CARTESIAN_POINT('Ctrl Pts',(-27.4247153590143,-35.2504426036076,
9.27946171175751));
#23940=CARTESIAN_POINT('Ctrl Pts',(-28.6497487203333,-36.9914298037464,
10.9684916738292));
#23941=CARTESIAN_POINT('Ctrl Pts',(-30.2173377779965,-39.1277473516756,
11.5712994880388));
#23942=CARTESIAN_POINT('Ctrl Pts',(-31.7849268356597,-41.2640648996047,
12.1741073022483));
#23943=CARTESIAN_POINT('Ctrl Pts',(-33.3525158933229,-43.4003824475339,
11.5712994880388));
#23944=CARTESIAN_POINT('Ctrl Pts',(-23.84085208622,-29.3318883095341,0.));
#23945=CARTESIAN_POINT('Ctrl Pts',(-23.6789057488584,-29.4722156096652,
3.24562220582792));
#23946=CARTESIAN_POINT('Ctrl Pts',(-24.4391491613475,-30.676806614729,6.16982677025168));
#23947=CARTESIAN_POINT('Ctrl Pts',(-25.1993925738366,-31.8813976197928,
9.09403133467541));
#23948=CARTESIAN_POINT('Ctrl Pts',(-26.6991747463034,-33.9394618506896,
11.1176436806954));
#23949=CARTESIAN_POINT('Ctrl Pts',(-28.1989569187702,-35.9975260815863,
13.1412560267153));
#23950=CARTESIAN_POINT('Ctrl Pts',(-30.1091521400804,-38.529232219678,13.8634749112255));
#23951=CARTESIAN_POINT('Ctrl Pts',(-32.0193473613906,-41.0609383577696,
14.5856937957357));
#23952=CARTESIAN_POINT('Ctrl Pts',(-33.9295425827008,-43.5926444958612,
13.8634749112255));
#23953=CARTESIAN_POINT('',(-23.84085208622,-29.3318883095341,0.));
#23954=CARTESIAN_POINT('Ctrl Pts',(-23.84085208622,-29.3318883095341,0.));
#23955=CARTESIAN_POINT('Ctrl Pts',(-23.6789057488584,-29.4722156096652,
3.24562220582792));
#23956=CARTESIAN_POINT('Ctrl Pts',(-24.4391491613475,-30.676806614729,6.16982677025167));
#23957=CARTESIAN_POINT('Ctrl Pts',(-25.0738292744461,-31.6824449968208,
8.61106394926976));
#23958=CARTESIAN_POINT('Ctrl Pts',(-26.2405847244738,-33.3059180634111,
10.4489096280657));
#23959=CARTESIAN_POINT('Origin',(-8.81246358936573,-39.2388322978495,1.04083408558608E-14));
#23960=CARTESIAN_POINT('Ctrl Pts',(-23.84085208622,-29.3318883095341,0.));
#23961=CARTESIAN_POINT('Ctrl Pts',(-23.6789057488584,-29.4722156096652,
3.24562220582792));
#23962=CARTESIAN_POINT('Ctrl Pts',(-24.4391491613475,-30.676806614729,6.16982677025167));
#23963=CARTESIAN_POINT('Ctrl Pts',(-25.1993925738366,-31.8813976197928,
9.09403133467541));
#23964=CARTESIAN_POINT('Ctrl Pts',(-26.6991747463034,-33.9394618506896,
11.1176436806954));
#23965=CARTESIAN_POINT('Ctrl Pts',(-28.1989569187702,-35.9975260815863,
13.1412560267153));
#23966=CARTESIAN_POINT('Ctrl Pts',(-30.1091521400804,-38.529232219678,13.8634749112255));
#23967=CARTESIAN_POINT('Ctrl Pts',(-32.0193473613906,-41.0609383577696,
14.5856937957357));
#23968=CARTESIAN_POINT('Ctrl Pts',(-33.9295425827008,-43.5926444958612,
13.8634749112255));
#23969=CARTESIAN_POINT('Ctrl Pts',(-23.9681616891742,-28.3879644434328,
6.24500451351651E-15));
#23970=CARTESIAN_POINT('Ctrl Pts',(-23.8062153518126,-28.5282917435639,
3.38941559469373));
#23971=CARTESIAN_POINT('Ctrl Pts',(-24.6073152722065,-29.780033672264,6.44317352589573));
#23972=CARTESIAN_POINT('Ctrl Pts',(-25.4084151926004,-31.031775600964,9.49693145709775));
#23973=CARTESIAN_POINT('Ctrl Pts',(-26.981818248414,-33.174802860439,11.6101975146502));
#23974=CARTESIAN_POINT('Ctrl Pts',(-28.5552213042276,-35.317830119914,13.7234635722027));
#23975=CARTESIAN_POINT('Ctrl Pts',(-30.557220265479,-37.9554834217127,14.4776794959001));
#23976=CARTESIAN_POINT('Ctrl Pts',(-32.5592192267304,-40.5931367235114,
15.2318954195974));
#23977=CARTESIAN_POINT('Ctrl Pts',(-34.5612181879818,-43.2307900253102,
14.4776794959001));
#23978=CARTESIAN_POINT('Ctrl Pts',(-24.6879908429606,-27.7642289310886,
0.));
#23979=CARTESIAN_POINT('Ctrl Pts',(-24.526044505599,-27.9045562312197,3.38941559469372));
#23980=CARTESIAN_POINT('Ctrl Pts',(-25.3271444259928,-29.1562981599198,
6.44317352589573));
#23981=CARTESIAN_POINT('Ctrl Pts',(-26.1282443463867,-30.4080400886198,
9.49693145709774));
#23982=CARTESIAN_POINT('Ctrl Pts',(-27.7016474022003,-32.5510673480948,
11.6101975146502));
#23983=CARTESIAN_POINT('Ctrl Pts',(-29.2750504580139,-34.6940946075698,
13.7234635722027));
#23984=CARTESIAN_POINT('Ctrl Pts',(-31.2770494192653,-37.3317479093686,
14.4776794959001));
#23985=CARTESIAN_POINT('Ctrl Pts',(-33.2790483805167,-39.9694012111673,
15.2318954195974));
#23986=CARTESIAN_POINT('Ctrl Pts',(-35.2810473417681,-42.607054512966,14.4776794959001));
#23987=CARTESIAN_POINT('Ctrl Pts',(-25.6404249706859,-27.7725495286737,
0.));
#23988=CARTESIAN_POINT('Ctrl Pts',(-25.4784786333242,-27.9128768288048,
3.24562220582792));
#23989=CARTESIAN_POINT('Ctrl Pts',(-26.2387220458134,-29.1174678338686,
6.16982677025167));
#23990=CARTESIAN_POINT('Ctrl Pts',(-26.9989654583024,-30.3220588389324,
9.09403133467541));
#23991=CARTESIAN_POINT('Ctrl Pts',(-28.4987476307692,-32.3801230698292,
11.1176436806954));
#23992=CARTESIAN_POINT('Ctrl Pts',(-29.998529803236,-34.4381873007259,13.1412560267153));
#23993=CARTESIAN_POINT('Ctrl Pts',(-31.9087250245462,-36.9698934388175,
13.8634749112255));
#23994=CARTESIAN_POINT('Ctrl Pts',(-33.8189202458565,-39.5015995769092,
14.5856937957357));
#23995=CARTESIAN_POINT('Ctrl Pts',(-35.7291154671667,-42.0333057150007,
13.8634749112255));
#23996=CARTESIAN_POINT('',(-24.4459549573119,-28.2121283533451,1.04083408558608E-14));
#23997=CARTESIAN_POINT('Origin',(-25.6247005192791,-29.5724808444821,1.04083408558608E-14));
#23998=CARTESIAN_POINT('Origin',(-25.6247005192791,-29.5724808444821,1.04083408558608E-14));
#23999=CARTESIAN_POINT('Ctrl Pts',(-29.3318883095342,-23.8408520862199,
0.));
#24000=CARTESIAN_POINT('Ctrl Pts',(-29.191561009403,-24.0027984235815,3.24562220582793));
#24001=CARTESIAN_POINT('Ctrl Pts',(-30.1154974142046,-25.0869345107939,
6.16982677025168));
#24002=CARTESIAN_POINT('Ctrl Pts',(-31.0394338190061,-26.1710705980062,
9.09403133467541));
#24003=CARTESIAN_POINT('Ctrl Pts',(-32.8168434496406,-27.9947454451963,
11.1176436806954));
#24004=CARTESIAN_POINT('Ctrl Pts',(-34.5942530802751,-29.8184202923863,
13.1412560267153));
#24005=CARTESIAN_POINT('Ctrl Pts',(-36.8453046181045,-32.0525081884198,
13.8634749112255));
#24006=CARTESIAN_POINT('Ctrl Pts',(-39.0963561559338,-34.2865960844532,
14.5856937957357));
#24007=CARTESIAN_POINT('Ctrl Pts',(-41.3474076937632,-36.5206839804867,
13.8634749112255));
#24008=CARTESIAN_POINT('Ctrl Pts',(-31.3118750466446,-25.1460896841344,
0.));
#24009=CARTESIAN_POINT('Ctrl Pts',(-31.1715477465134,-25.308036021496,2.70899372698069));
#24010=CARTESIAN_POINT('Ctrl Pts',(-31.9195196745978,-26.2396980216805,
5.14971273833323));
#24011=CARTESIAN_POINT('Ctrl Pts',(-32.667491602682,-27.171360021865,7.59043174968578));
#24012=CARTESIAN_POINT('Ctrl Pts',(-34.1278242025586,-28.7202860579072,
9.27946171175751));
#24013=CARTESIAN_POINT('Ctrl Pts',(-35.5881568024352,-30.2692120939494,
10.9684916738293));
#24014=CARTESIAN_POINT('Ctrl Pts',(-37.4438197501021,-32.1606938263359,
11.5712994880388));
#24015=CARTESIAN_POINT('Ctrl Pts',(-39.299482697769,-34.0521755587224,12.1741073022483));
#24016=CARTESIAN_POINT('Ctrl Pts',(-41.1551456454359,-35.9436572911088,
11.5712994880388));
#24017=CARTESIAN_POINT('Ctrl Pts',(-33.5084586029187,-26.039965148866,0.));
#24018=CARTESIAN_POINT('Ctrl Pts',(-33.3681313027876,-26.2019114862276,
2.19648874705822));
#24019=CARTESIAN_POINT('Ctrl Pts',(-33.9480490292,-26.9879536917289,4.17545672685568));
#24020=CARTESIAN_POINT('Ctrl Pts',(-34.5279667556125,-27.7739958972302,
6.15442470665313));
#24021=CARTESIAN_POINT('Ctrl Pts',(-35.6854761478361,-29.0605241301525,
7.52391304034139));
#24022=CARTESIAN_POINT('Ctrl Pts',(-36.8429855400596,-30.3470523630749,
8.89340137402966));
#24023=CARTESIAN_POINT('Ctrl Pts',(-38.321034124251,-31.9113293869106,9.3821661014496));
#24024=CARTESIAN_POINT('Ctrl Pts',(-39.7990827084423,-33.4756064107464,
9.87093082886952));
#24025=CARTESIAN_POINT('Ctrl Pts',(-41.2771312926336,-35.0398834345822,
9.3821661014496));
#24026=CARTESIAN_POINT('Ctrl Pts',(-35.837223120671,-26.4881263776668,1.04083408558608E-14));
#24027=CARTESIAN_POINT('Ctrl Pts',(-35.6968958205399,-26.6500727150284,
1.72780310113343));
#24028=CARTESIAN_POINT('Ctrl Pts',(-36.1231280314032,-27.3029456632459,
3.28449990511991));
#24029=CARTESIAN_POINT('Ctrl Pts',(-36.5493602422664,-27.9558186114633,
4.84119670910638));
#24030=CARTESIAN_POINT('Ctrl Pts',(-37.4299379045752,-29.0023841344369,
5.91846432228297));
#24031=CARTESIAN_POINT('Ctrl Pts',(-38.310515566884,-30.0489496574104,6.99573193545955));
#24032=CARTESIAN_POINT('Ctrl Pts',(-39.4432359322495,-31.3139980762872,
7.38020429521638));
#24033=CARTESIAN_POINT('Ctrl Pts',(-40.5759562976149,-32.579046495164,7.76467665497321));
#24034=CARTESIAN_POINT('Ctrl Pts',(-41.7086766629803,-33.8440949140408,
7.38020429521638));
#24035=CARTESIAN_POINT('',(-29.3318883095546,-23.8408520862337,1.57949999773541E-9));
#24036=CARTESIAN_POINT('Origin',(-39.2388322978495,-8.8124635893656,0.));
#24037=CARTESIAN_POINT('Ctrl Pts',(-29.3318883094702,-23.8408520864232,
3.13107478882928E-9));
#24038=CARTESIAN_POINT('Ctrl Pts',(-29.3212938718736,-23.8530787192648,
0.24503815333568));
#24039=CARTESIAN_POINT('Ctrl Pts',(-29.315395835283,-23.8695636319736,0.490791160522109));
#24040=CARTESIAN_POINT('Ctrl Pts',(-29.3142795252164,-23.8903394438999,
0.736766500725953));
#24041=CARTESIAN_POINT('Ctrl Pts',(-29.313166879933,-23.9110470500025,0.981934317701616));
#24042=CARTESIAN_POINT('Ctrl Pts',(-29.3168047115562,-23.9360174743379,
1.22732257376628));
#24043=CARTESIAN_POINT('Ctrl Pts',(-29.3252401898304,-23.9652487409632,
1.47243294816406));
#24044=CARTESIAN_POINT('Ctrl Pts',(-29.3336629639885,-23.9944359843103,
1.71717417803081));
#24045=CARTESIAN_POINT('Ctrl Pts',(-29.3468690005323,-24.0278712558267,
1.96163791541648));
#24046=CARTESIAN_POINT('Ctrl Pts',(-29.3648668425815,-24.0655179217454,
2.20532408778585));
#24047=CARTESIAN_POINT('Ctrl Pts',(-29.3828492487602,-24.1031322999564,
2.44880126242126));
#24048=CARTESIAN_POINT('Ctrl Pts',(-29.4056152523348,-24.1449508188715,
2.69150175431109));
#24049=CARTESIAN_POINT('Ctrl Pts',(-29.4331345151069,-24.1909024709824,
2.93292951866866));
#24050=CARTESIAN_POINT('Ctrl Pts',(-29.4606480207944,-24.236844509916,3.17430677585639));
#24051=CARTESIAN_POINT('Ctrl Pts',(-29.4929127564909,-24.2869178772581,
3.41441139318384));
#24052=CARTESIAN_POINT('Ctrl Pts',(-29.5298597835412,-24.3410179518311,
3.65275710614668));
#24053=CARTESIAN_POINT('Ctrl Pts',(-29.5668537253363,-24.3951867218146,
3.89140546668824));
#24054=CARTESIAN_POINT('Ctrl Pts',(-29.6085417737704,-24.453392318975,4.12829002081204));
#24055=CARTESIAN_POINT('Ctrl Pts',(-29.6548169223662,-24.5154973789739,
4.36293874377852));
#24056=CARTESIAN_POINT('Ctrl Pts',(-29.7011392900671,-24.5776658109002,
4.59782690201493));
#24057=CARTESIAN_POINT('Ctrl Pts',(-29.7520579892327,-24.643741511473,4.83047425895005));
#24058=CARTESIAN_POINT('Ctrl Pts',(-29.8074294704422,-24.7135563309895,
5.06042975959478));
#24059=CARTESIAN_POINT('Ctrl Pts',(-29.8629628361578,-24.7835752616715,
5.29105755998348));
#24060=CARTESIAN_POINT('Ctrl Pts',(-29.9229748872203,-24.8573550203559,
5.51897736305728));
#24061=CARTESIAN_POINT('Ctrl Pts',(-29.9872866904181,-24.9346980180644,
5.74376259354367));
#24062=CARTESIAN_POINT('Ctrl Pts',(-30.028293808516,-24.9840142132785,5.88709234072643));
#24063=CARTESIAN_POINT('Ctrl Pts',(-30.0710484023924,-25.0347785642252,
6.02914825314204));
#24064=CARTESIAN_POINT('Ctrl Pts',(-30.1154974142344,-25.0869345108129,
6.16982677023484));
#24065=CARTESIAN_POINT('Ctrl Pts',(-30.1851947723638,-25.1687165693394,
6.39041482339092));
#24066=CARTESIAN_POINT('Ctrl Pts',(-30.259341175839,-25.2545422584422,6.60890054011809));
#24067=CARTESIAN_POINT('Ctrl Pts',(-30.3378542445905,-25.3442989836977,
6.82480412008047));
#24068=CARTESIAN_POINT('Ctrl Pts',(-30.4161900656827,-25.4338530781082,
7.04022028559297));
#24069=CARTESIAN_POINT('Ctrl Pts',(-30.4988728090634,-25.5273204012125,
7.25306552029641));
#24070=CARTESIAN_POINT('Ctrl Pts',(-30.5857836273892,-25.6245550984955,
7.4628756626942));
#24071=CARTESIAN_POINT('Ctrl Pts',(-30.6725546575098,-25.7216334025459,
7.67234834441867));
#24072=CARTESIAN_POINT('Ctrl Pts',(-30.7635400773297,-25.8224668509014,
7.87879526532997));
#24073=CARTESIAN_POINT('Ctrl Pts',(-30.8585857424178,-25.9268778285524,
8.08177334612148));
#24074=CARTESIAN_POINT('Ctrl Pts',(-30.95354020777,-26.0311886201131,8.28455666214051));
#24075=CARTESIAN_POINT('Ctrl Pts',(-31.0525469907384,-26.1390699181374,
8.48387739272782));
#24076=CARTESIAN_POINT('Ctrl Pts',(-31.1554183156063,-26.2503142961674,
8.67931873611011));
#24077=CARTESIAN_POINT('Ctrl Pts',(-31.2582945883127,-26.3615640247576,
8.87476947970392));
#24078=CARTESIAN_POINT('Ctrl Pts',(-31.3650355954438,-26.4761769610834,
9.06634009532712));
#24079=CARTESIAN_POINT('Ctrl Pts',(-31.4754218249876,-26.5939179778759,
9.25364450340851));
#24080=CARTESIAN_POINT('Ctrl Pts',(-31.5858485486304,-26.7117021867986,
9.44101762226367));
#24081=CARTESIAN_POINT('Ctrl Pts',(-31.6999229509126,-26.8326165417648,
9.62412107874909));
#24082=CARTESIAN_POINT('Ctrl Pts',(-31.8173965346642,-26.956401163024,9.80260437466004));
#24083=CARTESIAN_POINT('Ctrl Pts',(-31.935061742163,-27.0803877026398,9.98137881379573));
#24084=CARTESIAN_POINT('Ctrl Pts',(-32.0561369802829,-27.2072536245426,
10.1555177270915));
#24085=CARTESIAN_POINT('Ctrl Pts',(-32.1803472149474,-27.3367168513597,
10.32470957477));
#24086=CARTESIAN_POINT('Ctrl Pts',(-32.216248177194,-27.3741361061484,10.3736117457733));
#24087=CARTESIAN_POINT('Ctrl Pts',(-32.2524108910189,-27.4117722217276,
10.4221009095721));
#24088=CARTESIAN_POINT('Ctrl Pts',(-32.2888283700867,-27.4496181106866,
10.4701702229062));
#24089=CARTESIAN_POINT('Ctrl Pts',(-31.3186840564486,-31.7027984407112,
0.));
#24090=CARTESIAN_POINT('Ctrl Pts',(-31.1783567563174,-31.8647447780728,
1.72780310113343));
#24091=CARTESIAN_POINT('Ctrl Pts',(-31.6045889671807,-32.5176177262903,
3.28449990511991));
#24092=CARTESIAN_POINT('Ctrl Pts',(-32.030821178044,-33.1704906745077,4.84119670910639));
#24093=CARTESIAN_POINT('Ctrl Pts',(-32.9113988403528,-34.2170561974812,
5.91846432228298));
#24094=CARTESIAN_POINT('Ctrl Pts',(-33.7919765026616,-35.2636217204548,
6.99573193545956));
#24095=CARTESIAN_POINT('Ctrl Pts',(-34.924696868027,-36.5286701393316,7.38020429521639));
#24096=CARTESIAN_POINT('Ctrl Pts',(-36.0574172333924,-37.7937185582084,
7.76467665497322));
#24097=CARTESIAN_POINT('Ctrl Pts',(-37.1901375987578,-39.0587669770852,
7.38020429521639));
#24098=CARTESIAN_POINT('Ctrl Pts',(-30.5436667170413,-29.4615173807455,
0.));
#24099=CARTESIAN_POINT('Ctrl Pts',(-30.4033394169102,-29.6234637181072,
2.19648874705823));
#24100=CARTESIAN_POINT('Ctrl Pts',(-30.9832571433227,-30.4095059236084,
4.17545672685568));
#24101=CARTESIAN_POINT('Ctrl Pts',(-31.5631748697351,-31.1955481291097,
6.15442470665314));
#24102=CARTESIAN_POINT('Ctrl Pts',(-32.7206842619587,-32.4820763620321,
7.5239130403414));
#24103=CARTESIAN_POINT('Ctrl Pts',(-33.8781936541823,-33.7686045949544,
8.89340137402969));
#24104=CARTESIAN_POINT('Ctrl Pts',(-35.3562422383736,-35.3328816187902,
9.38216610144961));
#24105=CARTESIAN_POINT('Ctrl Pts',(-36.834290822565,-36.897158642626,9.87093082886954));
#24106=CARTESIAN_POINT('Ctrl Pts',(-38.3123394067563,-38.4614356664617,
9.38216610144961));
#24107=CARTESIAN_POINT('Ctrl Pts',(-29.3462831821138,-27.4145036200621,
0.));
#24108=CARTESIAN_POINT('Ctrl Pts',(-29.2059558819827,-27.5764499574237,
2.70899372698069));
#24109=CARTESIAN_POINT('Ctrl Pts',(-29.953927810067,-28.5081119576082,5.14971273833323));
#24110=CARTESIAN_POINT('Ctrl Pts',(-30.7018997381513,-29.4397739577927,
7.59043174968578));
#24111=CARTESIAN_POINT('Ctrl Pts',(-32.1622323380279,-30.9886999938349,
9.27946171175751));
#24112=CARTESIAN_POINT('Ctrl Pts',(-33.6225649379044,-32.5376260298771,
10.9684916738292));
#24113=CARTESIAN_POINT('Ctrl Pts',(-35.4782278855713,-34.4291077622636,
11.5712994880388));
#24114=CARTESIAN_POINT('Ctrl Pts',(-37.3338908332383,-36.3205894946501,
12.1741073022483));
#24115=CARTESIAN_POINT('Ctrl Pts',(-39.1895537809052,-38.2120712270365,
11.5712994880388));
#24116=CARTESIAN_POINT('Ctrl Pts',(-27.7725495286738,-25.6404249706858,
0.));
#24117=CARTESIAN_POINT('Ctrl Pts',(-27.6322222285426,-25.8023713080474,
3.24562220582793));
#24118=CARTESIAN_POINT('Ctrl Pts',(-28.5561586333442,-26.8865073952597,
6.16982677025167));
#24119=CARTESIAN_POINT('Ctrl Pts',(-29.4800950381457,-27.9706434824721,
9.09403133467541));
#24120=CARTESIAN_POINT('Ctrl Pts',(-31.2575046687802,-29.7943183296621,
11.1176436806954));
#24121=CARTESIAN_POINT('Ctrl Pts',(-33.0349142994147,-31.6179931768522,
13.1412560267153));
#24122=CARTESIAN_POINT('Ctrl Pts',(-35.2859658372441,-33.8520810728856,
13.8634749112255));
#24123=CARTESIAN_POINT('Ctrl Pts',(-37.5370173750734,-36.0861689689191,
14.5856937957357));
#24124=CARTESIAN_POINT('Ctrl Pts',(-39.7880689129028,-38.3202568649526,
13.8634749112255));
#24125=CARTESIAN_POINT('',(-27.7725495286738,-25.6404249706858,0.));
#24126=CARTESIAN_POINT('Ctrl Pts',(-27.7725495286738,-25.6404249706858,
0.));
#24127=CARTESIAN_POINT('Ctrl Pts',(-27.6322222285426,-25.8023713080474,
3.24562220582793));
#24128=CARTESIAN_POINT('Ctrl Pts',(-28.5561586333442,-26.8865073952597,
6.16982677025167));
#24129=CARTESIAN_POINT('Ctrl Pts',(-29.3274958817334,-27.7915854309818,
8.61106394926976));
#24130=CARTESIAN_POINT('Ctrl Pts',(-30.7134197505151,-29.2324872694338,
10.4489096280657));
#24131=CARTESIAN_POINT('Origin',(-14.3070334890502,-37.5852932322717,1.04083408558608E-14));
#24132=CARTESIAN_POINT('Ctrl Pts',(-27.7725495286738,-25.6404249706858,
0.));
#24133=CARTESIAN_POINT('Ctrl Pts',(-27.6322222285426,-25.8023713080474,
3.24562220582793));
#24134=CARTESIAN_POINT('Ctrl Pts',(-28.5561586333442,-26.8865073952597,
6.16982677025167));
#24135=CARTESIAN_POINT('Ctrl Pts',(-29.4800950381457,-27.9706434824721,
9.09403133467541));
#24136=CARTESIAN_POINT('Ctrl Pts',(-31.2575046687802,-29.7943183296621,
11.1176436806954));
#24137=CARTESIAN_POINT('Ctrl Pts',(-33.0349142994147,-31.6179931768522,
13.1412560267153));
#24138=CARTESIAN_POINT('Ctrl Pts',(-35.2859658372441,-33.8520810728856,
13.8634749112255));
#24139=CARTESIAN_POINT('Ctrl Pts',(-37.5370173750734,-36.0861689689191,
14.5856937957357));
#24140=CARTESIAN_POINT('Ctrl Pts',(-39.7880689129028,-38.3202568649526,
13.8634749112255));
#24141=CARTESIAN_POINT('Ctrl Pts',(-27.7642289310887,-24.6879908429605,
0.));
#24142=CARTESIAN_POINT('Ctrl Pts',(-27.6239016309576,-24.8499371803221,
3.38941559469372));
#24143=CARTESIAN_POINT('Ctrl Pts',(-28.5949889593954,-25.9749297754392,
6.44317352589573));
#24144=CARTESIAN_POINT('Ctrl Pts',(-29.5660762878332,-27.0999223705563,
9.49693145709774));
#24145=CARTESIAN_POINT('Ctrl Pts',(-31.4284489470459,-28.9972181010932,
11.6101975146502));
#24146=CARTESIAN_POINT('Ctrl Pts',(-33.2908216062586,-30.8945138316301,
13.7234635722027));
#24147=CARTESIAN_POINT('Ctrl Pts',(-35.6478203077951,-33.2204054676047,
14.4776794959001));
#24148=CARTESIAN_POINT('Ctrl Pts',(-38.0048190093316,-35.5462971035794,
15.2318954195974));
#24149=CARTESIAN_POINT('Ctrl Pts',(-40.361817710868,-37.872188739554,14.4776794959001));
#24150=CARTESIAN_POINT('Ctrl Pts',(-28.3879644434329,-23.9681616891741,
0.));
#24151=CARTESIAN_POINT('Ctrl Pts',(-28.2476371433017,-24.1301080265358,
3.38941559469373));
#24152=CARTESIAN_POINT('Ctrl Pts',(-29.2187244717395,-25.2551006216529,
6.44317352589574));
#24153=CARTESIAN_POINT('Ctrl Pts',(-30.1898118001773,-26.38009321677,9.49693145709774));
#24154=CARTESIAN_POINT('Ctrl Pts',(-32.05218445939,-28.2773889473069,11.6101975146502));
#24155=CARTESIAN_POINT('Ctrl Pts',(-33.9145571186028,-30.1746846778437,
13.7234635722027));
#24156=CARTESIAN_POINT('Ctrl Pts',(-36.2715558201393,-32.5005763138184,
14.4776794959001));
#24157=CARTESIAN_POINT('Ctrl Pts',(-38.6285545216757,-34.826467949793,15.2318954195974));
#24158=CARTESIAN_POINT('Ctrl Pts',(-40.9855532232122,-37.1523595857677,
14.4776794959001));
#24159=CARTESIAN_POINT('Ctrl Pts',(-29.3318883095342,-23.8408520862199,
0.));
#24160=CARTESIAN_POINT('Ctrl Pts',(-29.191561009403,-24.0027984235816,3.24562220582793));
#24161=CARTESIAN_POINT('Ctrl Pts',(-30.1154974142046,-25.0869345107939,
6.16982677025167));
#24162=CARTESIAN_POINT('Ctrl Pts',(-31.0394338190061,-26.1710705980062,
9.09403133467541));
#24163=CARTESIAN_POINT('Ctrl Pts',(-32.8168434496406,-27.9947454451963,
11.1176436806954));
#24164=CARTESIAN_POINT('Ctrl Pts',(-34.5942530802751,-29.8184202923863,
13.1412560267153));
#24165=CARTESIAN_POINT('Ctrl Pts',(-36.8453046181045,-32.0525081884198,
13.8634749112255));
#24166=CARTESIAN_POINT('Ctrl Pts',(-39.0963561559338,-34.2865960844532,
14.5856937957357));
#24167=CARTESIAN_POINT('Ctrl Pts',(-41.3474076937632,-36.5206839804867,
13.8634749112255));
#24168=CARTESIAN_POINT('',(-28.2121348679537,-24.4459474390529,-3.59391607130504E-31));
#24169=CARTESIAN_POINT('Origin',(-29.5724808444822,-25.624700519279,0.));
#24170=CARTESIAN_POINT('Origin',(-29.5724808444822,-25.624700519279,0.));
#24171=CARTESIAN_POINT('Ctrl Pts',(-32.4262389885813,-19.4238236466308,
0.));
#24172=CARTESIAN_POINT('Ctrl Pts',(-32.3103873848408,-19.6040922608089,
3.24562220582792));
#24173=CARTESIAN_POINT('Ctrl Pts',(-33.3792081011656,-20.5457035458245,
6.16982677025168));
#24174=CARTESIAN_POINT('Ctrl Pts',(-34.4480288174904,-21.48731483084,9.09403133467541));
#24175=CARTESIAN_POINT('Ctrl Pts',(-36.466882971839,-23.0394755334785,11.1176436806954));
#24176=CARTESIAN_POINT('Ctrl Pts',(-38.4857371261876,-24.591636236117,13.1412560267153));
#24177=CARTESIAN_POINT('Ctrl Pts',(-41.0318200627225,-26.4826263031066,
13.8634749112255));
#24178=CARTESIAN_POINT('Ctrl Pts',(-43.5779029992573,-28.3736163700961,
14.5856937957357));
#24179=CARTESIAN_POINT('Ctrl Pts',(-46.1239859357922,-30.2646064370857,
13.8634749112255));
#24180=CARTESIAN_POINT('Ctrl Pts',(-34.5718269932685,-20.4339943155206,
0.));
#24181=CARTESIAN_POINT('Ctrl Pts',(-34.455975389528,-20.6142629296987,2.7089937269807));
#24182=CARTESIAN_POINT('Ctrl Pts',(-35.3289233687525,-21.4299944500888,
5.14971273833323));
#24183=CARTESIAN_POINT('Ctrl Pts',(-36.2018713479769,-22.2457259704788,
7.59043174968578));
#24184=CARTESIAN_POINT('Ctrl Pts',(-37.8677750259291,-23.5710591750643,
9.27946171175751));
#24185=CARTESIAN_POINT('Ctrl Pts',(-39.5336787038813,-24.8963923796499,
10.9684916738293));
#24186=CARTESIAN_POINT('Ctrl Pts',(-41.6396395952274,-26.5045331830051,
11.5712994880388));
#24187=CARTESIAN_POINT('Ctrl Pts',(-43.7456004865736,-28.1126739863604,
12.1741073022483));
#24188=CARTESIAN_POINT('Ctrl Pts',(-45.8515613779198,-29.7208147897157,
11.5712994880388));
#24189=CARTESIAN_POINT('Ctrl Pts',(-36.8732642383513,-21.0061649833183,
0.));
#24190=CARTESIAN_POINT('Ctrl Pts',(-36.7574126346109,-21.1864335974964,
2.19648874705824));
#24191=CARTESIAN_POINT('Ctrl Pts',(-37.4432931040927,-21.8819441292788,
4.17545672685568));
#24192=CARTESIAN_POINT('Ctrl Pts',(-38.1291735735745,-22.5774546610611,
6.15442470665314));
#24193=CARTESIAN_POINT('Ctrl Pts',(-39.4579932465783,-23.6861571296387,
7.5239130403414));
#24194=CARTESIAN_POINT('Ctrl Pts',(-40.7868129195821,-24.7948595982163,
8.89340137402967));
#24195=CARTESIAN_POINT('Ctrl Pts',(-42.4724369320183,-26.1328662922314,
9.38216610144961));
#24196=CARTESIAN_POINT('Ctrl Pts',(-44.1580609444544,-27.4708729862465,
9.87093082886954));
#24197=CARTESIAN_POINT('Ctrl Pts',(-45.8436849568905,-28.8088796802616,
9.38216610144961));
#24198=CARTESIAN_POINT('Ctrl Pts',(-39.2421052839113,-21.1183468312846,
0.));
#24199=CARTESIAN_POINT('Ctrl Pts',(-39.1262536801708,-21.2986154454627,
1.72780310113343));
#24200=CARTESIAN_POINT('Ctrl Pts',(-39.6410609697422,-21.8841839202765,
3.28449990511991));
#24201=CARTESIAN_POINT('Ctrl Pts',(-40.1558682593135,-22.4697523950902,
4.84119670910639));
#24202=CARTESIAN_POINT('Ctrl Pts',(-41.1764247138525,-23.3803461224642,
5.91846432228297));
#24203=CARTESIAN_POINT('Ctrl Pts',(-42.1969811683915,-24.2909398498382,
6.99573193545956));
#24204=CARTESIAN_POINT('Ctrl Pts',(-43.4982072348258,-25.3819089842542,
7.38020429521639));
#24205=CARTESIAN_POINT('Ctrl Pts',(-44.7994333012599,-26.4728781186702,
7.76467665497321));
#24206=CARTESIAN_POINT('Ctrl Pts',(-46.1006593676942,-27.5638472530862,
7.38020429521639));
#24207=CARTESIAN_POINT('',(-32.4262389886035,-19.4238236466415,1.57949966272277E-9));
#24208=CARTESIAN_POINT('Origin',(-40.0935818932913,-3.13849734404805,0.));
#24209=CARTESIAN_POINT('Ctrl Pts',(-32.4262389885469,-19.4238236468412,
3.13107437314513E-9));
#24210=CARTESIAN_POINT('Ctrl Pts',(-32.4174924183246,-19.4374335758629,
0.245038153335358));
#24211=CARTESIAN_POINT('Ctrl Pts',(-32.4140004629283,-19.454590074053,0.490791160521465));
#24212=CARTESIAN_POINT('Ctrl Pts',(-32.4158522216029,-19.4753132856568,
0.736766500724985));
#24213=CARTESIAN_POINT('Ctrl Pts',(-32.4176979010577,-19.4959684641207,
0.981934317700663));
#24214=CARTESIAN_POINT('Ctrl Pts',(-32.4248523667011,-19.5201670081216,
1.22732257376534));
#24215=CARTESIAN_POINT('Ctrl Pts',(-32.4373620269518,-19.5479002488743,
1.47243294816314));
#24216=CARTESIAN_POINT('Ctrl Pts',(-32.4498528472302,-19.5755917224265,
1.7171741780299));
#24217=CARTESIAN_POINT('Ctrl Pts',(-32.4676828006219,-19.6068072561337,
1.96163791541559));
#24218=CARTESIAN_POINT('Ctrl Pts',(-32.4908551297615,-19.6415093732947,
2.20532408778497));
#24219=CARTESIAN_POINT('Ctrl Pts',(-32.5140075851257,-19.676181728144,2.44880126242033));
#24220=CARTESIAN_POINT('Ctrl Pts',(-32.542493259366,-19.7143346547169,2.69150175431012));
#24221=CARTESIAN_POINT('Ctrl Pts',(-32.5762720176611,-19.7559021858353,
2.93292951866765));
#24222=CARTESIAN_POINT('Ctrl Pts',(-32.6100437093726,-19.7974610209433,
3.17430677585542));
#24223=CARTESIAN_POINT('Ctrl Pts',(-32.6491062197567,-19.8424329629631,
3.41441139318292));
#24224=CARTESIAN_POINT('Ctrl Pts',(-32.6933764227083,-19.8907242666035,
3.6527571061458));
#24225=CARTESIAN_POINT('Ctrl Pts',(-32.7377028392565,-19.9390768897698,
3.89140546668732));
#24226=CARTESIAN_POINT('Ctrl Pts',(-32.7872500836132,-19.9907572100057,
4.12829002081109));
#24227=CARTESIAN_POINT('Ctrl Pts',(-32.8418926894892,-20.0456444897535,
4.36293874377754));
#24228=CARTESIAN_POINT('Ctrl Pts',(-32.8965910526135,-20.1005877764144,
4.5978269020138));
#24229=CARTESIAN_POINT('Ctrl Pts',(-32.956395025481,-20.1587444351918,4.83047425894876));
#24230=CARTESIAN_POINT('Ctrl Pts',(-33.0211385895994,-20.2199684571169,
5.06042975959334));
#24231=CARTESIAN_POINT('Ctrl Pts',(-33.0860714385206,-20.281371474083,5.2910575599822));
#24232=CARTESIAN_POINT('Ctrl Pts',(-33.1559726078586,-20.3458596558642,
5.51897736305615));
#24233=CARTESIAN_POINT('Ctrl Pts',(-33.2306368658403,-20.4132628895043,
5.74376259354269));
#24234=CARTESIAN_POINT('Ctrl Pts',(-33.2782450169495,-20.4562411955792,
5.88709234072579));
#24235=CARTESIAN_POINT('Ctrl Pts',(-33.3277889511024,-20.5004042255165,
6.02914825314172));
#24236=CARTESIAN_POINT('Ctrl Pts',(-33.3792081011978,-20.545703545839,6.16982677023484));
#24237=CARTESIAN_POINT('Ctrl Pts',(-33.4598348411496,-20.6167342126795,
6.3904148233909));
#24238=CARTESIAN_POINT('Ctrl Pts',(-33.545440810212,-20.6911341865985,6.60890054011805));
#24239=CARTESIAN_POINT('Ctrl Pts',(-33.6359284429689,-20.7688037431277,
6.82480412008041));
#24240=CARTESIAN_POINT('Ctrl Pts',(-33.726211794816,-20.8462979562737,7.04022028559295));
#24241=CARTESIAN_POINT('Ctrl Pts',(-33.8213547340592,-20.9270469355454,
7.25306552029643));
#24242=CARTESIAN_POINT('Ctrl Pts',(-33.921218865788,-21.0109232247567,7.46287566269427));
#24243=CARTESIAN_POINT('Ctrl Pts',(-34.0209223750762,-21.0946646065288,
7.67234834441895));
#24244=CARTESIAN_POINT('Ctrl Pts',(-34.1253317904079,-21.1815231404631,
7.87879526533046));
#24245=CARTESIAN_POINT('Ctrl Pts',(-34.2342692590684,-21.2713449564543,
8.08177334612217));
#24246=CARTESIAN_POINT('Ctrl Pts',(-34.3431021983076,-21.3610805851809,
8.28455666214149));
#24247=CARTESIAN_POINT('Ctrl Pts',(-34.4564543444627,-21.4537736728373,
8.48387739272907));
#24248=CARTESIAN_POINT('Ctrl Pts',(-34.5741103132399,-21.5492456275387,
8.67931873611163));
#24249=CARTESIAN_POINT('Ctrl Pts',(-34.6917719409579,-21.6447221741884,
8.87476947970546));
#24250=CARTESIAN_POINT('Ctrl Pts',(-34.8137376000415,-21.7429776869136,
9.06634009532869));
#24251=CARTESIAN_POINT('Ctrl Pts',(-34.9397565506953,-21.8438106715187,
9.2536445034101));
#24252=CARTESIAN_POINT('Ctrl Pts',(-35.0658217301577,-21.9446806457091,
9.44101762226536));
#24253=CARTESIAN_POINT('Ctrl Pts',(-35.1959429263785,-22.0481297867741,
9.62412107875087));
#24254=CARTESIAN_POINT('Ctrl Pts',(-35.3298371867857,-22.1539362249986,
9.80260437466191));
#24255=CARTESIAN_POINT('Ctrl Pts',(-35.4639498564648,-22.2599152554393,
9.98137881379736));
#24256=CARTESIAN_POINT('Ctrl Pts',(-35.6018476263945,-22.3682590622507,
10.1555177270929));
#24257=CARTESIAN_POINT('Ctrl Pts',(-35.7432181181532,-22.478727580631,10.3247095747712));
#24258=CARTESIAN_POINT('Ctrl Pts',(-35.7840789755622,-22.5106567217238,
10.3736117457741));
#24259=CARTESIAN_POINT('Ctrl Pts',(-35.8252297828043,-22.5427632651434,
10.4221009095725));
#24260=CARTESIAN_POINT('Ctrl Pts',(-35.866662616011,-22.575041189878,10.4701702229062));
#24261=CARTESIAN_POINT('Ctrl Pts',(-35.5116836434677,-26.9229962078197,
0.));
#24262=CARTESIAN_POINT('Ctrl Pts',(-35.3958320397272,-27.1032648219978,
1.72780310113342));
#24263=CARTESIAN_POINT('Ctrl Pts',(-35.9106393292985,-27.6888332968116,
3.28449990511992));
#24264=CARTESIAN_POINT('Ctrl Pts',(-36.4254466188699,-28.2744017716254,
4.84119670910638));
#24265=CARTESIAN_POINT('Ctrl Pts',(-37.4460030734089,-29.1849954989994,
5.91846432228298));
#24266=CARTESIAN_POINT('Ctrl Pts',(-38.4665595279479,-30.0955892263734,
6.99573193545956));
#24267=CARTESIAN_POINT('Ctrl Pts',(-39.7677855943821,-31.1865583607894,
7.38020429521639));
#24268=CARTESIAN_POINT('Ctrl Pts',(-41.0690116608163,-32.2775274952054,
7.76467665497322));
#24269=CARTESIAN_POINT('Ctrl Pts',(-42.3702377272506,-33.3684966296214,
7.38020429521639));
#24270=CARTESIAN_POINT('Ctrl Pts',(-34.4255873115189,-24.8148246247008,
0.));
#24271=CARTESIAN_POINT('Ctrl Pts',(-34.3097357077784,-24.995093238879,2.19648874705823));
#24272=CARTESIAN_POINT('Ctrl Pts',(-34.9956161772602,-25.6906037706613,
4.17545672685568));
#24273=CARTESIAN_POINT('Ctrl Pts',(-35.681496646742,-26.3861143024436,6.15442470665313));
#24274=CARTESIAN_POINT('Ctrl Pts',(-37.0103163197458,-27.4948167710213,
7.5239130403414));
#24275=CARTESIAN_POINT('Ctrl Pts',(-38.3391359927496,-28.6035192395989,
8.89340137402967));
#24276=CARTESIAN_POINT('Ctrl Pts',(-40.0247600051858,-29.941525933614,9.3821661014496));
#24277=CARTESIAN_POINT('Ctrl Pts',(-41.7103840176219,-31.2795326276291,
9.87093082886954));
#24278=CARTESIAN_POINT('Ctrl Pts',(-43.3960080300581,-32.6175393216441,
9.3821661014496));
#24279=CARTESIAN_POINT('Ctrl Pts',(-32.9490709821976,-22.9590519566754,
-1.05434036998093E-14));
#24280=CARTESIAN_POINT('Ctrl Pts',(-32.8332193784571,-23.1393205708535,
2.70899372698069));
#24281=CARTESIAN_POINT('Ctrl Pts',(-33.7061673576816,-23.9550520912435,
5.14971273833323));
#24282=CARTESIAN_POINT('Ctrl Pts',(-34.5791153369061,-24.7707836116335,
7.59043174968578));
#24283=CARTESIAN_POINT('Ctrl Pts',(-36.2450190148583,-26.096116816219,9.27946171175751));
#24284=CARTESIAN_POINT('Ctrl Pts',(-37.9109226928105,-27.4214500208046,
10.9684916738293));
#24285=CARTESIAN_POINT('Ctrl Pts',(-40.0168835841566,-29.0295908241599,
11.5712994880388));
#24286=CARTESIAN_POINT('Ctrl Pts',(-42.1228444755027,-30.6377316275152,
12.1741073022483));
#24287=CARTESIAN_POINT('Ctrl Pts',(-44.2288053668489,-32.2458724308704,
11.5712994880388));
#24288=CARTESIAN_POINT('Ctrl Pts',(-31.1388779521429,-21.4269965203141,
0.));
#24289=CARTESIAN_POINT('Ctrl Pts',(-31.0230263484024,-21.6072651344922,
3.24562220582793));
#24290=CARTESIAN_POINT('Ctrl Pts',(-32.0918470647272,-22.5488764195077,
6.16982677025168));
#24291=CARTESIAN_POINT('Ctrl Pts',(-33.160667781052,-23.4904877045232,9.09403133467541));
#24292=CARTESIAN_POINT('Ctrl Pts',(-35.1795219354007,-25.0426484071617,
11.1176436806954));
#24293=CARTESIAN_POINT('Ctrl Pts',(-37.1983760897493,-26.5948091098002,
13.1412560267153));
#24294=CARTESIAN_POINT('Ctrl Pts',(-39.7444590262841,-28.4857991767898,
13.8634749112255));
#24295=CARTESIAN_POINT('Ctrl Pts',(-42.2905419628189,-30.3767892437794,
14.5856937957357));
#24296=CARTESIAN_POINT('Ctrl Pts',(-44.8366248993538,-32.267779310769,13.8634749112255));
#24297=CARTESIAN_POINT('',(-31.1388779521429,-21.4269965203141,0.));
#24298=CARTESIAN_POINT('Ctrl Pts',(-31.1388779521429,-21.4269965203141,
0.));
#24299=CARTESIAN_POINT('Ctrl Pts',(-31.0230263484024,-21.6072651344922,
3.24562220582793));
#24300=CARTESIAN_POINT('Ctrl Pts',(-32.0918470647272,-22.5488764195077,
6.16982677025168));
#24301=CARTESIAN_POINT('Ctrl Pts',(-32.9841392463828,-23.3349693300821,
8.61106394926976));
#24302=CARTESIAN_POINT('Ctrl Pts',(-34.5610181206245,-24.5639673341829,
10.4489096280657));
#24303=CARTESIAN_POINT('Origin',(-19.5103534449752,-35.1666259835201,0.));
#24304=CARTESIAN_POINT('Ctrl Pts',(-31.1388779521429,-21.4269965203141,
0.));
#24305=CARTESIAN_POINT('Ctrl Pts',(-31.0230263484024,-21.6072651344922,
3.24562220582793));
#24306=CARTESIAN_POINT('Ctrl Pts',(-32.0918470647273,-22.5488764195077,
6.16982677025168));
#24307=CARTESIAN_POINT('Ctrl Pts',(-33.160667781052,-23.4904877045232,9.09403133467541));
#24308=CARTESIAN_POINT('Ctrl Pts',(-35.1795219354007,-25.0426484071617,
11.1176436806954));
#24309=CARTESIAN_POINT('Ctrl Pts',(-37.1983760897493,-26.5948091098002,
13.1412560267153));
#24310=CARTESIAN_POINT('Ctrl Pts',(-39.7444590262841,-28.4857991767898,
13.8634749112255));
#24311=CARTESIAN_POINT('Ctrl Pts',(-42.2905419628189,-30.3767892437794,
14.5856937957357));
#24312=CARTESIAN_POINT('Ctrl Pts',(-44.8366248993538,-32.267779310769,13.8634749112255));
#24313=CARTESIAN_POINT('Ctrl Pts',(-30.9950965373908,-20.4854409432121,
0.));
#24314=CARTESIAN_POINT('Ctrl Pts',(-30.8792449336503,-20.6657095573902,
3.38941559469372));
#24315=CARTESIAN_POINT('Ctrl Pts',(-32.0005511325096,-21.6410512138985,
6.44317352589573));
#24316=CARTESIAN_POINT('Ctrl Pts',(-33.121857331369,-22.6163928704068,9.49693145709774));
#24317=CARTESIAN_POINT('Ctrl Pts',(-35.2352870572785,-24.2293336022809,
11.6101975146502));
#24318=CARTESIAN_POINT('Ctrl Pts',(-37.348716783188,-25.842274334155,13.7234635722027));
#24319=CARTESIAN_POINT('Ctrl Pts',(-40.0127335284693,-27.8090558579147,
14.4776794959001));
#24320=CARTESIAN_POINT('Ctrl Pts',(-42.6767502737505,-29.7758373816744,
15.2318954195974));
#24321=CARTESIAN_POINT('Ctrl Pts',(-45.3407670190317,-31.7426189054341,
14.4776794959001));
#24322=CARTESIAN_POINT('Ctrl Pts',(-31.5100409519661,-19.6841717937388,
6.24500451351651E-15));
#24323=CARTESIAN_POINT('Ctrl Pts',(-31.3941893482257,-19.8644404079169,
3.38941559469372));
#24324=CARTESIAN_POINT('Ctrl Pts',(-32.515495547085,-20.8397820644252,6.44317352589573));
#24325=CARTESIAN_POINT('Ctrl Pts',(-33.6368017459443,-21.8151237209335,
9.49693145709774));
#24326=CARTESIAN_POINT('Ctrl Pts',(-35.7502314718538,-23.4280644528076,
11.6101975146502));
#24327=CARTESIAN_POINT('Ctrl Pts',(-37.8636611977633,-25.0410051846817,
13.7234635722027));
#24328=CARTESIAN_POINT('Ctrl Pts',(-40.5276779430446,-27.0077867084414,
14.4776794959001));
#24329=CARTESIAN_POINT('Ctrl Pts',(-43.1916946883258,-28.9745682322011,
15.2318954195974));
#24330=CARTESIAN_POINT('Ctrl Pts',(-45.855711433607,-30.9413497559608,14.4776794959001));
#24331=CARTESIAN_POINT('Ctrl Pts',(-32.4262389885813,-19.4238236466308,
0.));
#24332=CARTESIAN_POINT('Ctrl Pts',(-32.3103873848408,-19.6040922608089,
3.24562220582792));
#24333=CARTESIAN_POINT('Ctrl Pts',(-33.3792081011656,-20.5457035458245,
6.16982677025168));
#24334=CARTESIAN_POINT('Ctrl Pts',(-34.4480288174904,-21.48731483084,9.09403133467541));
#24335=CARTESIAN_POINT('Ctrl Pts',(-36.466882971839,-23.0394755334785,11.1176436806954));
#24336=CARTESIAN_POINT('Ctrl Pts',(-38.4857371261876,-24.591636236117,13.1412560267153));
#24337=CARTESIAN_POINT('Ctrl Pts',(-41.0318200627225,-26.4826263031066,
13.8634749112255));
#24338=CARTESIAN_POINT('Ctrl Pts',(-43.5779029992573,-28.3736163700962,
14.5856937957357));
#24339=CARTESIAN_POINT('Ctrl Pts',(-46.1239859357922,-30.2646064370857,
13.8634749112255));
#24340=CARTESIAN_POINT('',(-31.4039970697396,-20.1821175312286,-3.07395939441906E-30));
#24341=CARTESIAN_POINT('Origin',(-32.9182507396842,-21.1552751870375,0.));
#24342=CARTESIAN_POINT('Origin',(-32.9182507396842,-21.1552751870375,0.));
#24343=CARTESIAN_POINT('Ctrl Pts',(-34.8604849513723,-14.6113821712782,
0.));
#24344=CARTESIAN_POINT('Ctrl Pts',(-34.7714674485862,-14.8063033131399,
3.24562220582793));
#24345=CARTESIAN_POINT('Ctrl Pts',(-35.9634143688743,-15.5862213055784,
6.16982677025167));
#24346=CARTESIAN_POINT('Ctrl Pts',(-37.1553612891624,-16.366139298017,9.09403133467541));
#24347=CARTESIAN_POINT('Ctrl Pts',(-39.3745619185372,-17.6151883402601,
11.1176436806954));
#24348=CARTESIAN_POINT('Ctrl Pts',(-41.593762547912,-18.8642373825032,13.1412560267153));
#24349=CARTESIAN_POINT('Ctrl Pts',(-44.3830459768614,-20.37363451585,13.8634749112255));
#24350=CARTESIAN_POINT('Ctrl Pts',(-47.1723294058108,-21.8830316491968,
14.5856937957357));
#24351=CARTESIAN_POINT('Ctrl Pts',(-49.9616128347602,-23.3924287825436,
13.8634749112255));
#24352=CARTESIAN_POINT('Ctrl Pts',(-37.1279962392257,-15.3059217494164,
0.));
#24353=CARTESIAN_POINT('Ctrl Pts',(-37.0389787364396,-15.5008428912781,
2.70899372698069));
#24354=CARTESIAN_POINT('Ctrl Pts',(-38.0191320633213,-16.1840379904939,
5.14971273833323));
#24355=CARTESIAN_POINT('Ctrl Pts',(-38.9992853902031,-16.8672330897098,
7.59043174968578));
#24356=CARTESIAN_POINT('Ctrl Pts',(-40.8368471514173,-17.9419935007387,
9.2794617117575));
#24357=CARTESIAN_POINT('Ctrl Pts',(-42.6744089126314,-19.0167539117676,
10.9684916738292));
#24358=CARTESIAN_POINT('Ctrl Pts',(-44.9877964569987,-20.3088166768305,
11.5712994880388));
#24359=CARTESIAN_POINT('Ctrl Pts',(-47.301184001366,-21.6008794418934,12.1741073022483));
#24360=CARTESIAN_POINT('Ctrl Pts',(-49.6145715457333,-22.8929422069563,
11.5712994880388));
#24361=CARTESIAN_POINT('Ctrl Pts',(-39.4874365476045,-15.5447398754878,
0.));
#24362=CARTESIAN_POINT('Ctrl Pts',(-39.3984190448183,-15.7396610173495,
2.19648874705824));
#24363=CARTESIAN_POINT('Ctrl Pts',(-40.1762997089267,-16.3304812866725,
4.17545672685568));
#24364=CARTESIAN_POINT('Ctrl Pts',(-40.9541803730352,-16.9213015559956,
6.15442470665314));
#24365=CARTESIAN_POINT('Ctrl Pts',(-42.4272593902764,-17.8296082752022,
7.5239130403414));
#24366=CARTESIAN_POINT('Ctrl Pts',(-43.9003384075176,-18.7379149944087,
8.89340137402967));
#24367=CARTESIAN_POINT('Ctrl Pts',(-45.7592234042436,-19.8224134008056,
9.3821661014496));
#24368=CARTESIAN_POINT('Ctrl Pts',(-47.6181084009696,-20.9069118072026,
9.87093082886953));
#24369=CARTESIAN_POINT('Ctrl Pts',(-49.4769933976956,-21.9914102135995,
9.3821661014496));
#24370=CARTESIAN_POINT('Ctrl Pts',(-41.8481313484579,-15.3186586437006,
0.));
#24371=CARTESIAN_POINT('Ctrl Pts',(-41.7591138456717,-15.5135797855623,
1.72780310113343));
#24372=CARTESIAN_POINT('Ctrl Pts',(-42.3520162221171,-16.0199233014653,
3.28449990511991));
#24373=CARTESIAN_POINT('Ctrl Pts',(-42.9449185985625,-16.5262668173682,
4.84119670910639));
#24374=CARTESIAN_POINT('Ctrl Pts',(-44.0846782589591,-17.2823516867888,
5.91846432228298));
#24375=CARTESIAN_POINT('Ctrl Pts',(-45.2244379193557,-18.0384365562093,
6.99573193545956));
#24376=CARTESIAN_POINT('Ctrl Pts',(-46.6676804765722,-18.933117420683,7.38020429521639));
#24377=CARTESIAN_POINT('Ctrl Pts',(-48.1109230337888,-19.8277982851567,
7.76467665497322));
#24378=CARTESIAN_POINT('Ctrl Pts',(-49.5541655910053,-20.7224791496304,
7.38020429521639));
#24379=CARTESIAN_POINT('',(-34.8604849513958,-14.6113821712857,1.57949297810451E-9));
#24380=CARTESIAN_POINT('Origin',(-40.1321417817282,2.59935965651536,0.));
#24381=CARTESIAN_POINT('Ctrl Pts',(-34.8604849513682,-14.6113821714913,
3.13106096116309E-9));
#24382=CARTESIAN_POINT('Ctrl Pts',(-34.8537643034669,-14.6260983377862,
0.245038153335458));
#24383=CARTESIAN_POINT('Ctrl Pts',(-34.8527495154069,-14.6435771646298,
0.490791160521679));
#24384=CARTESIAN_POINT('Ctrl Pts',(-34.857531646356,-14.6638259110836,0.736766500725313));
#24385=CARTESIAN_POINT('Ctrl Pts',(-34.8622980778378,-14.6840081820399,
0.981934317700944));
#24386=CARTESIAN_POINT('Ctrl Pts',(-34.8728235332128,-14.7069422331334,
1.22732257376558));
#24387=CARTESIAN_POINT('Ctrl Pts',(-34.8891527148321,-14.7326128792078,
1.47243294816333));
#24388=CARTESIAN_POINT('Ctrl Pts',(-34.9054573041505,-14.7582448644192,
1.71717417803007));
#24389=CARTESIAN_POINT('Ctrl Pts',(-34.9275482079565,-14.7866052020689,
1.96163791541575));
#24390=CARTESIAN_POINT('Ctrl Pts',(-34.9554233023887,-14.8176563354397,
2.20532408778512));
#24391=CARTESIAN_POINT('Ctrl Pts',(-34.9832744897133,-14.8486808377692,
2.44880126242062));
#24392=CARTESIAN_POINT('Ctrl Pts',(-35.0168999484377,-14.8823914884391,
2.69150175431054));
#24393=CARTESIAN_POINT('Ctrl Pts',(-35.0562505641469,-14.9187287035023,
2.9329295186682));
#24394=CARTESIAN_POINT('Ctrl Pts',(-35.0955929476288,-14.9550583167477,
3.17430677585629));
#24395=CARTESIAN_POINT('Ctrl Pts',(-35.1406580326361,-14.994013334394,3.41441139318411));
#24396=CARTESIAN_POINT('Ctrl Pts',(-35.1913501978218,-15.0355127954204,
3.65275710614731));
#24397=CARTESIAN_POINT('Ctrl Pts',(-35.2421067311089,-15.0770649517994,
3.89140546668886));
#24398=CARTESIAN_POINT('Ctrl Pts',(-35.2985045323756,-15.1211679328247,
4.12829002081264));
#24399=CARTESIAN_POINT('Ctrl Pts',(-35.3604022296526,-15.1677200855875,
4.36293874377911));
#24400=CARTESIAN_POINT('Ctrl Pts',(-35.4223630872641,-15.21431974011,4.59782690201544));
#24401=CARTESIAN_POINT('Ctrl Pts',(-35.4898348974065,-15.2633734552294,
4.83047425895048));
#24402=CARTESIAN_POINT('Ctrl Pts',(-35.5626325521735,-15.3147603350322,
5.06042975959513));
#24403=CARTESIAN_POINT('Ctrl Pts',(-35.6356430387471,-15.3662974499286,
5.29105755998388));
#24404=CARTESIAN_POINT('Ctrl Pts',(-35.7140103401311,-15.4201812613942,
5.51897736305773));
#24405=CARTESIAN_POINT('Ctrl Pts',(-35.7975071039181,-15.4762725955038,
5.74376259354417));
#24406=CARTESIAN_POINT('Ctrl Pts',(-35.8507471233725,-15.5120380980667,
5.88709234072676));
#24407=CARTESIAN_POINT('Ctrl Pts',(-35.9060718261752,-15.5487007750605,
6.02914825314221));
#24408=CARTESIAN_POINT('Ctrl Pts',(-35.9634143689083,-15.5862213055883,
6.16982677023483));
#24409=CARTESIAN_POINT('Ctrl Pts',(-36.0533291627654,-15.6450546012013,
6.39041482339093));
#24410=CARTESIAN_POINT('Ctrl Pts',(-36.1486520067522,-15.7065142910194,
6.60890054011812));
#24411=CARTESIAN_POINT('Ctrl Pts',(-36.2492721362562,-15.7705155506319,
6.82480412008051));
#24412=CARTESIAN_POINT('Ctrl Pts',(-36.3496651101703,-15.8343723238086,
7.04022028559306));
#24413=CARTESIAN_POINT('Ctrl Pts',(-36.4553314094026,-15.9007591428905,
7.25306552029654));
#24414=CARTESIAN_POINT('Ctrl Pts',(-36.5661159087967,-15.9695695446609,
7.46287566269438));
#24415=CARTESIAN_POINT('Ctrl Pts',(-36.6767222213246,-16.0382692711121,
7.67234834441907));
#24416=CARTESIAN_POINT('Ctrl Pts',(-36.7924301575638,-16.1093847013534,
7.87879526533059));
#24417=CARTESIAN_POINT('Ctrl Pts',(-36.9130417770843,-16.1827888425359,
8.0817733461223));
#24418=CARTESIAN_POINT('Ctrl Pts',(-37.0335376654159,-16.2561225498036,
8.28455666214181));
#24419=CARTESIAN_POINT('Ctrl Pts',(-37.1589276519424,-16.3317404631321,
8.48387739272959));
#24420=CARTESIAN_POINT('Ctrl Pts',(-37.2889731283965,-16.4094964608255,
8.67931873611233));
#24421=CARTESIAN_POINT('Ctrl Pts',(-37.4190248596937,-16.4872561983765,
8.87476947970613));
#24422=CARTESIAN_POINT('Ctrl Pts',(-37.5537323016307,-16.5671540886076,
9.06634009532933));
#24423=CARTESIAN_POINT('Ctrl Pts',(-37.6928185909679,-16.6490263722368,
9.25364450341071));
#24424=CARTESIAN_POINT('Ctrl Pts',(-37.831955902738,-16.7309286899055,9.44101762226605));
#24425=CARTESIAN_POINT('Ctrl Pts',(-37.9754750005807,-16.8148066908797,
9.62412107875164));
#24426=CARTESIAN_POINT('Ctrl Pts',(-38.1230642366208,-16.9004810321079,
9.80260437466275));
#24427=CARTESIAN_POINT('Ctrl Pts',(-38.2708942212748,-16.9862951259321,
9.98137881379835));
#24428=CARTESIAN_POINT('Ctrl Pts',(-38.4228073220832,-17.0739112501833,
10.1555177270941));
#24429=CARTESIAN_POINT('Ctrl Pts',(-38.578460175403,-17.1631362396578,10.3247095747725));
#24430=CARTESIAN_POINT('Ctrl Pts',(-38.6234491187505,-17.1889252818182,
10.373611745775));
#24431=CARTESIAN_POINT('Ctrl Pts',(-38.6687503076433,-17.2148486564419,
10.4221009095729));
#24432=CARTESIAN_POINT('Ctrl Pts',(-38.7143550419872,-17.2409015314864,
10.4701702229062));
#24433=CARTESIAN_POINT('Ctrl Pts',(-38.9817677587449,-21.5951194116468,
0.));
#24434=CARTESIAN_POINT('Ctrl Pts',(-38.8927502559587,-21.7900405535085,
1.72780310113343));
#24435=CARTESIAN_POINT('Ctrl Pts',(-39.4856526324041,-22.2963840694115,
3.28449990511991));
#24436=CARTESIAN_POINT('Ctrl Pts',(-40.0785550088495,-22.8027275853144,
4.84119670910638));
#24437=CARTESIAN_POINT('Ctrl Pts',(-41.2183146692461,-23.558812454735,5.91846432228297));
#24438=CARTESIAN_POINT('Ctrl Pts',(-42.3580743296427,-24.3148973241555,
6.99573193545956));
#24439=CARTESIAN_POINT('Ctrl Pts',(-43.8013168868592,-25.2095781886292,
7.38020429521638));
#24440=CARTESIAN_POINT('Ctrl Pts',(-45.2445594440757,-26.1042590531029,
7.76467665497321));
#24441=CARTESIAN_POINT('Ctrl Pts',(-46.6878020012923,-26.9989399175765,
7.38020429521638));
#24442=CARTESIAN_POINT('Ctrl Pts',(-37.6067022235298,-19.6629735993422,
0.));
#24443=CARTESIAN_POINT('Ctrl Pts',(-37.5176847207437,-19.8578947412039,
2.19648874705822));
#24444=CARTESIAN_POINT('Ctrl Pts',(-38.2955653848521,-20.4487150105269,
4.17545672685568));
#24445=CARTESIAN_POINT('Ctrl Pts',(-39.0734460489605,-21.03953527985,6.15442470665314));
#24446=CARTESIAN_POINT('Ctrl Pts',(-40.5465250662017,-21.9478419990565,
7.5239130403414));
#24447=CARTESIAN_POINT('Ctrl Pts',(-42.0196040834429,-22.8561487182631,
8.89340137402967));
#24448=CARTESIAN_POINT('Ctrl Pts',(-43.8784890801689,-23.94064712466,9.3821661014496));
#24449=CARTESIAN_POINT('Ctrl Pts',(-45.7373740768949,-25.025145531057,9.87093082886954));
#24450=CARTESIAN_POINT('Ctrl Pts',(-47.5962590736209,-26.1096439374539,
9.3821661014496));
#24451=CARTESIAN_POINT('Ctrl Pts',(-35.8811107143583,-18.0362202038892,
0.));
#24452=CARTESIAN_POINT('Ctrl Pts',(-35.7920932115721,-18.2311413457509,
2.70899372698069));
#24453=CARTESIAN_POINT('Ctrl Pts',(-36.7722465384539,-18.9143364449667,
5.14971273833323));
#24454=CARTESIAN_POINT('Ctrl Pts',(-37.7523998653356,-19.5975315441826,
7.59043174968577));
#24455=CARTESIAN_POINT('Ctrl Pts',(-39.5899616265498,-20.6722919552115,
9.27946171175751));
#24456=CARTESIAN_POINT('Ctrl Pts',(-41.427523387764,-21.7470523662404,10.9684916738293));
#24457=CARTESIAN_POINT('Ctrl Pts',(-43.7409109321313,-23.0391151313033,
11.5712994880388));
#24458=CARTESIAN_POINT('Ctrl Pts',(-46.0542984764985,-24.3311778963662,
12.1741073022483));
#24459=CARTESIAN_POINT('Ctrl Pts',(-48.3676860208658,-25.6232406614291,
11.5712994880388));
#24460=CARTESIAN_POINT('Ctrl Pts',(-33.8713086176153,-16.7773762111442,
0.));
#24461=CARTESIAN_POINT('Ctrl Pts',(-33.7822911148291,-16.9722973530059,
3.24562220582793));
#24462=CARTESIAN_POINT('Ctrl Pts',(-34.9742380351172,-17.7522153454444,
6.16982677025168));
#24463=CARTESIAN_POINT('Ctrl Pts',(-36.1661849554053,-18.5321333378829,
9.09403133467541));
#24464=CARTESIAN_POINT('Ctrl Pts',(-38.3853855847801,-19.781182380126,11.1176436806954));
#24465=CARTESIAN_POINT('Ctrl Pts',(-40.604586214155,-21.0302314223691,13.1412560267153));
#24466=CARTESIAN_POINT('Ctrl Pts',(-43.3938696431043,-22.5396285557159,
13.8634749112255));
#24467=CARTESIAN_POINT('Ctrl Pts',(-46.1831530720537,-24.0490256890628,
14.5856937957357));
#24468=CARTESIAN_POINT('Ctrl Pts',(-48.9724365010031,-25.5584228224096,
13.8634749112255));
#24469=CARTESIAN_POINT('',(-33.8713086176152,-16.7773762111442,0.));
#24470=CARTESIAN_POINT('Ctrl Pts',(-33.8713086176152,-16.7773762111442,
0.));
#24471=CARTESIAN_POINT('Ctrl Pts',(-33.7822911148291,-16.9722973530059,
3.24562220582793));
#24472=CARTESIAN_POINT('Ctrl Pts',(-34.9742380351172,-17.7522153454444,
6.16982677025168));
#24473=CARTESIAN_POINT('Ctrl Pts',(-35.9693206543788,-18.4033205461167,
8.61106394926976));
#24474=CARTESIAN_POINT('Ctrl Pts',(-37.7050538275441,-19.3953958606403,
10.4489096280657));
#24475=CARTESIAN_POINT('Origin',(-24.3164988679738,-32.0320676419191,1.04083408558608E-14));
#24476=CARTESIAN_POINT('Ctrl Pts',(-33.8713086176153,-16.7773762111442,
0.));
#24477=CARTESIAN_POINT('Ctrl Pts',(-33.7822911148291,-16.9722973530059,
3.24562220582793));
#24478=CARTESIAN_POINT('Ctrl Pts',(-34.9742380351173,-17.7522153454444,
6.16982677025168));
#24479=CARTESIAN_POINT('Ctrl Pts',(-36.1661849554053,-18.5321333378829,
9.09403133467541));
#24480=CARTESIAN_POINT('Ctrl Pts',(-38.3853855847801,-19.781182380126,11.1176436806954));
#24481=CARTESIAN_POINT('Ctrl Pts',(-40.604586214155,-21.0302314223691,13.1412560267153));
#24482=CARTESIAN_POINT('Ctrl Pts',(-43.3938696431043,-22.5396285557159,
13.8634749112255));
#24483=CARTESIAN_POINT('Ctrl Pts',(-46.1831530720537,-24.0490256890628,
14.5856937957357));
#24484=CARTESIAN_POINT('Ctrl Pts',(-48.9724365010031,-25.5584228224096,
13.8634749112255));
#24485=CARTESIAN_POINT('Ctrl Pts',(-33.594993360669,-15.8658665409932,0.));
#24486=CARTESIAN_POINT('Ctrl Pts',(-33.5059758578829,-16.0607876828549,
3.38941559469372));
#24487=CARTESIAN_POINT('Ctrl Pts',(-34.7546743665351,-16.866623257281,6.44317352589574));
#24488=CARTESIAN_POINT('Ctrl Pts',(-36.0033728751872,-17.6724588317071,
9.49693145709774));
#24489=CARTESIAN_POINT('Ctrl Pts',(-38.3248363332021,-18.9682097429545,
11.6101975146502));
#24490=CARTESIAN_POINT('Ctrl Pts',(-40.6462997912169,-20.2639606542018,
13.7234635722027));
#24491=CARTESIAN_POINT('Ctrl Pts',(-43.5631028816989,-21.8315940656524,
14.4776794959001));
#24492=CARTESIAN_POINT('Ctrl Pts',(-46.4799059721808,-23.399227477103,15.2318954195974));
#24493=CARTESIAN_POINT('Ctrl Pts',(-49.3967090626628,-24.9668608885536,
14.4776794959001));
#24494=CARTESIAN_POINT('Ctrl Pts',(-33.9906638941719,-14.9994689250468,
0.));
#24495=CARTESIAN_POINT('Ctrl Pts',(-33.9016463913857,-15.1943900669085,
3.38941559469371));
#24496=CARTESIAN_POINT('Ctrl Pts',(-35.1503449000379,-16.0002256413346,
6.44317352589574));
#24497=CARTESIAN_POINT('Ctrl Pts',(-36.3990434086901,-16.8060612157607,
9.49693145709774));
#24498=CARTESIAN_POINT('Ctrl Pts',(-38.7205068667049,-18.1018121270081,
11.6101975146502));
#24499=CARTESIAN_POINT('Ctrl Pts',(-41.0419703247197,-19.3975630382554,
13.7234635722027));
#24500=CARTESIAN_POINT('Ctrl Pts',(-43.9587734152017,-20.965196449706,14.4776794959001));
#24501=CARTESIAN_POINT('Ctrl Pts',(-46.8755765056837,-22.5328298611566,
15.2318954195974));
#24502=CARTESIAN_POINT('Ctrl Pts',(-49.7923795961656,-24.1004632726072,
14.4776794959001));
#24503=CARTESIAN_POINT('Ctrl Pts',(-34.8604849513723,-14.6113821712782,
0.));
#24504=CARTESIAN_POINT('Ctrl Pts',(-34.7714674485862,-14.8063033131399,
3.24562220582793));
#24505=CARTESIAN_POINT('Ctrl Pts',(-35.9634143688743,-15.5862213055784,
6.16982677025167));
#24506=CARTESIAN_POINT('Ctrl Pts',(-37.1553612891624,-16.366139298017,9.09403133467541));
#24507=CARTESIAN_POINT('Ctrl Pts',(-39.3745619185372,-17.6151883402601,
11.1176436806954));
#24508=CARTESIAN_POINT('Ctrl Pts',(-41.593762547912,-18.8642373825032,13.1412560267153));
#24509=CARTESIAN_POINT('Ctrl Pts',(-44.3830459768614,-20.37363451585,13.8634749112255));
#24510=CARTESIAN_POINT('Ctrl Pts',(-47.1723294058108,-21.8830316491968,
14.5856937957357));
#24511=CARTESIAN_POINT('Ctrl Pts',(-49.9616128347602,-23.3924287825436,
13.8634749112255));
#24512=CARTESIAN_POINT('',(-33.9565644528763,-15.5074379108284,-5.72595023222876E-30));
#24513=CARTESIAN_POINT('Origin',(-35.5938999782224,-16.2551894587637,0.));
#24514=CARTESIAN_POINT('Origin',(-35.5938999782224,-16.2551894587637,0.));
#24515=CARTESIAN_POINT('Ctrl Pts',(-36.5850719698905,-9.5014950906651,0.));
#24516=CARTESIAN_POINT('Ctrl Pts',(-36.5247007077102,-9.7071007278682,3.24562220582792));
#24517=CARTESIAN_POINT('Ctrl Pts',(-37.8155092299557,-10.3094485465015,
6.16982677025168));
#24518=CARTESIAN_POINT('Ctrl Pts',(-39.1063177522011,-10.9117963651347,
9.09403133467541));
#24519=CARTESIAN_POINT('Ctrl Pts',(-41.4806883314342,-11.8323067104423,
11.1176436806954));
#24520=CARTESIAN_POINT('Ctrl Pts',(-43.8550589106673,-12.7528170557499,
13.1412560267153));
#24521=CARTESIAN_POINT('Ctrl Pts',(-46.8307610650469,-13.8498942825609,
13.8634749112255));
#24522=CARTESIAN_POINT('Ctrl Pts',(-49.8064632194266,-14.9469715093719,
14.5856937957357));
#24523=CARTESIAN_POINT('Ctrl Pts',(-52.7821653738063,-16.044048736183,13.8634749112255));
#24524=CARTESIAN_POINT('Ctrl Pts',(-38.928346550052,-9.86626475512752,0.));
#24525=CARTESIAN_POINT('Ctrl Pts',(-38.8679752878717,-10.0718703923306,
2.7089937269807));
#24526=CARTESIAN_POINT('Ctrl Pts',(-39.9353808672041,-10.6086211883242,
5.14971273833324));
#24527=CARTESIAN_POINT('Ctrl Pts',(-41.0027864465366,-11.1453719843179,
7.59043174968579));
#24528=CARTESIAN_POINT('Ctrl Pts',(-42.9745988326451,-11.9476805791747,
9.27946171175752));
#24529=CARTESIAN_POINT('Ctrl Pts',(-44.9464112187534,-12.7499891740315,
10.9684916738293));
#24530=CARTESIAN_POINT('Ctrl Pts',(-47.4201315169973,-13.6996712289066,
11.5712994880388));
#24531=CARTESIAN_POINT('Ctrl Pts',(-49.8938518152412,-14.6493532837818,
12.1741073022483));
#24532=CARTESIAN_POINT('Ctrl Pts',(-52.367572113485,-15.599035338657,11.5712994880388));
#24533=CARTESIAN_POINT('Ctrl Pts',(-41.297758521112,-9.76686869112041,0.));
#24534=CARTESIAN_POINT('Ctrl Pts',(-41.2373872589317,-9.97247432832351,
2.19648874705824));
#24535=CARTESIAN_POINT('Ctrl Pts',(-42.0914327105681,-10.4465769382888,
4.17545672685568));
#24536=CARTESIAN_POINT('Ctrl Pts',(-42.9454781622045,-10.9206795482542,
6.15442470665314));
#24537=CARTESIAN_POINT('Ctrl Pts',(-44.5328288829012,-11.6101000126269,
7.5239130403414));
#24538=CARTESIAN_POINT('Ctrl Pts',(-46.1201796035978,-12.2995204769996,
8.89340137402967));
#24539=CARTESIAN_POINT('Ctrl Pts',(-48.114484046662,-13.1084333356593,9.3821661014496));
#24540=CARTESIAN_POINT('Ctrl Pts',(-50.1087884897262,-13.917346194319,9.87093082886953));
#24541=CARTESIAN_POINT('Ctrl Pts',(-52.1030929327903,-14.7262590529787,
9.3821661014496));
#24542=CARTESIAN_POINT('Ctrl Pts',(-43.6022501387951,-9.20712674149459,
0.));
#24543=CARTESIAN_POINT('Ctrl Pts',(-43.5418788766148,-9.4127323786977,1.72780310113343));
#24544=CARTESIAN_POINT('Ctrl Pts',(-44.2008065573391,-9.82954324188014,
3.28449990511991));
#24545=CARTESIAN_POINT('Ctrl Pts',(-44.8597342380633,-10.2463541050626,
4.84119670910639));
#24546=CARTESIAN_POINT('Ctrl Pts',(-46.0954948844273,-10.8325384089571,
5.91846432228298));
#24547=CARTESIAN_POINT('Ctrl Pts',(-47.3312555307912,-11.4187227128515,
6.99573193545956));
#24548=CARTESIAN_POINT('Ctrl Pts',(-48.887134322293,-12.0989021850287,7.38020429521639));
#24549=CARTESIAN_POINT('Ctrl Pts',(-50.4430131137947,-12.7790816572059,
7.76467665497321));
#24550=CARTESIAN_POINT('Ctrl Pts',(-51.9988919052965,-13.4592611293832,
7.38020429521639));
#24551=CARTESIAN_POINT('',(-36.5850719699045,-9.50149509067428,1.57948780722887E-9));
#24552=CARTESIAN_POINT('Origin',(-39.3537269950291,8.28430119040637,0.));
#24553=CARTESIAN_POINT('Ctrl Pts',(-36.5850719699168,-9.5014950908766,3.13105117804127E-9));
#24554=CARTESIAN_POINT('Ctrl Pts',(-36.580514057347,-9.51701791573671,0.245038153335549));
#24555=CARTESIAN_POINT('Ctrl Pts',(-36.5819970947817,-9.53446325272415,
0.490791160521871));
#24556=CARTESIAN_POINT('Ctrl Pts',(-36.5896122476098,-9.55382532794269,
0.736766500725606));
#24557=CARTESIAN_POINT('Ctrl Pts',(-36.5972024003189,-9.57312383855566,
0.981934317701291));
#24558=CARTESIAN_POINT('Ctrl Pts',(-36.610884577507,-9.59432652559767,1.22732257376598));
#24559=CARTESIAN_POINT('Ctrl Pts',(-36.6307008654466,-9.61741199666781,
1.47243294816378));
#24560=CARTESIAN_POINT('Ctrl Pts',(-36.650487309385,-9.64046270023612,1.71717417803054));
#24561=CARTESIAN_POINT('Ctrl Pts',(-36.6763894565087,-9.66539050713831,
1.96163791541623));
#24562=CARTESIAN_POINT('Ctrl Pts',(-36.7083998596961,-9.69215854518743,
2.20532408778562));
#24563=CARTESIAN_POINT('Ctrl Pts',(-36.7403828091233,-9.71890362559706,
2.44880126242105));
#24564=CARTESIAN_POINT('Ctrl Pts',(-36.7784635349599,-9.7474857487296,2.6915017543109));
#24565=CARTESIAN_POINT('Ctrl Pts',(-36.8225849430251,-9.7778529268268,2.93292951866849));
#24566=CARTESIAN_POINT('Ctrl Pts',(-36.8666971208038,-9.8082137520498,3.17430677585641));
#24567=CARTESIAN_POINT('Ctrl Pts',(-36.9168473852604,-9.8403588335004,3.41441139318406));
#24568=CARTESIAN_POINT('Ctrl Pts',(-36.9729295663809,-9.87422164256066,
3.65275710614709));
#24569=CARTESIAN_POINT('Ctrl Pts',(-37.029082959759,-9.90812745007487,3.89140546668862));
#24570=CARTESIAN_POINT('Ctrl Pts',(-37.0911832213397,-9.94375528237833,
4.1282900208124));
#24571=CARTESIAN_POINT('Ctrl Pts',(-37.1590759513992,-9.98102464057122,
4.36293874377885));
#24572=CARTESIAN_POINT('Ctrl Pts',(-37.2270379591174,-10.0183320283716,
4.59782690201515));
#24573=CARTESIAN_POINT('Ctrl Pts',(-37.3008040750528,-10.0572842076522,
4.83047425895016));
#24574=CARTESIAN_POINT('Ctrl Pts',(-37.3801738701483,-10.0977878566476,
5.06042975959479));
#24575=CARTESIAN_POINT('Ctrl Pts',(-37.4597757114126,-10.1384099224358,
5.29105755998349));
#24576=CARTESIAN_POINT('Ctrl Pts',(-37.545013812579,-10.1805924445722,5.51897736305729));
#24577=CARTESIAN_POINT('Ctrl Pts',(-37.6356433288454,-10.2242300213429,
5.74376259354369));
#24578=CARTESIAN_POINT('Ctrl Pts',(-37.6934314033805,-10.252054637901,5.88709234072645));
#24579=CARTESIAN_POINT('Ctrl Pts',(-37.7534106234274,-10.2804706155745,
6.02914825314205));
#24580=CARTESIAN_POINT('Ctrl Pts',(-37.8155092299907,-10.3094485465064,
6.16982677023484));
#24581=CARTESIAN_POINT('Ctrl Pts',(-37.912881671843,-10.3548867946545,6.39041482339099));
#24582=CARTESIAN_POINT('Ctrl Pts',(-38.0159808925391,-10.4021550583221,
6.60890054011821));
#24583=CARTESIAN_POINT('Ctrl Pts',(-38.124685183118,-10.4511851399366,6.82480412008066));
#24584=CARTESIAN_POINT('Ctrl Pts',(-38.2331440676597,-10.5001045333898,
7.0402202855931));
#24585=CARTESIAN_POINT('Ctrl Pts',(-38.3471826657451,-10.5507777480891,
7.25306552029649));
#24586=CARTESIAN_POINT('Ctrl Pts',(-38.4666322798727,-10.6031214810715,
7.46287566269424));
#24587=CARTESIAN_POINT('Ctrl Pts',(-38.5858897700796,-10.6553810238848,
7.67234834441891));
#24588=CARTESIAN_POINT('Ctrl Pts',(-38.7105407473184,-10.7093056453534,
7.87879526533041));
#24589=CARTESIAN_POINT('Ctrl Pts',(-38.8403712129408,-10.7647978150927,
8.0817733461221));
#24590=CARTESIAN_POINT('Ctrl Pts',(-38.9700771015593,-10.8202367380982,
8.28455666214101));
#24591=CARTESIAN_POINT('Ctrl Pts',(-39.1049523499259,-10.8772401144473,
8.48387739272821));
#24592=CARTESIAN_POINT('Ctrl Pts',(-39.2447399831758,-10.9356972672492,
8.67931873611038));
#24593=CARTESIAN_POINT('Ctrl Pts',(-39.3845343398413,-10.9941572316855,
8.87476947970425));
#24594=CARTESIAN_POINT('Ctrl Pts',(-39.5292413095781,-11.0540710087837,
9.0663400953275));
#24595=CARTESIAN_POINT('Ctrl Pts',(-39.6785635418394,-11.1153159078427,
9.25364450340895));
#24596=CARTESIAN_POINT('Ctrl Pts',(-39.8279405514878,-11.1765832739883,
9.44101762226374));
#24597=CARTESIAN_POINT('Ctrl Pts',(-39.9819359159948,-11.2391826206559,
9.62412107874879));
#24598=CARTESIAN_POINT('Ctrl Pts',(-40.1402156364337,-11.3029807823644,
9.80260437465941));
#24599=CARTESIAN_POINT('Ctrl Pts',(-40.2987535438811,-11.3668830120892,
9.98137881379501));
#24600=CARTESIAN_POINT('Ctrl Pts',(-40.4615894629167,-11.4319878421543,
10.1555177270907));
#24601=CARTESIAN_POINT('Ctrl Pts',(-40.6283560345695,-11.4981529392408,
10.3247095747691));
#24602=CARTESIAN_POINT('Ctrl Pts',(-40.6765572187095,-11.5172768919413,
10.3736117457744));
#24603=CARTESIAN_POINT('Ctrl Pts',(-40.7250865876881,-11.5364893726199,
10.4221009095751));
#24604=CARTESIAN_POINT('Ctrl Pts',(-40.7739348422943,-11.5557868365701,
10.4701702229111));
#24605=CARTESIAN_POINT('Ctrl Pts',(-41.6582954965893,-15.8276282594346,
0.));
#24606=CARTESIAN_POINT('Ctrl Pts',(-41.597924234409,-16.0332338966377,1.72780310113342));
#24607=CARTESIAN_POINT('Ctrl Pts',(-42.2568519151332,-16.4500447598202,
3.28449990511991));
#24608=CARTESIAN_POINT('Ctrl Pts',(-42.9157795958575,-16.8668556230026,
4.84119670910638));
#24609=CARTESIAN_POINT('Ctrl Pts',(-44.1515402422214,-17.4530399268971,
5.91846432228298));
#24610=CARTESIAN_POINT('Ctrl Pts',(-45.3873008885854,-18.0392242307915,
6.99573193545957));
#24611=CARTESIAN_POINT('Ctrl Pts',(-46.9431796800871,-18.7194037029688,
7.3802042952164));
#24612=CARTESIAN_POINT('Ctrl Pts',(-48.4990584715889,-19.399583175146,7.76467665497322));
#24613=CARTESIAN_POINT('Ctrl Pts',(-50.0549372630907,-20.0797626473232,
7.3802042952164));
#24614=CARTESIAN_POINT('Ctrl Pts',(-40.0222531270434,-14.1108411348343,
0.));
#24615=CARTESIAN_POINT('Ctrl Pts',(-39.9618818648631,-14.3164467720375,
2.19648874705823));
#24616=CARTESIAN_POINT('Ctrl Pts',(-40.8159273164995,-14.7905493820028,
4.17545672685568));
#24617=CARTESIAN_POINT('Ctrl Pts',(-41.6699727681359,-15.2646519919681,
6.15442470665314));
#24618=CARTESIAN_POINT('Ctrl Pts',(-43.2573234888326,-15.9540724563408,
7.5239130403414));
#24619=CARTESIAN_POINT('Ctrl Pts',(-44.8446742095292,-16.6434929207135,
8.89340137402967));
#24620=CARTESIAN_POINT('Ctrl Pts',(-46.8389786525934,-17.4524057793732,
9.3821661014496));
#24621=CARTESIAN_POINT('Ctrl Pts',(-48.8332830956575,-18.2613186380329,
9.87093082886954));
#24622=CARTESIAN_POINT('Ctrl Pts',(-50.8275875387217,-19.0702314966926,
9.38216610144961));
#24623=CARTESIAN_POINT('Ctrl Pts',(-38.0827145049533,-12.7462230199159,
0.));
#24624=CARTESIAN_POINT('Ctrl Pts',(-38.022343242773,-12.951828657119,2.70899372698069));
#24625=CARTESIAN_POINT('Ctrl Pts',(-39.0897488221055,-13.4885794531126,
5.14971273833323));
#24626=CARTESIAN_POINT('Ctrl Pts',(-40.157154401438,-14.0253302491062,7.59043174968578));
#24627=CARTESIAN_POINT('Ctrl Pts',(-42.1289667875464,-14.827638843963,9.27946171175752));
#24628=CARTESIAN_POINT('Ctrl Pts',(-44.1007791736548,-15.6299474388198,
10.9684916738293));
#24629=CARTESIAN_POINT('Ctrl Pts',(-46.5744994718987,-16.579629493695,11.5712994880388));
#24630=CARTESIAN_POINT('Ctrl Pts',(-49.0482197701425,-17.5293115485701,
12.1741073022483));
#24631=CARTESIAN_POINT('Ctrl Pts',(-51.5219400683864,-18.4789936034453,
11.5712994880388));
#24632=CARTESIAN_POINT('Ctrl Pts',(-35.914217116421,-11.7862169042732,0.));
#24633=CARTESIAN_POINT('Ctrl Pts',(-35.8538458542407,-11.9918225414763,
3.24562220582792));
#24634=CARTESIAN_POINT('Ctrl Pts',(-37.1446543764862,-12.5941703601095,
6.16982677025167));
#24635=CARTESIAN_POINT('Ctrl Pts',(-38.4354628987316,-13.1965181787427,
9.09403133467541));
#24636=CARTESIAN_POINT('Ctrl Pts',(-40.8098334779647,-14.1170285240504,
11.1176436806954));
#24637=CARTESIAN_POINT('Ctrl Pts',(-43.1842040571977,-15.037538869358,13.1412560267153));
#24638=CARTESIAN_POINT('Ctrl Pts',(-46.1599062115774,-16.134616096169,13.8634749112255));
#24639=CARTESIAN_POINT('Ctrl Pts',(-49.1356083659571,-17.23169332298,14.5856937957357));
#24640=CARTESIAN_POINT('Ctrl Pts',(-52.1113105203367,-18.328770549791,13.8634749112255));
#24641=CARTESIAN_POINT('',(-35.914217116421,-11.7862169042732,0.));
#24642=CARTESIAN_POINT('Ctrl Pts',(-35.914217116421,-11.7862169042732,0.));
#24643=CARTESIAN_POINT('Ctrl Pts',(-35.8538458542407,-11.9918225414763,
3.24562220582792));
#24644=CARTESIAN_POINT('Ctrl Pts',(-37.1446543764862,-12.5941703601095,
6.16982677025167));
#24645=CARTESIAN_POINT('Ctrl Pts',(-38.2222704208069,-13.0970332266264,
8.61106394926975));
#24646=CARTESIAN_POINT('Ctrl Pts',(-40.0815233709313,-13.831990059078,10.4489096280657));
#24647=CARTESIAN_POINT('Origin',(-28.6276304970126,-28.2454287759837,0.));
#24648=CARTESIAN_POINT('Ctrl Pts',(-35.914217116421,-11.7862169042732,0.));
#24649=CARTESIAN_POINT('Ctrl Pts',(-35.8538458542407,-11.9918225414763,
3.24562220582792));
#24650=CARTESIAN_POINT('Ctrl Pts',(-37.1446543764862,-12.5941703601095,
6.16982677025167));
#24651=CARTESIAN_POINT('Ctrl Pts',(-38.4354628987316,-13.1965181787427,
9.09403133467541));
#24652=CARTESIAN_POINT('Ctrl Pts',(-40.8098334779647,-14.1170285240504,
11.1176436806954));
#24653=CARTESIAN_POINT('Ctrl Pts',(-43.1842040571977,-15.037538869358,13.1412560267153));
#24654=CARTESIAN_POINT('Ctrl Pts',(-46.1599062115774,-16.134616096169,13.8634749112255));
#24655=CARTESIAN_POINT('Ctrl Pts',(-49.1356083659571,-17.23169332298,14.5856937957357));
#24656=CARTESIAN_POINT('Ctrl Pts',(-52.1113105203367,-18.328770549791,13.8634749112255));
#24657=CARTESIAN_POINT('Ctrl Pts',(-35.5109929990848,-10.9233088493806,
0.));
#24658=CARTESIAN_POINT('Ctrl Pts',(-35.4506217369044,-11.1289144865837,
3.38941559469374));
#24659=CARTESIAN_POINT('Ctrl Pts',(-36.8012926546624,-11.7488394904702,
6.44317352589574));
#24660=CARTESIAN_POINT('Ctrl Pts',(-38.1519635724204,-12.3687644943567,
9.49693145709775));
#24661=CARTESIAN_POINT('Ctrl Pts',(-40.6342024610831,-13.3209478330614,
11.6101975146502));
#24662=CARTESIAN_POINT('Ctrl Pts',(-43.1164413497459,-14.273131171766,13.7234635722027));
#24663=CARTESIAN_POINT('Ctrl Pts',(-46.2266530858719,-15.4097039753318,
14.4776794959001));
#24664=CARTESIAN_POINT('Ctrl Pts',(-49.336864821998,-16.5462767788976,15.2318954195974));
#24665=CARTESIAN_POINT('Ctrl Pts',(-52.447076558124,-17.6828495824634,14.4776794959001));
#24666=CARTESIAN_POINT('Ctrl Pts',(-35.7793349404726,-10.0094201239374,
0.));
#24667=CARTESIAN_POINT('Ctrl Pts',(-35.7189636782922,-10.2150257611405,
3.38941559469374));
#24668=CARTESIAN_POINT('Ctrl Pts',(-37.0696345960502,-10.834950765027,6.44317352589574));
#24669=CARTESIAN_POINT('Ctrl Pts',(-38.4203055138082,-11.4548757689135,
9.49693145709775));
#24670=CARTESIAN_POINT('Ctrl Pts',(-40.9025444024709,-12.4070591076181,
11.6101975146502));
#24671=CARTESIAN_POINT('Ctrl Pts',(-43.3847832911337,-13.3592424463228,
13.7234635722027));
#24672=CARTESIAN_POINT('Ctrl Pts',(-46.4949950272597,-14.4958152498886,
14.4776794959001));
#24673=CARTESIAN_POINT('Ctrl Pts',(-49.6052067633858,-15.6323880534543,
15.2318954195974));
#24674=CARTESIAN_POINT('Ctrl Pts',(-52.7154184995118,-16.7689608570201,
14.4776794959001));
#24675=CARTESIAN_POINT('Ctrl Pts',(-36.5850719698906,-9.5014950906651,0.));
#24676=CARTESIAN_POINT('Ctrl Pts',(-36.5247007077102,-9.7071007278682,3.24562220582792));
#24677=CARTESIAN_POINT('Ctrl Pts',(-37.8155092299557,-10.3094485465015,
6.16982677025167));
#24678=CARTESIAN_POINT('Ctrl Pts',(-39.1063177522011,-10.9117963651347,
9.09403133467541));
#24679=CARTESIAN_POINT('Ctrl Pts',(-41.4806883314342,-11.8323067104423,
11.1176436806954));
#24680=CARTESIAN_POINT('Ctrl Pts',(-43.8550589106672,-12.7528170557499,
13.1412560267153));
#24681=CARTESIAN_POINT('Ctrl Pts',(-46.8307610650469,-13.8498942825609,
13.8634749112255));
#24682=CARTESIAN_POINT('Ctrl Pts',(-49.8064632194266,-14.9469715093719,
14.5856937957357));
#24683=CARTESIAN_POINT('Ctrl Pts',(-52.7821653738063,-16.044048736183,13.8634749112255));
#24684=CARTESIAN_POINT('',(-35.817874106385,-10.5170715743355,-8.26137723578747E-30));
#24685=CARTESIAN_POINT('Origin',(-37.5449600575354,-11.024194949205,0.));
#24686=CARTESIAN_POINT('Origin',(-37.5449600575354,-11.024194949205,0.));
#24687=CARTESIAN_POINT('Ctrl Pts',(-37.5648924257372,-4.19818497005524,
0.));
#24688=CARTESIAN_POINT('Ctrl Pts',(-37.5343963889643,-4.410289564744,3.24562220582793));
#24689=CARTESIAN_POINT('Ctrl Pts',(-38.8977893740386,-4.82280514501228,
6.16982677025168));
#24690=CARTESIAN_POINT('Ctrl Pts',(-40.2611823591128,-5.23532072528053,
9.09403133467541));
#24691=CARTESIAN_POINT('Ctrl Pts',(-42.7423875503303,-5.80855343755483,
11.1176436806954));
#24692=CARTESIAN_POINT('Ctrl Pts',(-45.2235927415478,-6.38178614982912,
13.1412560267153));
#24693=CARTESIAN_POINT('Ctrl Pts',(-48.3251369067109,-7.04421014147591,
13.8634749112255));
#24694=CARTESIAN_POINT('Ctrl Pts',(-51.4266810718741,-7.70663413312271,
14.5856937957357));
#24695=CARTESIAN_POINT('Ctrl Pts',(-54.5282252370373,-8.36905812476951,
13.8634749112255));
#24696=CARTESIAN_POINT('Ctrl Pts',(-39.9362279852005,-4.22575906238229,
-1.05434036998093E-14));
#24697=CARTESIAN_POINT('Ctrl Pts',(-39.9057319484276,-4.43786365707106,
2.70899372698069));
#24698=CARTESIAN_POINT('Ctrl Pts',(-41.0386604807592,-4.8172434514975,5.14971273833323));
#24699=CARTESIAN_POINT('Ctrl Pts',(-42.1715890130907,-5.19662324592393,
7.59043174968578));
#24700=CARTESIAN_POINT('Ctrl Pts',(-44.2375116101495,-5.71014733528427,
9.27946171175751));
#24701=CARTESIAN_POINT('Ctrl Pts',(-46.3034342072083,-6.22367142464463,
10.9684916738292));
#24702=CARTESIAN_POINT('Ctrl Pts',(-48.8871294476768,-6.81163998135168,
11.5712994880388));
#24703=CARTESIAN_POINT('Ctrl Pts',(-51.4708246881452,-7.39960853805875,
12.1741073022483));
#24704=CARTESIAN_POINT('Ctrl Pts',(-54.0545199286137,-7.9875770947658,11.5712994880388));
#24705=CARTESIAN_POINT('Ctrl Pts',(-42.2673772240309,-3.79017222552529,
0.));
#24706=CARTESIAN_POINT('Ctrl Pts',(-42.2368811872581,-4.00227682021405,
2.19648874705824));
#24707=CARTESIAN_POINT('Ctrl Pts',(-43.1497055238908,-4.35001040888178,
4.17545672685567));
#24708=CARTESIAN_POINT('Ctrl Pts',(-44.0625298605235,-4.6977439975495,6.15442470665313));
#24709=CARTESIAN_POINT('Ctrl Pts',(-45.7318384015437,-5.15424359455821,
7.5239130403414));
#24710=CARTESIAN_POINT('Ctrl Pts',(-47.4011469425639,-5.61074319156689,
8.89340137402966));
#24711=CARTESIAN_POINT('Ctrl Pts',(-49.4902725446046,-6.1276033693991,9.3821661014496));
#24712=CARTESIAN_POINT('Ctrl Pts',(-51.5793981466452,-6.64446354723128,
9.87093082886953));
#24713=CARTESIAN_POINT('Ctrl Pts',(-53.6685237486859,-7.16132372506348,
9.3821661014496));
#24714=CARTESIAN_POINT('Ctrl Pts',(-44.4687528548128,-2.90816428999269,
0.));
#24715=CARTESIAN_POINT('Ctrl Pts',(-44.4382568180399,-3.12026888468146,
1.72780310113343));
#24716=CARTESIAN_POINT('Ctrl Pts',(-45.149795935654,-3.43906202795228,3.28449990511991));
#24717=CARTESIAN_POINT('Ctrl Pts',(-45.8613350532681,-3.75785517122311,
4.84119670910638));
#24718=CARTESIAN_POINT('Ctrl Pts',(-47.1679401624789,-4.16220588758012,
5.91846432228298));
#24719=CARTESIAN_POINT('Ctrl Pts',(-48.4745452716896,-4.56655660393713,
6.99573193545956));
#24720=CARTESIAN_POINT('Ctrl Pts',(-50.1113870920655,-5.01838819123999,
7.38020429521639));
#24721=CARTESIAN_POINT('Ctrl Pts',(-51.7482289124415,-5.47021977854284,
7.76467665497321));
#24722=CARTESIAN_POINT('Ctrl Pts',(-53.3850707328175,-5.9220513658457,7.38020429521639));
#24723=CARTESIAN_POINT('',(-37.5648924257618,-4.19818497005579,1.57948609960414E-9));
#24724=CARTESIAN_POINT('Origin',(-37.7741838134884,13.8005982420126,0.));
#24725=CARTESIAN_POINT('Ctrl Pts',(-37.5648924257933,-4.19818497026086,
3.13104702311909E-9));
#24726=CARTESIAN_POINT('Ctrl Pts',(-37.562590034511,-4.21419845373618,0.245038153335525));
#24727=CARTESIAN_POINT('Ctrl Pts',(-37.5665407070749,-4.23125516411452,
0.490791160521828));
#24728=CARTESIAN_POINT('Ctrl Pts',(-37.5768338592308,-4.24933641208198,
0.736766500725544));
#24729=CARTESIAN_POINT('Ctrl Pts',(-37.5870932195462,-4.26735830032779,
0.981934317701182));
#24730=CARTESIAN_POINT('Ctrl Pts',(-37.6036535888759,-4.28639799775371,
1.22732257376582));
#24731=CARTESIAN_POINT('Ctrl Pts',(-37.6265535806588,-4.30642834020156,
1.47243294816358));
#24732=CARTESIAN_POINT('Ctrl Pts',(-37.649419084278,-4.32642851627481,1.71717417803032));
#24733=CARTESIAN_POINT('Ctrl Pts',(-37.6786051816996,-4.34741633416683,
1.96163791541599));
#24734=CARTESIAN_POINT('Ctrl Pts',(-37.7140992541435,-4.36935635683226,
2.20532408778536));
#24735=CARTESIAN_POINT('Ctrl Pts',(-37.7495628850543,-4.39127756261129,
2.44880126242071));
#24736=CARTESIAN_POINT('Ctrl Pts',(-37.7913236642409,-4.41414930860358,
2.69150175431049));
#24737=CARTESIAN_POINT('Ctrl Pts',(-37.8393176800295,-4.43792826156041,
2.93292951866801));
#24738=CARTESIAN_POINT('Ctrl Pts',(-37.8873016553743,-4.46170223991287,
3.17430677585588));
#24739=CARTESIAN_POINT('Ctrl Pts',(-37.9415161845174,-4.48638300400817,
3.41441139318348));
#24740=CARTESIAN_POINT('Ctrl Pts',(-38.0018467100928,-4.51191981196215,
3.65275710614646));
#24741=CARTESIAN_POINT('Ctrl Pts',(-38.0622538424057,-4.5374890461469,3.89140546668795));
#24742=CARTESIAN_POINT('Ctrl Pts',(-38.1287923820569,-4.56391644980501,
4.12829002081169));
#24743=CARTESIAN_POINT('Ctrl Pts',(-38.2012980447014,-4.59114431677112,
4.36293874377811));
#24744=CARTESIAN_POINT('Ctrl Pts',(-38.2738776920354,-4.61839996701937,
4.59782690201448));
#24745=CARTESIAN_POINT('Ctrl Pts',(-38.3524364483672,-4.64645765641992,
4.83047425894955));
#24746=CARTESIAN_POINT('Ctrl Pts',(-38.4367626436466,-4.67525353711722,
5.06042975959425));
#24747=CARTESIAN_POINT('Ctrl Pts',(-38.5213353756662,-4.70413360568203,
5.29105755998295));
#24748=CARTESIAN_POINT('Ctrl Pts',(-38.6117090746818,-4.73375612398307,
5.51897736305675));
#24749=CARTESIAN_POINT('Ctrl Pts',(-38.7076263878303,-4.7640516081922,5.74376259354315));
#24750=CARTESIAN_POINT('Ctrl Pts',(-38.7687861188958,-4.78336890979197,
5.88709234072609));
#24751=CARTESIAN_POINT('Ctrl Pts',(-38.8321988522325,-4.80295972078441,
6.02914825314188));
#24752=CARTESIAN_POINT('Ctrl Pts',(-38.8977893740739,-4.82280514501219,
6.16982677023484));
#24753=CARTESIAN_POINT('Ctrl Pts',(-39.0006372418043,-4.8539233539962,6.39041482339094));
#24754=CARTESIAN_POINT('Ctrl Pts',(-39.1094140363897,-4.88603794597538,
6.60890054011812));
#24755=CARTESIAN_POINT('Ctrl Pts',(-39.2239895821647,-4.91909873852119,
6.82480412008052));
#24756=CARTESIAN_POINT('Ctrl Pts',(-39.3383064672143,-4.95208489447222,
7.04022028559309));
#24757=CARTESIAN_POINT('Ctrl Pts',(-39.458395867156,-4.98601294426717,7.25306552029659));
#24758=CARTESIAN_POINT('Ctrl Pts',(-39.5840789463381,-5.02082444100485,
7.46287566269445));
#24759=CARTESIAN_POINT('Ctrl Pts',(-39.7095598756334,-5.05557994659266,
7.67234834441904));
#24760=CARTESIAN_POINT('Ctrl Pts',(-39.840616359439,-5.0912160095013,7.87879526533046));
#24761=CARTESIAN_POINT('Ctrl Pts',(-39.9770226972832,-5.12766654724775,
8.08177334612208));
#24762=CARTESIAN_POINT('Ctrl Pts',(-40.1132981483379,-5.16408210939161,
8.28455666214132));
#24763=CARTESIAN_POINT('Ctrl Pts',(-40.2549129874365,-5.20131052440325,
8.48387739272884));
#24764=CARTESIAN_POINT('Ctrl Pts',(-40.4015971043843,-5.23927881325933,
8.67931873611132));
#24765=CARTESIAN_POINT('Ctrl Pts',(-40.5482882764499,-5.27724892828962,
8.87476947970519));
#24766=CARTESIAN_POINT('Ctrl Pts',(-40.7000489573831,-5.31595892053044,
9.06634009532845));
#24767=CARTESIAN_POINT('Ctrl Pts',(-40.8565673625296,-5.35532966548994,
9.2536445034099));
#24768=CARTESIAN_POINT('Ctrl Pts',(-41.0131431849084,-5.39471485321869,
9.44101762226499));
#24769=CARTESIAN_POINT('Ctrl Pts',(-41.174479914545,-5.4347612034034,9.62412107875033));
#24770=CARTESIAN_POINT('Ctrl Pts',(-41.3402280007163,-5.47538443899895,
9.80260437466121));
#24771=CARTESIAN_POINT('Ctrl Pts',(-41.5062464563473,-5.516073939506,9.98137881379674));
#24772=CARTESIAN_POINT('Ctrl Pts',(-41.6766903238786,-5.55734212879185,
10.1555177270924));
#24773=CARTESIAN_POINT('Ctrl Pts',(-41.8511757273807,-5.59910040291801,
10.3247095747707));
#24774=CARTESIAN_POINT('Ctrl Pts',(-41.9016079151999,-5.61116995762843,
10.3736117457738));
#24775=CARTESIAN_POINT('Ctrl Pts',(-41.9523775462543,-5.62328043365766,
10.4221009095724));
#24776=CARTESIAN_POINT('Ctrl Pts',(-42.0034749115207,-5.63542964579464,
10.4701702229062));
#24777=CARTESIAN_POINT('Ctrl Pts',(-43.4867804707271,-9.73793223897115,
0.));
#24778=CARTESIAN_POINT('Ctrl Pts',(-43.4562844339543,-9.95003683365991,
1.72780310113343));
#24779=CARTESIAN_POINT('Ctrl Pts',(-44.1678235515683,-10.2688299769307,
3.28449990511991));
#24780=CARTESIAN_POINT('Ctrl Pts',(-44.8793626691824,-10.5876231202016,
4.84119670910639));
#24781=CARTESIAN_POINT('Ctrl Pts',(-46.1859677783932,-10.9919738365586,
5.91846432228298));
#24782=CARTESIAN_POINT('Ctrl Pts',(-47.492572887604,-11.3963245529156,6.99573193545957));
#24783=CARTESIAN_POINT('Ctrl Pts',(-49.1294147079799,-11.8481561402184,
7.3802042952164));
#24784=CARTESIAN_POINT('Ctrl Pts',(-50.7662565283558,-12.2999877275213,
7.76467665497322));
#24785=CARTESIAN_POINT('Ctrl Pts',(-52.4030983487318,-12.7518193148241,
7.38020429521639));
#24786=CARTESIAN_POINT('Ctrl Pts',(-41.6230663715377,-8.27145263712683,
0.));
#24787=CARTESIAN_POINT('Ctrl Pts',(-41.5925703347649,-8.4835572318156,2.19648874705823));
#24788=CARTESIAN_POINT('Ctrl Pts',(-42.5053946713976,-8.83129082048332,
4.17545672685568));
#24789=CARTESIAN_POINT('Ctrl Pts',(-43.4182190080304,-9.17902440915105,
6.15442470665314));
#24790=CARTESIAN_POINT('Ctrl Pts',(-45.0875275490506,-9.63552400615975,
7.52391304034141));
#24791=CARTESIAN_POINT('Ctrl Pts',(-46.7568360900708,-10.0920236031684,
8.89340137402968));
#24792=CARTESIAN_POINT('Ctrl Pts',(-48.8459616921114,-10.6088837810006,
9.38216610144961));
#24793=CARTESIAN_POINT('Ctrl Pts',(-50.9350872941521,-11.1257439588328,
9.87093082886955));
#24794=CARTESIAN_POINT('Ctrl Pts',(-53.0242128961928,-11.642604136665,9.38216610144961));
#24795=CARTESIAN_POINT('Ctrl Pts',(-39.5090640497074,-7.19674949232894,
0.));
#24796=CARTESIAN_POINT('Ctrl Pts',(-39.4785680129345,-7.40885408701771,
2.7089937269807));
#24797=CARTESIAN_POINT('Ctrl Pts',(-40.611496545266,-7.78823388144414,5.14971273833323));
#24798=CARTESIAN_POINT('Ctrl Pts',(-41.7444250775976,-8.16761367587058,
7.59043174968577));
#24799=CARTESIAN_POINT('Ctrl Pts',(-43.8103476746564,-8.68113776523092,
9.27946171175751));
#24800=CARTESIAN_POINT('Ctrl Pts',(-45.8762702717152,-9.19466185459128,
10.9684916738293));
#24801=CARTESIAN_POINT('Ctrl Pts',(-48.4599655121837,-9.78263041129834,
11.5712994880388));
#24802=CARTESIAN_POINT('Ctrl Pts',(-51.0436607526521,-10.3705989680054,
12.1741073022483));
#24803=CARTESIAN_POINT('Ctrl Pts',(-53.6273559931206,-10.9585675247124,
11.5712994880388));
#24804=CARTESIAN_POINT('Ctrl Pts',(-37.2260157227863,-6.55512420987395,
0.));
#24805=CARTESIAN_POINT('Ctrl Pts',(-37.1955196860134,-6.76722880456271,
3.24562220582793));
#24806=CARTESIAN_POINT('Ctrl Pts',(-38.5589126710876,-7.17974438483098,
6.16982677025168));
#24807=CARTESIAN_POINT('Ctrl Pts',(-39.9223056561618,-7.59225996509924,
9.09403133467541));
#24808=CARTESIAN_POINT('Ctrl Pts',(-42.4035108473793,-8.16549267737354,
11.1176436806954));
#24809=CARTESIAN_POINT('Ctrl Pts',(-44.8847160385968,-8.73872538964782,
13.1412560267153));
#24810=CARTESIAN_POINT('Ctrl Pts',(-47.98626020376,-9.40114938129462,13.8634749112255));
#24811=CARTESIAN_POINT('Ctrl Pts',(-51.0878043689232,-10.0635733729414,
14.5856937957357));
#24812=CARTESIAN_POINT('Ctrl Pts',(-54.1893485340864,-10.7259973645882,
13.8634749112255));
#24813=CARTESIAN_POINT('',(-37.2260157227863,-6.55512420987395,0.));
#24814=CARTESIAN_POINT('Ctrl Pts',(-37.2260157227863,-6.55512420987395,
0.));
#24815=CARTESIAN_POINT('Ctrl Pts',(-37.1955196860134,-6.76722880456271,
3.24562220582793));
#24816=CARTESIAN_POINT('Ctrl Pts',(-38.5589126710876,-7.17974438483098,
6.16982677025168));
#24817=CARTESIAN_POINT('Ctrl Pts',(-39.6971249853932,-7.52412807936691,
8.61106394926976));
#24818=CARTESIAN_POINT('Ctrl Pts',(-41.6420486840548,-7.98700482807827,
10.4489096280657));
#24819=CARTESIAN_POINT('Origin',(-32.3559861244012,-23.8837944332597,1.04083408558608E-14));
#24820=CARTESIAN_POINT('Ctrl Pts',(-37.2260157227863,-6.55512420987395,
0.));
#24821=CARTESIAN_POINT('Ctrl Pts',(-37.1955196860134,-6.76722880456271,
3.24562220582793));
#24822=CARTESIAN_POINT('Ctrl Pts',(-38.5589126710876,-7.17974438483098,
6.16982677025168));
#24823=CARTESIAN_POINT('Ctrl Pts',(-39.9223056561618,-7.59225996509924,
9.09403133467541));
#24824=CARTESIAN_POINT('Ctrl Pts',(-42.4035108473793,-8.16549267737352,
11.1176436806954));
#24825=CARTESIAN_POINT('Ctrl Pts',(-44.8847160385968,-8.73872538964782,
13.1412560267153));
#24826=CARTESIAN_POINT('Ctrl Pts',(-47.98626020376,-9.40114938129462,13.8634749112255));
#24827=CARTESIAN_POINT('Ctrl Pts',(-51.0878043689232,-10.0635733729414,
14.5856937957357));
#24828=CARTESIAN_POINT('Ctrl Pts',(-54.1893485340864,-10.7259973645882,
13.8634749112255));
#24829=CARTESIAN_POINT('Ctrl Pts',(-36.7040912252865,-5.75838408981617,
6.24500451351651E-15));
#24830=CARTESIAN_POINT('Ctrl Pts',(-36.6735951885137,-5.97048868450495,
3.38941559469373));
#24831=CARTESIAN_POINT('Ctrl Pts',(-38.0987427505052,-6.39188323248875,
6.44317352589574));
#24832=CARTESIAN_POINT('Ctrl Pts',(-39.5238903124967,-6.81327778047256,
9.49693145709775));
#24833=CARTESIAN_POINT('Ctrl Pts',(-42.1163734062201,-7.40250983972848,
11.6101975146502));
#24834=CARTESIAN_POINT('Ctrl Pts',(-44.7088564999434,-7.99174189898442,
13.7234635722027));
#24835=CARTESIAN_POINT('Ctrl Pts',(-47.949161939876,-8.67411674999011,14.4776794959001));
#24836=CARTESIAN_POINT('Ctrl Pts',(-51.1894673798085,-9.35649160099581,
15.2318954195974));
#24837=CARTESIAN_POINT('Ctrl Pts',(-54.429772819741,-10.0388664520015,14.4776794959001));
#24838=CARTESIAN_POINT('Ctrl Pts',(-36.8396419064669,-4.81560839388869,
0.));
#24839=CARTESIAN_POINT('Ctrl Pts',(-36.8091458696941,-5.02771298857746,
3.38941559469373));
#24840=CARTESIAN_POINT('Ctrl Pts',(-38.2342934316856,-5.44910753656127,
6.44317352589573));
#24841=CARTESIAN_POINT('Ctrl Pts',(-39.6594409936771,-5.87050208454507,
9.49693145709775));
#24842=CARTESIAN_POINT('Ctrl Pts',(-42.2519240874005,-6.459734143801,11.6101975146502));
#24843=CARTESIAN_POINT('Ctrl Pts',(-44.8444071811238,-7.04896620305693,
13.7234635722027));
#24844=CARTESIAN_POINT('Ctrl Pts',(-48.0847126210563,-7.73134105406263,
14.4776794959001));
#24845=CARTESIAN_POINT('Ctrl Pts',(-51.3250180609889,-8.41371590506832,
15.2318954195974));
#24846=CARTESIAN_POINT('Ctrl Pts',(-54.5653235009214,-9.09609075607403,
14.4776794959001));
#24847=CARTESIAN_POINT('Ctrl Pts',(-37.5648924257372,-4.19818497005524,
0.));
#24848=CARTESIAN_POINT('Ctrl Pts',(-37.5343963889643,-4.41028956474401,
3.24562220582793));
#24849=CARTESIAN_POINT('Ctrl Pts',(-38.8977893740386,-4.82280514501228,
6.16982677025168));
#24850=CARTESIAN_POINT('Ctrl Pts',(-40.2611823591128,-5.23532072528053,
9.09403133467541));
#24851=CARTESIAN_POINT('Ctrl Pts',(-42.7423875503303,-5.80855343755483,
11.1176436806954));
#24852=CARTESIAN_POINT('Ctrl Pts',(-45.2235927415478,-6.38178614982912,
13.1412560267153));
#24853=CARTESIAN_POINT('Ctrl Pts',(-48.3251369067109,-7.04421014147591,
13.8634749112255));
#24854=CARTESIAN_POINT('Ctrl Pts',(-51.4266810718741,-7.70663413312271,
14.5856937957357));
#24855=CARTESIAN_POINT('Ctrl Pts',(-54.5282252370373,-8.36905812476951,
13.8634749112255));
#24856=CARTESIAN_POINT('',(-36.9500351333142,-5.31260798924485,-1.06286264220349E-29));
#24857=CARTESIAN_POINT('Origin',(-38.731713020801,-5.56877962163353,0.));
#24858=CARTESIAN_POINT('Origin',(-38.731713020801,-5.56877962163353,0.));
#24859=CARTESIAN_POINT('Ctrl Pts',(-37.7800000000001,1.19058808997921,0.));
#24860=CARTESIAN_POINT('Ctrl Pts',(-37.78,0.976302375693506,3.24562220582793));
#24861=CARTESIAN_POINT('Ctrl Pts',(-39.1882226984277,0.762016661407787,
6.16982677025167));
#24862=CARTESIAN_POINT('Ctrl Pts',(-40.5964453968553,0.547730947122094,
9.09403133467541));
#24863=CARTESIAN_POINT('Ctrl Pts',(-43.1339750175689,0.333445232836368,
11.1176436806954));
#24864=CARTESIAN_POINT('Ctrl Pts',(-45.6715046382825,0.119159518550672,
13.1412560267153));
#24865=CARTESIAN_POINT('Ctrl Pts',(-48.8357523191413,-0.0951261957350281,
13.8634749112255));
#24866=CARTESIAN_POINT('Ctrl Pts',(-52.0000000000001,-0.309411910020729,
14.5856937957357));
#24867=CARTESIAN_POINT('Ctrl Pts',(-55.1642476808589,-0.52369762430643,
13.8634749112255));
#24868=CARTESIAN_POINT('Ctrl Pts',(-40.1311229851416,1.5007708987902,0.));
#24869=CARTESIAN_POINT('Ctrl Pts',(-40.1311229851416,1.2864851845045,2.70899372698069));
#24870=CARTESIAN_POINT('Ctrl Pts',(-41.30651131265,1.07219947021879,5.14971273833323));
#24871=CARTESIAN_POINT('Ctrl Pts',(-42.4818996401584,0.857913755933074,
7.59043174968577));
#24872=CARTESIAN_POINT('Ctrl Pts',(-44.5998762217203,0.643628041647366,
9.27946171175751));
#24873=CARTESIAN_POINT('Ctrl Pts',(-46.7178528032822,0.429342327361657,
10.9684916738292));
#24874=CARTESIAN_POINT('Ctrl Pts',(-49.3589264016411,0.215056613075952,
11.5712994880388));
#24875=CARTESIAN_POINT('Ctrl Pts',(-52.0000000000001,0.000770898790245644,
12.1741073022483));
#24876=CARTESIAN_POINT('Ctrl Pts',(-54.641073598359,-0.213514815495465,
11.5712994880388));
#24877=CARTESIAN_POINT('Ctrl Pts',(-42.3765540157191,2.26368121662741,0.));
#24878=CARTESIAN_POINT('Ctrl Pts',(-42.3765540157191,2.04939550234168,2.19648874705823));
#24879=CARTESIAN_POINT('Ctrl Pts',(-43.3295747662223,1.83510978805599,4.17545672685568));
#24880=CARTESIAN_POINT('Ctrl Pts',(-44.2825955167256,1.62082407377026,6.15442470665314));
#24881=CARTESIAN_POINT('Ctrl Pts',(-45.9998795700625,1.40653835948456,7.5239130403414));
#24882=CARTESIAN_POINT('Ctrl Pts',(-47.7171636233994,1.19225264519886,8.89340137402968));
#24883=CARTESIAN_POINT('Ctrl Pts',(-49.8585818116997,0.977966930913157,
9.3821661014496));
#24884=CARTESIAN_POINT('Ctrl Pts',(-52.0000000000001,0.763681216627436,
9.87093082886954));
#24885=CARTESIAN_POINT('Ctrl Pts',(-54.1414181883004,0.54939550234174,9.3821661014496));
#24886=CARTESIAN_POINT('Ctrl Pts',(-44.43,3.45000000000016,0.));
#24887=CARTESIAN_POINT('Ctrl Pts',(-44.43,3.23571428571445,1.72780310113342));
#24888=CARTESIAN_POINT('Ctrl Pts',(-45.1796656699787,3.02142857142873,3.28449990511991));
#24889=CARTESIAN_POINT('Ctrl Pts',(-45.9293313399574,2.80714285714304,4.84119670910638));
#24890=CARTESIAN_POINT('Ctrl Pts',(-47.2801821999295,2.59285714285731,5.91846432228297));
#24891=CARTESIAN_POINT('Ctrl Pts',(-48.6310330599015,2.37857142857161,6.99573193545956));
#24892=CARTESIAN_POINT('Ctrl Pts',(-50.3155165299508,2.1642857142859,7.38020429521639));
#24893=CARTESIAN_POINT('Ctrl Pts',(-52.0000000000001,1.95000000000019,7.76467665497321));
#24894=CARTESIAN_POINT('Ctrl Pts',(-53.6844834700493,1.73571428571448,7.38020429521638));
#24895=CARTESIAN_POINT('',(-37.7800000000897,1.19058809004707,1.57948074790763E-9));
#24896=CARTESIAN_POINT('Origin',(-35.4256671812559,19.0359549110503,0.));
#24897=CARTESIAN_POINT('Ctrl Pts',(-37.7800000000849,1.19058808978368,3.13103676972182E-9));
#24898=CARTESIAN_POINT('Ctrl Pts',(-37.780000000137,1.17440993603763,0.24503815333525));
#24899=CARTESIAN_POINT('Ctrl Pts',(-37.7863378835296,1.15808907770421,0.490791160521286));
#24900=CARTESIAN_POINT('Ctrl Pts',(-37.7990994961183,1.14165673905446,0.736766500724735));
#24901=CARTESIAN_POINT('Ctrl Pts',(-37.8118192130495,1.12527834684966,0.981934317700371));
#24902=CARTESIAN_POINT('Ctrl Pts',(-37.8309206531574,1.10878923237345,1.22732257376501));
#24903=CARTESIAN_POINT('Ctrl Pts',(-37.8564381709891,1.0922217785574,1.47243294816276));
#24904=CARTESIAN_POINT('Ctrl Pts',(-37.881917258574,1.0756792758883,1.71717417802952));
#24905=CARTESIAN_POINT('Ctrl Pts',(-37.9137931615158,1.05905869845488,1.96163791541521));
#24906=CARTESIAN_POINT('Ctrl Pts',(-37.9520483462578,1.0423933267648,2.2053240877846));
#24907=CARTESIAN_POINT('Ctrl Pts',(-37.9902707213954,1.02574224815047,2.44880126242));
#24908=CARTESIAN_POINT('Ctrl Pts',(-38.0348614248958,1.00904648209016,2.69150175430983));
#24909=CARTESIAN_POINT('Ctrl Pts',(-38.0857510286497,0.992339825183044,
2.9329295186674));
#24910=CARTESIAN_POINT('Ctrl Pts',(-38.1366299861971,0.975636663341864,
3.17430677585535));
#24911=CARTESIAN_POINT('Ctrl Pts',(-38.1938051285551,0.95892264578539,3.41441139318303));
#24912=CARTESIAN_POINT('Ctrl Pts',(-38.2571558430635,0.942231694705537,
3.6527571061461));
#24913=CARTESIAN_POINT('Ctrl Pts',(-38.3205869992972,0.925519549722661,
3.89140546668762));
#24914=CARTESIAN_POINT('Ctrl Pts',(-38.390209284233,0.908830560438021,4.12829002081138));
#24915=CARTESIAN_POINT('Ctrl Pts',(-38.4658518732601,0.89219846555144,4.36293874377782));
#24916=CARTESIAN_POINT('Ctrl Pts',(-38.5415716478926,0.875549399295574,
4.59782690201425));
#24917=CARTESIAN_POINT('Ctrl Pts',(-38.6233238148867,0.858957373419583,
4.83047425894938));
#24918=CARTESIAN_POINT('Ctrl Pts',(-38.7108897721909,0.842455462110944,
5.06042975959413));
#24919=CARTESIAN_POINT('Ctrl Pts',(-38.7987117380295,0.82590530568219,5.29105755998297));
#24920=CARTESIAN_POINT('Ctrl Pts',(-38.8923812869985,0.809445820264863,
5.51897736305691));
#24921=CARTESIAN_POINT('Ctrl Pts',(-38.9916337971362,0.79310915731082,5.74376259354344));
#24922=CARTESIAN_POINT('Ctrl Pts',(-39.0549201489775,0.782692415223513,
5.88709234072628));
#24923=CARTESIAN_POINT('Ctrl Pts',(-39.1204754952205,0.772325583328654,
6.02914825314197));
#24924=CARTESIAN_POINT('Ctrl Pts',(-39.1882226984626,0.762016661412907,
6.16982677023484));
#24925=CARTESIAN_POINT('Ctrl Pts',(-39.2944523060728,0.745851968590391,
6.390414823391));
#24926=CARTESIAN_POINT('Ctrl Pts',(-39.4066922926963,0.729544808781451,
6.60890054011824));
#24927=CARTESIAN_POINT('Ctrl Pts',(-39.524806665964,0.713126327701068,6.82480412008069));
#24928=CARTESIAN_POINT('Ctrl Pts',(-39.6426543894045,0.696744912263256,
7.04022028559321));
#24929=CARTESIAN_POINT('Ctrl Pts',(-39.766349917329,0.68025270462606,7.25306552029667));
#24930=CARTESIAN_POINT('Ctrl Pts',(-39.8957079165132,0.663682105818622,
7.46287566269449));
#24931=CARTESIAN_POINT('Ctrl Pts',(-40.0248578550338,0.647138159323428,
7.6723483444192));
#24932=CARTESIAN_POINT('Ctrl Pts',(-40.1596519133317,0.630516102449693,
7.87879526533074));
#24933=CARTESIAN_POINT('Ctrl Pts',(-40.2998572837228,0.613849224529908,
8.08177334612247));
#24934=CARTESIAN_POINT('Ctrl Pts',(-40.4399281220159,0.597198339079233,
8.28455666214167));
#24935=CARTESIAN_POINT('Ctrl Pts',(-40.5853996821057,0.580502748576888,
8.48387739272915));
#24936=CARTESIAN_POINT('Ctrl Pts',(-40.735994217132,0.5637962485363,8.6793187361116));
#24937=CARTESIAN_POINT('Ctrl Pts',(-40.8865959953569,0.547088944957281,
8.87476947970534));
#24938=CARTESIAN_POINT('Ctrl Pts',(-41.0423209776643,0.53037076138554,9.06634009532848));
#24939=CARTESIAN_POINT('Ctrl Pts',(-41.2028492923288,0.513675645357026,
9.2536445034098));
#24940=CARTESIAN_POINT('Ctrl Pts',(-41.3634364952214,0.496974404889944,
9.44101762226492));
#24941=CARTESIAN_POINT('Ctrl Pts',(-41.5288302394286,0.480296279393814,
9.62412107875029));
#24942=CARTESIAN_POINT('Ctrl Pts',(-41.6986725382757,0.463674941840322,
9.8026043746612));
#24943=CARTESIAN_POINT('Ctrl Pts',(-41.8687918850914,0.44702649144251,9.98137881379691));
#24944=CARTESIAN_POINT('Ctrl Pts',(-42.0433739554953,0.430435044262166,
10.1555177270927));
#24945=CARTESIAN_POINT('Ctrl Pts',(-42.2220261712059,0.413933671136578,
10.3247095747712));
#24946=CARTESIAN_POINT('Ctrl Pts',(-42.2736627087968,0.409164215743528,
10.3736117457741));
#24947=CARTESIAN_POINT('Ctrl Pts',(-42.3256390786481,0.404402278731116,
10.4221009095725));
#24948=CARTESIAN_POINT('Ctrl Pts',(-42.3779453595728,0.399648641330075,
10.4701702229062));
#24949=CARTESIAN_POINT('Ctrl Pts',(-44.4300000000001,-3.44999999999985,
0.));
#24950=CARTESIAN_POINT('Ctrl Pts',(-44.4300000000001,-3.66428571428556,
1.72780310113342));
#24951=CARTESIAN_POINT('Ctrl Pts',(-45.1796656699787,-3.87857142857126,
3.28449990511991));
#24952=CARTESIAN_POINT('Ctrl Pts',(-45.9293313399574,-4.09285714285698,
4.84119670910638));
#24953=CARTESIAN_POINT('Ctrl Pts',(-47.2801821999295,-4.30714285714269,
5.91846432228298));
#24954=CARTESIAN_POINT('Ctrl Pts',(-48.6310330599015,-4.52142857142839,
6.99573193545956));
#24955=CARTESIAN_POINT('Ctrl Pts',(-50.3155165299508,-4.73571428571411,
7.38020429521639));
#24956=CARTESIAN_POINT('Ctrl Pts',(-52.0000000000001,-4.94999999999981,
7.76467665497322));
#24957=CARTESIAN_POINT('Ctrl Pts',(-53.6844834700494,-5.16428571428552,
7.38020429521639));
#24958=CARTESIAN_POINT('Ctrl Pts',(-42.3765540157191,-2.2636812166271,0.));
#24959=CARTESIAN_POINT('Ctrl Pts',(-42.3765540157191,-2.47796693091281,
2.19648874705822));
#24960=CARTESIAN_POINT('Ctrl Pts',(-43.3295747662224,-2.69225264519852,
4.17545672685568));
#24961=CARTESIAN_POINT('Ctrl Pts',(-44.2825955167256,-2.90653835948424,
6.15442470665314));
#24962=CARTESIAN_POINT('Ctrl Pts',(-45.9998795700625,-3.12082407376995,
7.52391304034139));
#24963=CARTESIAN_POINT('Ctrl Pts',(-47.7171636233994,-3.33510978805565,
8.89340137402966));
#24964=CARTESIAN_POINT('Ctrl Pts',(-49.8585818116998,-3.54939550234135,
9.38216610144959));
#24965=CARTESIAN_POINT('Ctrl Pts',(-52.0000000000001,-3.76368121662706,
9.87093082886952));
#24966=CARTESIAN_POINT('Ctrl Pts',(-54.1414181883004,-3.97796693091276,
9.38216610144959));
#24967=CARTESIAN_POINT('Ctrl Pts',(-40.1311229851416,-1.50077089878991,
0.));
#24968=CARTESIAN_POINT('Ctrl Pts',(-40.1311229851416,-1.71505661307563,
2.7089937269807));
#24969=CARTESIAN_POINT('Ctrl Pts',(-41.30651131265,-1.92934232736134,5.14971273833323));
#24970=CARTESIAN_POINT('Ctrl Pts',(-42.4818996401584,-2.14362804164706,
7.59043174968577));
#24971=CARTESIAN_POINT('Ctrl Pts',(-44.5998762217203,-2.35791375593276,
9.27946171175751));
#24972=CARTESIAN_POINT('Ctrl Pts',(-46.7178528032822,-2.57219947021846,
10.9684916738293));
#24973=CARTESIAN_POINT('Ctrl Pts',(-49.3589264016412,-2.78648518450417,
11.5712994880388));
#24974=CARTESIAN_POINT('Ctrl Pts',(-52.0000000000001,-3.00077089878988,
12.1741073022483));
#24975=CARTESIAN_POINT('Ctrl Pts',(-54.641073598359,-3.21505661307558,11.5712994880388));
#24976=CARTESIAN_POINT('Ctrl Pts',(-37.7800000000001,-1.19058808997893,
0.));
#24977=CARTESIAN_POINT('Ctrl Pts',(-37.7800000000001,-1.40487380426465,
3.24562220582792));
#24978=CARTESIAN_POINT('Ctrl Pts',(-39.1882226984277,-1.61915951855035,
6.16982677025167));
#24979=CARTESIAN_POINT('Ctrl Pts',(-40.5964453968553,-1.83344523283606,
9.09403133467541));
#24980=CARTESIAN_POINT('Ctrl Pts',(-43.1339750175689,-2.04773094712177,
11.1176436806954));
#24981=CARTESIAN_POINT('Ctrl Pts',(-45.6715046382825,-2.26201666140747,
13.1412560267153));
#24982=CARTESIAN_POINT('Ctrl Pts',(-48.8357523191413,-2.47630237569317,
13.8634749112255));
#24983=CARTESIAN_POINT('Ctrl Pts',(-52.0000000000001,-2.69058808997887,
14.5856937957357));
#24984=CARTESIAN_POINT('Ctrl Pts',(-55.1642476808589,-2.90487380426458,
13.8634749112255));
#24985=CARTESIAN_POINT('',(-37.7800000000001,-1.19058808997893,0.));
#24986=CARTESIAN_POINT('Ctrl Pts',(-37.7800000000001,-1.19058808997893,
0.));
#24987=CARTESIAN_POINT('Ctrl Pts',(-37.7800000000001,-1.40487380426465,
3.24562220582792));
#24988=CARTESIAN_POINT('Ctrl Pts',(-39.1882226984277,-1.61915951855035,
6.16982677025167));
#24989=CARTESIAN_POINT('Ctrl Pts',(-40.3638605623321,-1.79805338220513,
8.61106394926977));
#24990=CARTESIAN_POINT('Ctrl Pts',(-42.3548619717231,-1.97942721139887,
10.4489096280657));
#24991=CARTESIAN_POINT('Origin',(-35.425667181256,-19.03595491105,0.));
#24992=CARTESIAN_POINT('Ctrl Pts',(-37.7800000000001,-1.19058808997893,
0.));
#24993=CARTESIAN_POINT('Ctrl Pts',(-37.7800000000001,-1.40487380426465,
3.24562220582792));
#24994=CARTESIAN_POINT('Ctrl Pts',(-39.1882226984277,-1.61915951855037,
6.16982677025167));
#24995=CARTESIAN_POINT('Ctrl Pts',(-40.5964453968553,-1.83344523283606,
9.09403133467541));
#24996=CARTESIAN_POINT('Ctrl Pts',(-43.1339750175689,-2.04773094712178,
11.1176436806954));
#24997=CARTESIAN_POINT('Ctrl Pts',(-45.6715046382825,-2.26201666140747,
13.1412560267153));
#24998=CARTESIAN_POINT('Ctrl Pts',(-48.8357523191413,-2.47630237569318,
13.8634749112255));
#24999=CARTESIAN_POINT('Ctrl Pts',(-52.0000000000001,-2.69058808997887,
14.5856937957357));
#25000=CARTESIAN_POINT('Ctrl Pts',(-55.1642476808589,-2.90487380426458,
13.8634749112255));
#25001=CARTESIAN_POINT('Ctrl Pts',(-37.1500000000001,-0.476235235991505,
0.));
#25002=CARTESIAN_POINT('Ctrl Pts',(-37.15,-0.690520950277214,3.38941559469372));
#25003=CARTESIAN_POINT('Ctrl Pts',(-38.6206123116491,-0.904806664562923,
6.44317352589573));
#25004=CARTESIAN_POINT('Ctrl Pts',(-40.0912246232982,-1.11909237884862,
9.49693145709775));
#25005=CARTESIAN_POINT('Ctrl Pts',(-42.7411764423979,-1.33337809313434,
11.6101975146502));
#25006=CARTESIAN_POINT('Ctrl Pts',(-45.3911282614975,-1.54766380742003,
13.7234635722027));
#25007=CARTESIAN_POINT('Ctrl Pts',(-48.6955641307488,-1.76194952170574,
14.4776794959001));
#25008=CARTESIAN_POINT('Ctrl Pts',(-52.0000000000001,-1.97623523599144,
15.2318954195974));
#25009=CARTESIAN_POINT('Ctrl Pts',(-55.3044358692513,-2.19052095027714,
14.4776794959001));
#25010=CARTESIAN_POINT('Ctrl Pts',(-37.1500000000001,0.476235235991757,
0.));
#25011=CARTESIAN_POINT('Ctrl Pts',(-37.15,0.261949521706039,3.38941559469373));
#25012=CARTESIAN_POINT('Ctrl Pts',(-38.6206123116491,0.0476638074203333,
6.44317352589573));
#25013=CARTESIAN_POINT('Ctrl Pts',(-40.0912246232982,-0.166621906865366,
9.49693145709774));
#25014=CARTESIAN_POINT('Ctrl Pts',(-42.7411764423979,-0.380907621151074,
11.6101975146502));
#25015=CARTESIAN_POINT('Ctrl Pts',(-45.3911282614975,-0.595193335436777,
13.7234635722027));
#25016=CARTESIAN_POINT('Ctrl Pts',(-48.6955641307488,-0.809479049722483,
14.4776794959001));
#25017=CARTESIAN_POINT('Ctrl Pts',(-52.0000000000001,-1.02376476400818,
15.2318954195974));
#25018=CARTESIAN_POINT('Ctrl Pts',(-55.3044358692513,-1.23805047829389,
14.4776794959001));
#25019=CARTESIAN_POINT('Ctrl Pts',(-37.7800000000001,1.1905880899792,0.));
#25020=CARTESIAN_POINT('Ctrl Pts',(-37.78,0.976302375693499,3.24562220582793));
#25021=CARTESIAN_POINT('Ctrl Pts',(-39.1882226984276,0.762016661407785,
6.16982677025167));
#25022=CARTESIAN_POINT('Ctrl Pts',(-40.5964453968553,0.547730947122086,
9.09403133467541));
#25023=CARTESIAN_POINT('Ctrl Pts',(-43.1339750175689,0.333445232836365,
11.1176436806954));
#25024=CARTESIAN_POINT('Ctrl Pts',(-45.6715046382825,0.119159518550669,
13.1412560267153));
#25025=CARTESIAN_POINT('Ctrl Pts',(-48.8357523191413,-0.0951261957350281,
13.8634749112255));
#25026=CARTESIAN_POINT('Ctrl Pts',(-52.0000000000001,-0.309411910020738,
14.5856937957357));
#25027=CARTESIAN_POINT('Ctrl Pts',(-55.1642476808589,-0.52369762430644,
13.8634749112255));
#25028=CARTESIAN_POINT('',(-37.3300000000069,4.97394955414463E-6,-1.27795074269892E-29));
#25029=CARTESIAN_POINT('Origin',(-39.1300000000001,1.37043154602168E-13,
0.));
#25030=CARTESIAN_POINT('Origin',(-39.1300000000001,1.37043154602168E-13,
0.));
#25031=CARTESIAN_POINT('Ctrl Pts',(-37.2260157227862,6.5551242098742,0.));
#25032=CARTESIAN_POINT('Ctrl Pts',(-37.256511759559,6.34301961518543,3.24562220582793));
#25033=CARTESIAN_POINT('Ctrl Pts',(-38.680896818179,6.33132600607616,6.16982677025168));
#25034=CARTESIAN_POINT('Ctrl Pts',(-40.1052818767989,6.31963239696691,9.09403133467542));
#25035=CARTESIAN_POINT('Ctrl Pts',(-42.647479141562,6.46865591986365,11.1176436806954));
#25036=CARTESIAN_POINT('Ctrl Pts',(-45.1896764063252,6.61767944276043,13.1412560267153));
#25037=CARTESIAN_POINT('Ctrl Pts',(-48.3522126450341,6.85589424502971,13.8634749112255));
#25038=CARTESIAN_POINT('Ctrl Pts',(-51.514748883743,7.09410904729899,14.5856937957357));
#25039=CARTESIAN_POINT('Ctrl Pts',(-54.6772851224519,7.33232384956826,13.8634749112255));
#25040=CARTESIAN_POINT('Ctrl Pts',(-39.5090640497073,7.19674949232921,0.));
#25041=CARTESIAN_POINT('Ctrl Pts',(-39.5395600864801,6.98464489764044,2.70899372698069));
#25042=CARTESIAN_POINT('Ctrl Pts',(-40.7334806923574,6.93981550268934,5.14971273833323));
#25043=CARTESIAN_POINT('Ctrl Pts',(-41.9274012982346,6.89498610773823,7.59043174968578));
#25044=CARTESIAN_POINT('Ctrl Pts',(-44.0543159688391,6.98430100772104,9.27946171175752));
#25045=CARTESIAN_POINT('Ctrl Pts',(-46.1812306394436,7.07361590770388,10.9684916738293));
#25046=CARTESIAN_POINT('Ctrl Pts',(-48.8259179534578,7.2373752750334,11.5712994880388));
#25047=CARTESIAN_POINT('Ctrl Pts',(-51.4706052674719,7.40113464236295,12.1741073022483));
#25048=CARTESIAN_POINT('Ctrl Pts',(-54.1152925814861,7.56489400969249,11.5712994880388));
#25049=CARTESIAN_POINT('Ctrl Pts',(-41.6230663715377,8.27145263712713,-1.05434036998093E-14));
#25050=CARTESIAN_POINT('Ctrl Pts',(-41.6535624083105,8.05934804243833,2.19648874705823));
#25051=CARTESIAN_POINT('Ctrl Pts',(-42.6273788184889,7.98287244172854,4.17545672685567));
#25052=CARTESIAN_POINT('Ctrl Pts',(-43.6011952286674,7.90639684101872,6.15442470665313));
#25053=CARTESIAN_POINT('Ctrl Pts',(-45.3314958432333,7.93868724864988,7.5239130403414));
#25054=CARTESIAN_POINT('Ctrl Pts',(-47.0617964577992,7.97097765628105,8.89340137402968));
#25055=CARTESIAN_POINT('Ctrl Pts',(-49.2119141333855,8.06362864473573,9.3821661014496));
#25056=CARTESIAN_POINT('Ctrl Pts',(-51.3620318089719,8.1562796331904,9.87093082886953));
#25057=CARTESIAN_POINT('Ctrl Pts',(-53.5121494845583,8.24893062164507,9.3821661014496));
#25058=CARTESIAN_POINT('Ctrl Pts',(-43.486780470727,9.73793223897145,0.));
#25059=CARTESIAN_POINT('Ctrl Pts',(-43.5172765074999,9.52582764428269,1.72780310113343));
#25060=CARTESIAN_POINT('Ctrl Pts',(-44.2898076986597,9.42041159817596,3.28449990511991));
#25061=CARTESIAN_POINT('Ctrl Pts',(-45.0623388898194,9.31499555206925,4.84119670910638));
#25062=CARTESIAN_POINT('Ctrl Pts',(-46.4299360725759,9.29513707904871,5.91846432228298));
#25063=CARTESIAN_POINT('Ctrl Pts',(-47.7975332553324,9.27527860602821,6.99573193545956));
#25064=CARTESIAN_POINT('Ctrl Pts',(-49.495367149254,9.30290100395352,7.38020429521639));
#25065=CARTESIAN_POINT('Ctrl Pts',(-51.1932010431756,9.33052340187885,7.76467665497322));
#25066=CARTESIAN_POINT('Ctrl Pts',(-52.8910349370973,9.35814579980418,7.38020429521639));
#25067=CARTESIAN_POINT('',(-37.2260157226851,6.55512420967627,-1.21941363803477E-9));
#25068=CARTESIAN_POINT('Origin',(-32.3559861244011,23.8837944332599,1.04083408558608E-14));
#25069=CARTESIAN_POINT('Ctrl Pts',(-37.2260157227862,6.5551242098742,0.));
#25070=CARTESIAN_POINT('Ctrl Pts',(-37.256511759559,6.34301961518543,3.24562220582793));
#25071=CARTESIAN_POINT('Ctrl Pts',(-38.680896818179,6.33132600607616,6.16982677025168));
#25072=CARTESIAN_POINT('Ctrl Pts',(-39.8771654641449,6.32150513786997,8.6257176219852));
#25073=CARTESIAN_POINT('Ctrl Pts',(-41.8897230480067,6.4265912346088,10.4701702229062));
#25074=CARTESIAN_POINT('Ctrl Pts',(-44.4687528548127,2.90816428999302,0.));
#25075=CARTESIAN_POINT('Ctrl Pts',(-44.4992488915856,2.69605969530425,1.72780310113343));
#25076=CARTESIAN_POINT('Ctrl Pts',(-45.2717800827454,2.59064364919753,3.28449990511991));
#25077=CARTESIAN_POINT('Ctrl Pts',(-46.0443112739052,2.48522760309082,4.84119670910639));
#25078=CARTESIAN_POINT('Ctrl Pts',(-47.4119084566616,2.46536913007028,5.91846432228298));
#25079=CARTESIAN_POINT('Ctrl Pts',(-48.7795056394181,2.44551065704976,6.99573193545956));
#25080=CARTESIAN_POINT('Ctrl Pts',(-50.4773395333397,2.47313305497509,7.38020429521639));
#25081=CARTESIAN_POINT('Ctrl Pts',(-52.1751734272613,2.50075545290041,7.76467665497322));
#25082=CARTESIAN_POINT('Ctrl Pts',(-53.873007321183,2.52837785082574,7.38020429521639));
#25083=CARTESIAN_POINT('Ctrl Pts',(-42.2673772240309,3.79017222552557,0.));
#25084=CARTESIAN_POINT('Ctrl Pts',(-42.2978732608037,3.57806763083681,2.19648874705823));
#25085=CARTESIAN_POINT('Ctrl Pts',(-43.2716896709821,3.501592030127,4.17545672685568));
#25086=CARTESIAN_POINT('Ctrl Pts',(-44.2455060811606,3.42511642941718,6.15442470665314));
#25087=CARTESIAN_POINT('Ctrl Pts',(-45.9758066957265,3.45740683704835,7.52391304034141));
#25088=CARTESIAN_POINT('Ctrl Pts',(-47.7061073102924,3.48969724467951,8.89340137402968));
#25089=CARTESIAN_POINT('Ctrl Pts',(-49.8562249858787,3.5823482331342,9.38216610144962));
#25090=CARTESIAN_POINT('Ctrl Pts',(-52.0063426614651,3.67499922158886,9.87093082886955));
#25091=CARTESIAN_POINT('Ctrl Pts',(-54.1564603370514,3.76765021004354,9.38216610144961));
#25092=CARTESIAN_POINT('Ctrl Pts',(-39.9362279852004,4.22575906238256,0.));
#25093=CARTESIAN_POINT('Ctrl Pts',(-39.9667240219733,4.0136544676938,2.70899372698069));
#25094=CARTESIAN_POINT('Ctrl Pts',(-41.1606446278505,3.9688250727427,5.14971273833323));
#25095=CARTESIAN_POINT('Ctrl Pts',(-42.3545652337277,3.92399567779159,7.59043174968578));
#25096=CARTESIAN_POINT('Ctrl Pts',(-44.4814799043322,4.01331057777441,9.27946171175751));
#25097=CARTESIAN_POINT('Ctrl Pts',(-46.6083945749367,4.10262547775725,10.9684916738293));
#25098=CARTESIAN_POINT('Ctrl Pts',(-49.2530818889509,4.26638484508678,11.5712994880388));
#25099=CARTESIAN_POINT('Ctrl Pts',(-51.8977692029651,4.43014421241632,12.1741073022483));
#25100=CARTESIAN_POINT('Ctrl Pts',(-54.5424565169792,4.59390357974585,11.5712994880388));
#25101=CARTESIAN_POINT('Ctrl Pts',(-37.5648924257371,4.19818497005551,0.));
#25102=CARTESIAN_POINT('Ctrl Pts',(-37.59538846251,3.98608037536675,3.24562220582792));
#25103=CARTESIAN_POINT('Ctrl Pts',(-39.0197735211299,3.97438676625746,6.16982677025168));
#25104=CARTESIAN_POINT('Ctrl Pts',(-40.4441585797498,3.96269315714822,9.09403133467541));
#25105=CARTESIAN_POINT('Ctrl Pts',(-42.986355844513,4.11171668004496,11.1176436806954));
#25106=CARTESIAN_POINT('Ctrl Pts',(-45.5285531092762,4.26074020294174,13.1412560267153));
#25107=CARTESIAN_POINT('Ctrl Pts',(-48.691089347985,4.49895500521102,13.8634749112255));
#25108=CARTESIAN_POINT('Ctrl Pts',(-51.8536255866939,4.73716980748029,14.5856937957357));
#25109=CARTESIAN_POINT('Ctrl Pts',(-55.0161618254028,4.97538460974957,13.8634749112255));
#25110=CARTESIAN_POINT('',(-37.5648924257371,4.19818497005551,0.));
#25111=CARTESIAN_POINT('Ctrl Pts',(-37.5648924257371,4.19818497005551,0.));
#25112=CARTESIAN_POINT('Ctrl Pts',(-37.59538846251,3.98608037536675,3.24562220582792));
#25113=CARTESIAN_POINT('Ctrl Pts',(-39.0197735211299,3.97438676625746,6.16982677025168));
#25114=CARTESIAN_POINT('Ctrl Pts',(-40.2089043379837,3.96462449666056,8.61106394926976));
#25115=CARTESIAN_POINT('Ctrl Pts',(-42.2054524109828,4.06844583510791,10.4489096280657));
#25116=CARTESIAN_POINT('Origin',(-37.7741838134885,-13.8005982420123,1.04083408558608E-14));
#25117=CARTESIAN_POINT('Ctrl Pts',(-37.5648924257371,4.19818497005551,0.));
#25118=CARTESIAN_POINT('Ctrl Pts',(-37.59538846251,3.98608037536675,3.24562220582792));
#25119=CARTESIAN_POINT('Ctrl Pts',(-39.0197735211299,3.97438676625746,6.16982677025168));
#25120=CARTESIAN_POINT('Ctrl Pts',(-40.4441585797498,3.96269315714822,9.09403133467541));
#25121=CARTESIAN_POINT('Ctrl Pts',(-42.986355844513,4.11171668004496,11.1176436806954));
#25122=CARTESIAN_POINT('Ctrl Pts',(-45.5285531092762,4.26074020294174,13.1412560267153));
#25123=CARTESIAN_POINT('Ctrl Pts',(-48.691089347985,4.49895500521102,13.8634749112255));
#25124=CARTESIAN_POINT('Ctrl Pts',(-51.8536255866939,4.73716980748029,14.5856937957357));
#25125=CARTESIAN_POINT('Ctrl Pts',(-55.0161618254028,4.97538460974957,13.8634749112255));
#25126=CARTESIAN_POINT('Ctrl Pts',(-36.8396419064669,4.81560839388895,0.));
#25127=CARTESIAN_POINT('Ctrl Pts',(-36.8701379432397,4.60350379920018,3.38941559469373));
#25128=CARTESIAN_POINT('Ctrl Pts',(-38.3562775787769,4.60068915780645,6.44317352589574));
#25129=CARTESIAN_POINT('Ctrl Pts',(-39.8424172143141,4.59787451641272,9.49693145709774));
#25130=CARTESIAN_POINT('Ctrl Pts',(-42.4958923815832,4.76289738629114,11.6101975146502));
#25131=CARTESIAN_POINT('Ctrl Pts',(-45.1493675488523,4.92792025616953,13.7234635722027));
#25132=CARTESIAN_POINT('Ctrl Pts',(-48.4506650623305,5.18608591779772,14.4776794959001));
#25133=CARTESIAN_POINT('Ctrl Pts',(-51.7519625758087,5.44425157942588,15.2318954195974));
#25134=CARTESIAN_POINT('Ctrl Pts',(-55.0532600892869,5.70241724105408,14.4776794959001));
#25135=CARTESIAN_POINT('Ctrl Pts',(-36.7040912252865,5.75838408981643,6.24500451351651E-15));
#25136=CARTESIAN_POINT('Ctrl Pts',(-36.7345872620593,5.54627949512765,3.38941559469373));
#25137=CARTESIAN_POINT('Ctrl Pts',(-38.2207268975965,5.54346485373394,6.44317352589574));
#25138=CARTESIAN_POINT('Ctrl Pts',(-39.7068665331337,5.54065021234019,9.49693145709775));
#25139=CARTESIAN_POINT('Ctrl Pts',(-42.3603417004028,5.70567308221862,11.6101975146502));
#25140=CARTESIAN_POINT('Ctrl Pts',(-45.0138168676718,5.87069595209702,13.7234635722027));
#25141=CARTESIAN_POINT('Ctrl Pts',(-48.3151143811501,6.12886161372521,14.4776794959001));
#25142=CARTESIAN_POINT('Ctrl Pts',(-51.6164118946283,6.38702727535337,15.2318954195974));
#25143=CARTESIAN_POINT('Ctrl Pts',(-54.9177094081065,6.64519293698155,14.4776794959001));
#25144=CARTESIAN_POINT('Ctrl Pts',(-37.2260157227862,6.5551242098742,0.));
#25145=CARTESIAN_POINT('Ctrl Pts',(-37.2565117595591,6.34301961518544,3.24562220582793));
#25146=CARTESIAN_POINT('Ctrl Pts',(-38.680896818179,6.33132600607617,6.16982677025167));
#25147=CARTESIAN_POINT('Ctrl Pts',(-40.1052818767989,6.31963239696691,9.09403133467541));
#25148=CARTESIAN_POINT('Ctrl Pts',(-42.647479141562,6.46865591986366,11.1176436806954));
#25149=CARTESIAN_POINT('Ctrl Pts',(-45.1896764063252,6.61767944276043,13.1412560267153));
#25150=CARTESIAN_POINT('Ctrl Pts',(-48.3522126450341,6.85589424502971,13.8634749112255));
#25151=CARTESIAN_POINT('Ctrl Pts',(-51.514748883743,7.09410904729899,14.5856937957357));
#25152=CARTESIAN_POINT('Ctrl Pts',(-54.6772851224519,7.33232384956826,13.8634749112255));
#25153=CARTESIAN_POINT('',(-36.9500337175364,5.31261783619598,-1.46702345113165E-29));
#25154=CARTESIAN_POINT('Origin',(-38.7317130208009,5.56877962163379,0.));
#25155=CARTESIAN_POINT('Origin',(-38.7317130208009,5.56877962163379,0.));
#25156=CARTESIAN_POINT('Ctrl Pts',(-35.914217116421,11.7862169042734,0.));
#25157=CARTESIAN_POINT('Ctrl Pts',(-35.9745883786013,11.5806112670703,3.24562220582793));
#25158=CARTESIAN_POINT('Ctrl Pts',(-37.3861394252073,11.7717478112973,6.16982677025167));
#25159=CARTESIAN_POINT('Ctrl Pts',(-38.7976904718133,11.9628843555244,9.09403133467541));
#25160=CARTESIAN_POINT('Ctrl Pts',(-41.292803575407,12.4721834264258,11.1176436806954));
#25161=CARTESIAN_POINT('Ctrl Pts',(-43.7879166790007,12.9814824973272,13.1412560267153));
#25162=CARTESIAN_POINT('Ctrl Pts',(-46.884361357741,13.667348449732,13.8634749112255));
#25163=CARTESIAN_POINT('Ctrl Pts',(-49.9808060364813,14.3532144021369,14.5856937957357));
#25164=CARTESIAN_POINT('Ctrl Pts',(-53.0772507152215,15.0390803545417,13.8634749112255));
#25165=CARTESIAN_POINT('Ctrl Pts',(-38.0827145049532,12.7462230199162,0.));
#25166=CARTESIAN_POINT('Ctrl Pts',(-38.1430857671335,12.540617382713,2.7089937269807));
#25167=CARTESIAN_POINT('Ctrl Pts',(-39.3312338708267,12.6661569043005,5.14971273833323));
#25168=CARTESIAN_POINT('Ctrl Pts',(-40.5193819745197,12.7916964258879,7.59043174968578));
#25169=CARTESIAN_POINT('Ctrl Pts',(-42.6119368849888,13.1827937463385,9.27946171175751));
#25170=CARTESIAN_POINT('Ctrl Pts',(-44.7044917954577,13.5738910667891,10.9684916738293));
#25171=CARTESIAN_POINT('Ctrl Pts',(-47.2989546180622,14.1123618472581,11.5712994880388));
#25172=CARTESIAN_POINT('Ctrl Pts',(-49.8934174406667,14.650832627727,12.1741073022483));
#25173=CARTESIAN_POINT('Ctrl Pts',(-52.4878802632712,15.189303408196,11.5712994880388));
#25174=CARTESIAN_POINT('Ctrl Pts',(-40.0222531270433,14.1108411348346,0.));
#25175=CARTESIAN_POINT('Ctrl Pts',(-40.0826243892236,13.9052354976315,2.19648874705823));
#25176=CARTESIAN_POINT('Ctrl Pts',(-41.0574123652206,13.9681268331906,4.17545672685568));
#25177=CARTESIAN_POINT('Ctrl Pts',(-42.0322003412176,14.0310181687497,6.15442470665314));
#25178=CARTESIAN_POINT('Ctrl Pts',(-43.7402935862749,14.3092273587163,7.5239130403414));
#25179=CARTESIAN_POINT('Ctrl Pts',(-45.4483868313321,14.5874365486828,8.89340137402967));
#25180=CARTESIAN_POINT('Ctrl Pts',(-47.5634337987569,14.9851381329363,9.3821661014496));
#25181=CARTESIAN_POINT('Ctrl Pts',(-49.6784807661817,15.3828397171898,9.87093082886953));
#25182=CARTESIAN_POINT('Ctrl Pts',(-51.7935277336065,15.7805413014433,9.3821661014496));
#25183=CARTESIAN_POINT('Ctrl Pts',(-41.6582954965892,15.8276282594349,0.));
#25184=CARTESIAN_POINT('Ctrl Pts',(-41.7186667587695,15.6220226222318,1.72780310113342));
#25185=CARTESIAN_POINT('Ctrl Pts',(-42.4983369638544,15.6276222110081,3.28449990511991));
#25186=CARTESIAN_POINT('Ctrl Pts',(-43.2780071689392,15.6332217997843,4.84119670910639));
#25187=CARTESIAN_POINT('Ctrl Pts',(-44.6345103396638,15.8081948292726,5.91846432228298));
#25188=CARTESIAN_POINT('Ctrl Pts',(-45.9910135103883,15.9831678587608,6.99573193545956));
#25189=CARTESIAN_POINT('Ctrl Pts',(-47.6676348262507,16.2521360565318,7.38020429521639));
#25190=CARTESIAN_POINT('Ctrl Pts',(-49.3442561421131,16.5211042543028,7.76467665497322));
#25191=CARTESIAN_POINT('Ctrl Pts',(-51.0208774579755,16.7900724520738,7.38020429521639));
#25192=CARTESIAN_POINT('',(-35.9142171164436,11.7862169042832,1.57948959448622E-9));
#25193=CARTESIAN_POINT('Origin',(-28.6276304970124,28.2454287759839,0.));
#25194=CARTESIAN_POINT('Ctrl Pts',(-35.9142171165574,11.7862169041097,3.13105427371818E-9));
#25195=CARTESIAN_POINT('Ctrl Pts',(-35.9187750292273,11.770694079279,0.245038153335573));
#25196=CARTESIAN_POINT('Ctrl Pts',(-35.9294543009582,11.7568199184778,0.490791160521916));
#25197=CARTESIAN_POINT('Ctrl Pts',(-35.9463285033518,11.7446485667474,0.736766500725672));
#25198=CARTESIAN_POINT('Ctrl Pts',(-35.9631473086865,11.7325171728811,0.981934317701321));
#25199=CARTESIAN_POINT('Ctrl Pts',(-35.9861205266374,11.722077480961,1.22732257376597));
#25200=CARTESIAN_POINT('Ctrl Pts',(-36.0152719968249,11.7133702409768,1.47243294816374));
#25201=CARTESIAN_POINT('Ctrl Pts',(-36.0443795639103,11.7046761143911,1.7171741780305));
#25202=CARTESIAN_POINT('Ctrl Pts',(-36.0796468265871,11.6977092667637,1.96163791541619));
#25203=CARTESIAN_POINT('Ctrl Pts',(-36.1210475853283,11.6924966907342,2.20532408778557));
#25204=CARTESIAN_POINT('Ctrl Pts',(-36.1624128366599,11.6872885852767,2.44880126242097));
#25205=CARTESIAN_POINT('Ctrl Pts',(-36.2099010442177,11.6838317679613,2.69150175431078));
#25206=CARTESIAN_POINT('Ctrl Pts',(-36.2634360706164,11.6821391062286,2.93292951866834));
#25207=CARTESIAN_POINT('Ctrl Pts',(-36.3169598973807,11.6804467986041,3.17430677585616));
#25208=CARTESIAN_POINT('Ctrl Pts',(-36.3765279276399,11.6805179152421,3.41441139318369));
#25209=CARTESIAN_POINT('Ctrl Pts',(-36.442014877408,11.6823510237342,3.65275710614662));
#25210=CARTESIAN_POINT('Ctrl Pts',(-36.5075849814587,11.6841864598782,3.89140546668812));
#25211=CARTESIAN_POINT('Ctrl Pts',(-36.5790889062839,11.687788356271,4.12829002081188));
#25212=CARTESIAN_POINT('Ctrl Pts',(-36.6563532415795,11.6931409581035,4.36293874377831));
#25213=CARTESIAN_POINT('Ctrl Pts',(-36.7336964173083,11.6984990217245,4.59782690201468));
#25214=CARTESIAN_POINT('Ctrl Pts',(-36.8168115609901,11.705611336513,4.83047425894976));
#25215=CARTESIAN_POINT('Ctrl Pts',(-36.9054796074171,11.7144480496047,5.06042975959445));
#25216=CARTESIAN_POINT('Ctrl Pts',(-36.994406884455,11.7233105977817,5.29105755998327));
#25217=CARTESIAN_POINT('Ctrl Pts',(-37.0889193314433,11.7339075987037,5.51897736305718));
#25218=CARTESIAN_POINT('Ctrl Pts',(-37.1887539873583,11.746195348841,5.74376259354369));
#25219=CARTESIAN_POINT('Ctrl Pts',(-37.2524115326579,11.7540303837176,5.88709234072645));
#25220=CARTESIAN_POINT('Ctrl Pts',(-37.318232100817,11.7625525566675,6.02914825314205));
#25221=CARTESIAN_POINT('Ctrl Pts',(-37.3861394252394,11.7717478113121,6.16982677023484));
#25222=CARTESIAN_POINT('Ctrl Pts',(-37.4926201075706,11.7861662410925,6.39041482339092));
#25223=CARTESIAN_POINT('Ctrl Pts',(-37.6049078439222,11.8021412942475,6.60890054011809));
#25224=CARTESIAN_POINT('Ctrl Pts',(-37.7228633758096,11.8196645413939,6.82480412008048));
#25225=CARTESIAN_POINT('Ctrl Pts',(-37.8405526164633,11.8371482288263,7.04022028559302));
#25226=CARTESIAN_POINT('Ctrl Pts',(-37.9638839981999,11.856173128831,7.2530655202965));
#25227=CARTESIAN_POINT('Ctrl Pts',(-38.0926705666684,11.8767181155648,7.46287566269434));
#25228=CARTESIAN_POINT('Ctrl Pts',(-38.221249993568,11.8972300575421,7.67234834441899));
#25229=CARTESIAN_POINT('Ctrl Pts',(-38.3552669199728,11.919257185456,7.87879526533047));
#25230=CARTESIAN_POINT('Ctrl Pts',(-38.4944885898569,11.9427658506831,8.08177334612215));
#25231=CARTESIAN_POINT('Ctrl Pts',(-38.6335766715388,11.9662519584999,8.28455666214102));
#25232=CARTESIAN_POINT('Ctrl Pts',(-38.7778593027057,11.9912167312943,8.48387739272819));
#25233=CARTESIAN_POINT('Ctrl Pts',(-38.9270604659003,12.0176143452909,8.67931873611034));
#25234=CARTESIAN_POINT('Ctrl Pts',(-39.0762688052762,12.044013228943,8.87476947970419));
#25235=CARTESIAN_POINT('Ctrl Pts',(-39.2303958882198,12.0718450467039,9.06634009532744));
#25236=CARTESIAN_POINT('Ctrl Pts',(-39.3891252359321,12.1010522527167,9.25364450340887));
#25237=CARTESIAN_POINT('Ctrl Pts',(-39.5479128119392,12.1302701731048,9.44101762226405));
#25238=CARTESIAN_POINT('Ctrl Pts',(-39.7113057183253,12.1608644313193,9.62412107874949));
#25239=CARTESIAN_POINT('Ctrl Pts',(-39.8789509826186,12.1927664798387,9.80260437466047));
#25240=CARTESIAN_POINT('Ctrl Pts',(-40.0468697110622,12.224720567207,9.98137881379611));
#25241=CARTESIAN_POINT('Ctrl Pts',(-40.2190543317695,12.2579866432889,10.1555177270919));
#25242=CARTESIAN_POINT('Ctrl Pts',(-40.3951188515065,12.2924858372374,10.3247095747703));
#25243=CARTESIAN_POINT('Ctrl Pts',(-40.4460074573697,12.3024572720618,10.3736117457735));
#25244=CARTESIAN_POINT('Ctrl Pts',(-40.4972200117263,12.3125316625312,10.4221009095722));
#25245=CARTESIAN_POINT('Ctrl Pts',(-40.548746775169,12.3227069631096,10.4701702229062));
#25246=CARTESIAN_POINT('Ctrl Pts',(-43.6022501387951,9.2071267414949,0.));
#25247=CARTESIAN_POINT('Ctrl Pts',(-43.6626214009754,9.0015211042918,1.72780310113343));
#25248=CARTESIAN_POINT('Ctrl Pts',(-44.4422916060602,9.00712069306803,3.28449990511991));
#25249=CARTESIAN_POINT('Ctrl Pts',(-45.2219618111451,9.01272028184427,4.84119670910639));
#25250=CARTESIAN_POINT('Ctrl Pts',(-46.5784649818697,9.18769331133252,5.91846432228298));
#25251=CARTESIAN_POINT('Ctrl Pts',(-47.9349681525942,9.36266634082079,6.99573193545957));
#25252=CARTESIAN_POINT('Ctrl Pts',(-49.6115894684566,9.6316345385918,7.3802042952164));
#25253=CARTESIAN_POINT('Ctrl Pts',(-51.288210784319,9.90060273636281,7.76467665497322));
#25254=CARTESIAN_POINT('Ctrl Pts',(-52.9648321001814,10.1695709341338,7.3802042952164));
#25255=CARTESIAN_POINT('Ctrl Pts',(-41.297758521112,9.7668686911207,0.));
#25256=CARTESIAN_POINT('Ctrl Pts',(-41.3581297832923,9.56126305391757,2.19648874705824));
#25257=CARTESIAN_POINT('Ctrl Pts',(-42.3329177592893,9.6241543894767,4.17545672685568));
#25258=CARTESIAN_POINT('Ctrl Pts',(-43.3077057352862,9.68704572503582,6.15442470665313));
#25259=CARTESIAN_POINT('Ctrl Pts',(-45.0157989803435,9.96525491500233,7.5239130403414));
#25260=CARTESIAN_POINT('Ctrl Pts',(-46.7238922254008,10.2434641049689,8.89340137402967));
#25261=CARTESIAN_POINT('Ctrl Pts',(-48.8389391928256,10.6411656892224,9.3821661014496));
#25262=CARTESIAN_POINT('Ctrl Pts',(-50.9539861602504,11.0388672734759,9.87093082886954));
#25263=CARTESIAN_POINT('Ctrl Pts',(-53.0690331276751,11.4365688577294,9.3821661014496));
#25264=CARTESIAN_POINT('Ctrl Pts',(-38.9283465500519,9.8662647551278,-1.05434036998093E-14));
#25265=CARTESIAN_POINT('Ctrl Pts',(-38.9887178122322,9.66065911792467,2.70899372698069));
#25266=CARTESIAN_POINT('Ctrl Pts',(-40.1768659159253,9.78619863951209,5.14971273833323));
#25267=CARTESIAN_POINT('Ctrl Pts',(-41.3650140196184,9.9117381610995,7.59043174968577));
#25268=CARTESIAN_POINT('Ctrl Pts',(-43.4575689300874,10.3028354815501,9.27946171175751));
#25269=CARTESIAN_POINT('Ctrl Pts',(-45.5501238405564,10.6939328020007,10.9684916738292));
#25270=CARTESIAN_POINT('Ctrl Pts',(-48.1445866631609,11.2324035824697,11.5712994880388));
#25271=CARTESIAN_POINT('Ctrl Pts',(-50.7390494857654,11.7708743629386,12.1741073022483));
#25272=CARTESIAN_POINT('Ctrl Pts',(-53.3335123083699,12.3093451434076,11.5712994880388));
#25273=CARTESIAN_POINT('Ctrl Pts',(-36.5850719698905,9.50149509066535,0.));
#25274=CARTESIAN_POINT('Ctrl Pts',(-36.6454432320708,9.29588945346225,3.24562220582793));
#25275=CARTESIAN_POINT('Ctrl Pts',(-38.0569942786769,9.4870259976893,6.16982677025167));
#25276=CARTESIAN_POINT('Ctrl Pts',(-39.4685453252829,9.67816254191635,9.0940313346754));
#25277=CARTESIAN_POINT('Ctrl Pts',(-41.9636584288765,10.1874616128177,11.1176436806954));
#25278=CARTESIAN_POINT('Ctrl Pts',(-44.4587715324702,10.6967606837192,13.1412560267153));
#25279=CARTESIAN_POINT('Ctrl Pts',(-47.5552162112105,11.382626636124,13.8634749112255));
#25280=CARTESIAN_POINT('Ctrl Pts',(-50.6516608899508,12.0684925885288,14.5856937957357));
#25281=CARTESIAN_POINT('Ctrl Pts',(-53.7481055686911,12.7543585409336,13.8634749112255));
#25282=CARTESIAN_POINT('',(-36.5850719698905,9.50149509066535,0.));
#25283=CARTESIAN_POINT('Ctrl Pts',(-36.5850719698905,9.50149509066535,0.));
#25284=CARTESIAN_POINT('Ctrl Pts',(-36.6454432320708,9.29588945346226,3.24562220582793));
#25285=CARTESIAN_POINT('Ctrl Pts',(-38.0569942786768,9.4870259976893,6.16982677025168));
#25286=CARTESIAN_POINT('Ctrl Pts',(-39.235410774219,9.64659405380718,8.61106394926975));
#25287=CARTESIAN_POINT('Ctrl Pts',(-41.1968615496291,10.0334970568409,10.4489096280657));
#25288=CARTESIAN_POINT('Origin',(-39.3537269950292,-8.28430119040609,0.));
#25289=CARTESIAN_POINT('Ctrl Pts',(-36.5850719698905,9.50149509066535,0.));
#25290=CARTESIAN_POINT('Ctrl Pts',(-36.6454432320708,9.29588945346225,3.24562220582793));
#25291=CARTESIAN_POINT('Ctrl Pts',(-38.0569942786768,9.4870259976893,6.16982677025168));
#25292=CARTESIAN_POINT('Ctrl Pts',(-39.4685453252829,9.67816254191635,9.0940313346754));
#25293=CARTESIAN_POINT('Ctrl Pts',(-41.9636584288765,10.1874616128177,11.1176436806954));
#25294=CARTESIAN_POINT('Ctrl Pts',(-44.4587715324702,10.6967606837192,13.1412560267153));
#25295=CARTESIAN_POINT('Ctrl Pts',(-47.5552162112105,11.382626636124,13.8634749112255));
#25296=CARTESIAN_POINT('Ctrl Pts',(-50.6516608899508,12.0684925885288,14.5856937957357));
#25297=CARTESIAN_POINT('Ctrl Pts',(-53.7481055686911,12.7543585409336,13.8634749112255));
#25298=CARTESIAN_POINT('Ctrl Pts',(-35.7793349404725,10.0094201239377,0.));
#25299=CARTESIAN_POINT('Ctrl Pts',(-35.8397062026528,9.80381448673455,3.38941559469372));
#25300=CARTESIAN_POINT('Ctrl Pts',(-37.3111196447714,10.0125282162148,6.44317352589574));
#25301=CARTESIAN_POINT('Ctrl Pts',(-38.78253308689,10.2212419456951,9.49693145709775));
#25302=CARTESIAN_POINT('Ctrl Pts',(-41.3855144999133,10.7622140099936,11.6101975146502));
#25303=CARTESIAN_POINT('Ctrl Pts',(-43.9884959129367,11.303186074292,13.7234635722027));
#25304=CARTESIAN_POINT('Ctrl Pts',(-47.2194501734233,12.0285476034516,14.4776794959001));
#25305=CARTESIAN_POINT('Ctrl Pts',(-50.45040443391,12.7539091326112,15.2318954195974));
#25306=CARTESIAN_POINT('Ctrl Pts',(-53.6813586943966,13.4792706617708,14.4776794959001));
#25307=CARTESIAN_POINT('Ctrl Pts',(-35.5109929990847,10.9233088493809,6.24500451351652E-15));
#25308=CARTESIAN_POINT('Ctrl Pts',(-35.571364261265,10.7177032121778,3.38941559469373));
#25309=CARTESIAN_POINT('Ctrl Pts',(-37.0427777033836,10.9264169416581,6.44317352589575));
#25310=CARTESIAN_POINT('Ctrl Pts',(-38.5141911455021,11.1351306711383,9.49693145709774));
#25311=CARTESIAN_POINT('Ctrl Pts',(-41.1171725585255,11.6761027354368,11.6101975146502));
#25312=CARTESIAN_POINT('Ctrl Pts',(-43.7201539715489,12.2170747997352,13.7234635722027));
#25313=CARTESIAN_POINT('Ctrl Pts',(-46.9511082320355,12.9424363288948,14.4776794959001));
#25314=CARTESIAN_POINT('Ctrl Pts',(-50.1820624925221,13.6677978580544,15.2318954195974));
#25315=CARTESIAN_POINT('Ctrl Pts',(-53.4130167530088,14.393159387214,14.4776794959001));
#25316=CARTESIAN_POINT('Ctrl Pts',(-35.914217116421,11.7862169042734,0.));
#25317=CARTESIAN_POINT('Ctrl Pts',(-35.9745883786013,11.5806112670703,3.24562220582793));
#25318=CARTESIAN_POINT('Ctrl Pts',(-37.3861394252073,11.7717478112973,6.16982677025167));
#25319=CARTESIAN_POINT('Ctrl Pts',(-38.7976904718133,11.9628843555244,9.09403133467541));
#25320=CARTESIAN_POINT('Ctrl Pts',(-41.292803575407,12.4721834264258,11.1176436806954));
#25321=CARTESIAN_POINT('Ctrl Pts',(-43.7879166790007,12.9814824973272,13.1412560267153));
#25322=CARTESIAN_POINT('Ctrl Pts',(-46.884361357741,13.667348449732,13.8634749112255));
#25323=CARTESIAN_POINT('Ctrl Pts',(-49.9808060364812,14.3532144021369,14.5856937957357));
#25324=CARTESIAN_POINT('Ctrl Pts',(-53.0772507152215,15.0390803545417,13.8634749112255));
#25325=CARTESIAN_POINT('',(-35.817871303676,10.5170811194858,-1.62623179275245E-29));
#25326=CARTESIAN_POINT('Origin',(-37.5449600575353,11.0241949492053,0.));
#25327=CARTESIAN_POINT('Origin',(-37.5449600575353,11.0241949492053,0.));
#25328=CARTESIAN_POINT('Ctrl Pts',(-33.8713086176151,16.7773762111444,0.));
#25329=CARTESIAN_POINT('Ctrl Pts',(-33.9603261204012,16.5824550692827,3.24562220582792));
#25330=CARTESIAN_POINT('Ctrl Pts',(-35.3303080462616,16.9725307779979,6.16982677025168));
#25331=CARTESIAN_POINT('Ctrl Pts',(-36.7002899721219,17.3626064867131,9.09403133467542));
#25332=CARTESIAN_POINT('Ctrl Pts',(-39.097525607069,18.2218132452328,11.1176436806954));
#25333=CARTESIAN_POINT('Ctrl Pts',(-41.494761242016,19.0810200037526,13.1412560267153));
#25334=CARTESIAN_POINT('Ctrl Pts',(-44.4620796765376,20.2005748533761,13.8634749112255));
#25335=CARTESIAN_POINT('Ctrl Pts',(-47.4293981110592,21.3201297029996,14.5856937957357));
#25336=CARTESIAN_POINT('Ctrl Pts',(-50.3967165455808,22.439684552623,13.8634749112255));
#25337=CARTESIAN_POINT('Ctrl Pts',(-35.8811107143581,18.0362202038895,-1.05434036998093E-14));
#25338=CARTESIAN_POINT('Ctrl Pts',(-35.9701282171443,17.8412990620278,2.7089937269807));
#25339=CARTESIAN_POINT('Ctrl Pts',(-37.1283165495982,18.1346518775203,5.14971273833323));
#25340=CARTESIAN_POINT('Ctrl Pts',(-38.2865048820522,18.4280046930127,7.59043174968579));
#25341=CARTESIAN_POINT('Ctrl Pts',(-40.3021016488386,19.1129228203183,9.27946171175751));
#25342=CARTESIAN_POINT('Ctrl Pts',(-42.317698415625,19.7978409476239,10.9684916738293));
#25343=CARTESIAN_POINT('Ctrl Pts',(-44.8091209655645,20.7000614289634,11.5712994880388));
#25344=CARTESIAN_POINT('Ctrl Pts',(-47.300543515504,21.602281910303,12.1741073022483));
#25345=CARTESIAN_POINT('Ctrl Pts',(-49.7919660654436,22.5045023916425,11.5712994880388));
#25346=CARTESIAN_POINT('Ctrl Pts',(-37.6067022235296,19.6629735993424,0.));
#25347=CARTESIAN_POINT('Ctrl Pts',(-37.6957197263158,19.4680524574808,2.19648874705824));
#25348=CARTESIAN_POINT('Ctrl Pts',(-38.6516353959964,19.6690304430805,4.17545672685568));
#25349=CARTESIAN_POINT('Ctrl Pts',(-39.6075510656771,19.8700084286802,6.15442470665314));
#25350=CARTESIAN_POINT('Ctrl Pts',(-41.2586650884905,20.3884728641634,7.52391304034141));
#25351=CARTESIAN_POINT('Ctrl Pts',(-42.909779111304,20.9069372996466,8.89340137402968));
#25352=CARTESIAN_POINT('Ctrl Pts',(-44.9466991136022,21.6015934223202,9.38216610144961));
#25353=CARTESIAN_POINT('Ctrl Pts',(-46.9836191159004,22.2962495449937,9.87093082886954));
#25354=CARTESIAN_POINT('Ctrl Pts',(-49.0205391181987,22.9909056676674,9.38216610144961));
#25355=CARTESIAN_POINT('Ctrl Pts',(-38.9817677587447,21.5951194116471,1.04083408558608E-14));
#25356=CARTESIAN_POINT('Ctrl Pts',(-39.0707852615308,21.4001982697854,1.72780310113343));
#25357=CARTESIAN_POINT('Ctrl Pts',(-39.8417226435484,21.516699501965,3.28449990511991));
#25358=CARTESIAN_POINT('Ctrl Pts',(-40.6126600255661,21.6332007341446,4.84119670910638));
#25359=CARTESIAN_POINT('Ctrl Pts',(-41.9304546915349,21.9994433198418,5.91846432228298));
#25360=CARTESIAN_POINT('Ctrl Pts',(-43.2482493575037,22.365685905539,6.99573193545957));
#25361=CARTESIAN_POINT('Ctrl Pts',(-44.8695269202925,22.8705244862893,7.38020429521639));
#25362=CARTESIAN_POINT('Ctrl Pts',(-46.4908044830812,23.3753630670397,7.76467665497322));
#25363=CARTESIAN_POINT('Ctrl Pts',(-48.11208204587,23.88020164779,7.38020429521639));
#25364=CARTESIAN_POINT('',(-33.8713086176317,16.7773762111466,1.5794947023715E-9));
#25365=CARTESIAN_POINT('Origin',(-24.3164988679736,32.0320676419193,0.));
#25366=CARTESIAN_POINT('Ctrl Pts',(-33.8713086177735,16.7773762110018,3.13106388084265E-9));
#25367=CARTESIAN_POINT('Ctrl Pts',(-33.8780292657697,16.7626600447503,0.245038153335515));
#25368=CARTESIAN_POINT('Ctrl Pts',(-33.8905743368632,16.7504469217305,0.490791160521789));
#25369=CARTESIAN_POINT('Ctrl Pts',(-33.9090089481601,16.7408009061956,0.736766500725478));
#25370=CARTESIAN_POINT('Ctrl Pts',(-33.9273830396633,16.731186557988,0.981934317701124));
#25371=CARTESIAN_POINT('Ctrl Pts',(-33.9516081464474,16.7241225568762,1.22732257376577));
#25372=CARTESIAN_POINT('Ctrl Pts',(-33.9817020661515,16.7196526308054,1.47243294816354));
#25373=CARTESIAN_POINT('Ctrl Pts',(-34.0117506633926,16.7151894365947,1.71717417803031));
#25374=CARTESIAN_POINT('Ctrl Pts',(-34.0476504419798,16.713312556215,1.96163791541602));
#25375=CARTESIAN_POINT('Ctrl Pts',(-34.0893716276067,16.7140449789782,2.20532408778542));
#25376=CARTESIAN_POINT('Ctrl Pts',(-34.1310570310094,16.7147767735782,2.44880126242085));
#25377=CARTESIAN_POINT('Ctrl Pts',(-34.1785538334838,16.7181134182572,2.6915017543107));
#25378=CARTESIAN_POINT('Ctrl Pts',(-34.2317848413855,16.7240568140042,2.9329295186683));
#25379=CARTESIAN_POINT('Ctrl Pts',(-34.2850047132543,16.7299989663809,3.17430677585617));
#25380=CARTESIAN_POINT('Ctrl Pts',(-34.3439563059026,16.7385467737467,3.41441139318376));
#25381=CARTESIAN_POINT('Ctrl Pts',(-34.4085158144079,16.7496809885027,3.65275710614674));
#25382=CARTESIAN_POINT('Ctrl Pts',(-34.4731572995457,16.7608293413068,3.89140546668823));
#25383=CARTESIAN_POINT('Ctrl Pts',(-34.5434208142137,16.7745706450852,4.12829002081196));
#25384=CARTESIAN_POINT('Ctrl Pts',(-34.6191369553178,16.7908646265308,4.36293874377837));
#25385=CARTESIAN_POINT('Ctrl Pts',(-34.6949303570796,16.8071752343352,4.59782690201464));
#25386=CARTESIAN_POINT('Ctrl Pts',(-34.7761873205119,16.8260436742454,4.83047425894961));
#25387=CARTESIAN_POINT('Ctrl Pts',(-34.8626952586805,16.8474092210266,5.0604297595942));
#25388=CARTESIAN_POINT('Ctrl Pts',(-34.9494561121503,16.8688372322916,5.29105755998298));
#25389=CARTESIAN_POINT('Ctrl Pts',(-35.0414984482315,16.8927768946317,5.51897736305686));
#25390=CARTESIAN_POINT('Ctrl Pts',(-35.1385682021254,16.9191475261007,5.74376259354333));
#25391=CARTESIAN_POINT('Ctrl Pts',(-35.2004627636792,16.9359622248837,5.88709234072621));
#25392=CARTESIAN_POINT('Ctrl Pts',(-35.2644005416947,16.9537648979136,6.02914825314193));
#25393=CARTESIAN_POINT('Ctrl Pts',(-35.3303080462913,16.9725307780171,6.16982677023484));
#25394=CARTESIAN_POINT('Ctrl Pts',(-35.4336529523065,17.0019562300572,6.39041482339095));
#25395=CARTESIAN_POINT('Ctrl Pts',(-35.5425242743014,17.0337488912442,6.60890054011814));
#25396=CARTESIAN_POINT('Ctrl Pts',(-35.6567853708684,17.067880599445,6.82480412008055));
#25397=CARTESIAN_POINT('Ctrl Pts',(-35.7707885165966,17.1019352533989,7.04022028559297));
#25398=CARTESIAN_POINT('Ctrl Pts',(-35.8901570371289,17.138318392999,7.25306552029633));
#25399=CARTESIAN_POINT('Ctrl Pts',(-36.0147088875609,17.1769825010546,7.46287566269405));
#25400=CARTESIAN_POINT('Ctrl Pts',(-36.1390604075859,17.2155844213829,7.67234834441897));
#25401=CARTESIAN_POINT('Ctrl Pts',(-36.2685784477697,17.2564599421024,7.8787952653307));
#25402=CARTESIAN_POINT('Ctrl Pts',(-36.4030374099059,17.2995426324479,8.08177334612262));
#25403=CARTESIAN_POINT('Ctrl Pts',(-36.5373673538294,17.3425839834017,8.28455666214181));
#25404=CARTESIAN_POINT('Ctrl Pts',(-36.6766285382468,17.3878282101255,8.48387739272927));
#25405=CARTESIAN_POINT('Ctrl Pts',(-36.8205542765639,17.4351906738842,8.67931873611171));
#25406=CARTESIAN_POINT('Ctrl Pts',(-36.9644869373279,17.482555415652,8.87476947970536));
#25407=CARTESIAN_POINT('Ctrl Pts',(-37.1130843481565,17.5320385165208,9.06634009532841));
#25408=CARTESIAN_POINT('Ctrl Pts',(-37.2660414411776,17.5835379767386,9.25364450340966));
#25409=CARTESIAN_POINT('Ctrl Pts',(-37.419054644999,17.6350563290252,9.44101762226471));
#25410=CARTESIAN_POINT('Ctrl Pts',(-37.5764304302811,17.6885924168517,9.62412107875002));
#25411=CARTESIAN_POINT('Ctrl Pts',(-37.7378291726328,17.7440281571912,9.80260437466088));
#25412=CARTESIAN_POINT('Ctrl Pts',(-37.8994911897636,17.7995543247056,9.98137881379651));
#25413=CARTESIAN_POINT('Ctrl Pts',(-38.0651889630643,17.8569862265478,10.1555177270923));
#25414=CARTESIAN_POINT('Ctrl Pts',(-38.2345516526471,17.9161908620977,10.3247095747707));
#25415=CARTESIAN_POINT('Ctrl Pts',(-38.2835032027434,17.9333030058065,10.3736117457738));
#25416=CARTESIAN_POINT('Ctrl Pts',(-38.3327607518886,17.9505631598978,10.4221009095723));
#25417=CARTESIAN_POINT('Ctrl Pts',(-38.3823149509186,17.967967913594,10.4701702229062));
#25418=CARTESIAN_POINT('Ctrl Pts',(-41.8481313484578,15.3186586437009,0.));
#25419=CARTESIAN_POINT('Ctrl Pts',(-41.9371488512439,15.1237375018392,1.72780310113342));
#25420=CARTESIAN_POINT('Ctrl Pts',(-42.7080862332615,15.2402387340188,3.28449990511991));
#25421=CARTESIAN_POINT('Ctrl Pts',(-43.4790236152791,15.3567399661984,4.84119670910639));
#25422=CARTESIAN_POINT('Ctrl Pts',(-44.796818281248,15.7229825518956,5.91846432228298));
#25423=CARTESIAN_POINT('Ctrl Pts',(-46.1146129472168,16.0892251375928,6.99573193545957));
#25424=CARTESIAN_POINT('Ctrl Pts',(-47.7358905100055,16.5940637183432,7.38020429521639));
#25425=CARTESIAN_POINT('Ctrl Pts',(-49.3571680727943,17.0989022990935,7.76467665497321));
#25426=CARTESIAN_POINT('Ctrl Pts',(-50.978445635583,17.6037408798438,7.38020429521639));
#25427=CARTESIAN_POINT('Ctrl Pts',(-39.4874365476043,15.5447398754881,0.));
#25428=CARTESIAN_POINT('Ctrl Pts',(-39.5764540503904,15.3498187336264,2.19648874705823));
#25429=CARTESIAN_POINT('Ctrl Pts',(-40.5323697200711,15.5507967192261,4.17545672685568));
#25430=CARTESIAN_POINT('Ctrl Pts',(-41.4882853897518,15.7517747048258,6.15442470665314));
#25431=CARTESIAN_POINT('Ctrl Pts',(-43.1393994125653,16.270239140309,7.5239130403414));
#25432=CARTESIAN_POINT('Ctrl Pts',(-44.7905134353787,16.7887035757922,8.89340137402966));
#25433=CARTESIAN_POINT('Ctrl Pts',(-46.8274334376769,17.4833596984658,9.3821661014496));
#25434=CARTESIAN_POINT('Ctrl Pts',(-48.8643534399751,18.1780158211394,9.87093082886953));
#25435=CARTESIAN_POINT('Ctrl Pts',(-50.9012734422734,18.872671943813,9.3821661014496));
#25436=CARTESIAN_POINT('Ctrl Pts',(-37.1279962392256,15.3059217494167,0.));
#25437=CARTESIAN_POINT('Ctrl Pts',(-37.2170137420117,15.111000607555,2.70899372698069));
#25438=CARTESIAN_POINT('Ctrl Pts',(-38.3752020744657,15.4043534230475,5.14971273833323));
#25439=CARTESIAN_POINT('Ctrl Pts',(-39.5333904069197,15.69770623854,7.59043174968578));
#25440=CARTESIAN_POINT('Ctrl Pts',(-41.5489871737061,16.3826243658455,9.27946171175751));
#25441=CARTESIAN_POINT('Ctrl Pts',(-43.5645839404925,17.0675424931511,10.9684916738293));
#25442=CARTESIAN_POINT('Ctrl Pts',(-46.056006490432,17.9697629744906,11.5712994880388));
#25443=CARTESIAN_POINT('Ctrl Pts',(-48.5474290403715,18.8719834558302,12.1741073022483));
#25444=CARTESIAN_POINT('Ctrl Pts',(-51.038851590311,19.7742039371697,11.5712994880388));
#25445=CARTESIAN_POINT('Ctrl Pts',(-34.8604849513722,14.6113821712785,0.));
#25446=CARTESIAN_POINT('Ctrl Pts',(-34.9495024541584,14.4164610294168,3.24562220582793));
#25447=CARTESIAN_POINT('Ctrl Pts',(-36.3194843800187,14.806536738132,6.16982677025168));
#25448=CARTESIAN_POINT('Ctrl Pts',(-37.6894663058791,15.1966124468471,9.09403133467541));
#25449=CARTESIAN_POINT('Ctrl Pts',(-40.0867019408261,16.0558192053669,11.1176436806954));
#25450=CARTESIAN_POINT('Ctrl Pts',(-42.4839375757731,16.9150259638866,13.1412560267153));
#25451=CARTESIAN_POINT('Ctrl Pts',(-45.4512560102947,18.0345808135101,13.8634749112255));
#25452=CARTESIAN_POINT('Ctrl Pts',(-48.4185744448163,19.1541356631336,14.5856937957357));
#25453=CARTESIAN_POINT('Ctrl Pts',(-51.3858928793379,20.2736905127571,13.8634749112255));
#25454=CARTESIAN_POINT('',(-34.8604849513722,14.6113821712785,0.));
#25455=CARTESIAN_POINT('Ctrl Pts',(-34.8604849513722,14.6113821712785,0.));
#25456=CARTESIAN_POINT('Ctrl Pts',(-34.9495024541584,14.4164610294168,3.24562220582793));
#25457=CARTESIAN_POINT('Ctrl Pts',(-36.3194843800187,14.806536738132,6.16982677025168));
#25458=CARTESIAN_POINT('Ctrl Pts',(-37.4631973926725,15.1321867744983,8.61106394926977));
#25459=CARTESIAN_POINT('Ctrl Pts',(-39.3496213890632,15.7942952127127,10.4489096280657));
#25460=CARTESIAN_POINT('Origin',(-40.1321417817282,-2.59935965651507,0.));
#25461=CARTESIAN_POINT('Ctrl Pts',(-34.8604849513722,14.6113821712785,0.));
#25462=CARTESIAN_POINT('Ctrl Pts',(-34.9495024541584,14.4164610294168,3.24562220582793));
#25463=CARTESIAN_POINT('Ctrl Pts',(-36.3194843800187,14.806536738132,6.16982677025168));
#25464=CARTESIAN_POINT('Ctrl Pts',(-37.6894663058791,15.1966124468471,9.09403133467541));
#25465=CARTESIAN_POINT('Ctrl Pts',(-40.0867019408261,16.0558192053669,11.1176436806954));
#25466=CARTESIAN_POINT('Ctrl Pts',(-42.4839375757731,16.9150259638866,13.1412560267153));
#25467=CARTESIAN_POINT('Ctrl Pts',(-45.4512560102947,18.0345808135101,13.8634749112255));
#25468=CARTESIAN_POINT('Ctrl Pts',(-48.4185744448163,19.1541356631336,14.5856937957357));
#25469=CARTESIAN_POINT('Ctrl Pts',(-51.3858928793379,20.2736905127571,13.8634749112255));
#25470=CARTESIAN_POINT('Ctrl Pts',(-33.9906638941717,14.9994689250471,0.));
#25471=CARTESIAN_POINT('Ctrl Pts',(-34.0796813969579,14.8045477831854,3.38941559469373));
#25472=CARTESIAN_POINT('Ctrl Pts',(-35.5064149111822,15.2205410738881,6.44317352589574));
#25473=CARTESIAN_POINT('Ctrl Pts',(-36.9331484254066,15.6365343645909,9.49693145709775));
#25474=CARTESIAN_POINT('Ctrl Pts',(-39.4326468889937,16.5424429921149,11.6101975146502));
#25475=CARTESIAN_POINT('Ctrl Pts',(-41.9321453525808,17.4483516196389,13.7234635722027));
#25476=CARTESIAN_POINT('Ctrl Pts',(-45.026983448635,18.6261427473661,14.4776794959001));
#25477=CARTESIAN_POINT('Ctrl Pts',(-48.1218215446892,19.8039338750934,15.2318954195974));
#25478=CARTESIAN_POINT('Ctrl Pts',(-51.2166596407434,20.9817250028206,14.4776794959001));
#25479=CARTESIAN_POINT('Ctrl Pts',(-33.5949933606689,15.8658665409935,0.));
#25480=CARTESIAN_POINT('Ctrl Pts',(-33.684010863455,15.6709453991318,3.38941559469373));
#25481=CARTESIAN_POINT('Ctrl Pts',(-35.1107443776794,16.0869386898345,6.44317352589574));
#25482=CARTESIAN_POINT('Ctrl Pts',(-36.5374778919038,16.5029319805373,9.49693145709774));
#25483=CARTESIAN_POINT('Ctrl Pts',(-39.0369763554909,17.4088406080613,11.6101975146502));
#25484=CARTESIAN_POINT('Ctrl Pts',(-41.536474819078,18.3147492355853,13.7234635722027));
#25485=CARTESIAN_POINT('Ctrl Pts',(-44.6313129151321,19.4925403633125,14.4776794959001));
#25486=CARTESIAN_POINT('Ctrl Pts',(-47.7261510111863,20.6703314910398,15.2318954195974));
#25487=CARTESIAN_POINT('Ctrl Pts',(-50.8209891072405,21.848122618767,14.4776794959001));
#25488=CARTESIAN_POINT('Ctrl Pts',(-33.8713086176151,16.7773762111444,0.));
#25489=CARTESIAN_POINT('Ctrl Pts',(-33.9603261204012,16.5824550692827,3.24562220582792));
#25490=CARTESIAN_POINT('Ctrl Pts',(-35.3303080462616,16.9725307779979,6.16982677025167));
#25491=CARTESIAN_POINT('Ctrl Pts',(-36.7002899721219,17.3626064867131,9.09403133467541));
#25492=CARTESIAN_POINT('Ctrl Pts',(-39.097525607069,18.2218132452328,11.1176436806954));
#25493=CARTESIAN_POINT('Ctrl Pts',(-41.494761242016,19.0810200037526,13.1412560267153));
#25494=CARTESIAN_POINT('Ctrl Pts',(-44.4620796765376,20.2005748533761,13.8634749112255));
#25495=CARTESIAN_POINT('Ctrl Pts',(-47.4293981110592,21.3201297029996,14.5856937957357));
#25496=CARTESIAN_POINT('Ctrl Pts',(-50.3967165455808,22.439684552623,13.8634749112255));
#25497=CARTESIAN_POINT('',(-33.9565603202845,15.5074469599424,-1.75233474473625E-29));
#25498=CARTESIAN_POINT('Origin',(-35.5938999782223,16.255189458764,0.));
#25499=CARTESIAN_POINT('Origin',(-35.5938999782223,16.255189458764,0.));
#25500=CARTESIAN_POINT('Ctrl Pts',(-39.2421052839111,21.1183468312849,1.04083408558608E-14));
#25501=CARTESIAN_POINT('Ctrl Pts',(-39.3579568876516,20.9380782171067,1.72780310113343));
#25502=CARTESIAN_POINT('Ctrl Pts',(-40.1044673847039,21.1631094635643,3.28449990511991));
#25503=CARTESIAN_POINT('Ctrl Pts',(-40.8509778817562,21.3881407100219,4.84119670910639));
#25504=CARTESIAN_POINT('Ctrl Pts',(-42.1032375437762,21.9381972090397,5.91846432228298));
#25505=CARTESIAN_POINT('Ctrl Pts',(-43.3554972057962,22.4882537080574,6.99573193545956));
#25506=CARTESIAN_POINT('Ctrl Pts',(-44.8884264797114,23.2186856141172,7.38020429521639));
#25507=CARTESIAN_POINT('Ctrl Pts',(-45.6451607014124,23.5792650807263,7.56999999999999));
#25508=CARTESIAN_POINT('Ctrl Pts',(-46.4213557536266,23.949117520177,7.56999999999998));
#25509=CARTESIAN_POINT('Ctrl Pts',(-36.8732642383512,21.0061649833186,-1.05434036998093E-14));
#25510=CARTESIAN_POINT('Ctrl Pts',(-36.9891158420917,20.8258963691405,2.19648874705824));
#25511=CARTESIAN_POINT('Ctrl Pts',(-37.9066995190544,21.1608696725666,4.17545672685568));
#25512=CARTESIAN_POINT('Ctrl Pts',(-38.8242831960172,21.4958429759927,6.15442470665315));
#25513=CARTESIAN_POINT('Ctrl Pts',(-40.384806076502,22.2440082162141,7.52391304034141));
#25514=CARTESIAN_POINT('Ctrl Pts',(-41.9453289569868,22.9921734564355,8.89340137402968));
#25515=CARTESIAN_POINT('Ctrl Pts',(-43.8626561769039,23.9696429220944,9.38216610144962));
#25516=CARTESIAN_POINT('Ctrl Pts',(-44.8091493688595,24.4521730739537,9.62344598428098));
#25517=CARTESIAN_POINT('Ctrl Pts',(-45.779983396821,24.9471123877533,9.62344598428098));
#25518=CARTESIAN_POINT('Ctrl Pts',(-34.5718269932683,20.4339943155209,-1.05434036998093E-14));
#25519=CARTESIAN_POINT('Ctrl Pts',(-34.6876785970088,20.2537257013428,2.70899372698069));
#25520=CARTESIAN_POINT('Ctrl Pts',(-35.7923297837143,20.7089199933766,5.14971273833323));
#25521=CARTESIAN_POINT('Ctrl Pts',(-36.8969809704197,21.1641142854104,7.59043174968577));
#25522=CARTESIAN_POINT('Ctrl Pts',(-38.7945878558529,22.1289102616397,9.27946171175752));
#25523=CARTESIAN_POINT('Ctrl Pts',(-40.692194741286,23.0937062378691,10.9684916738293));
#25524=CARTESIAN_POINT('Ctrl Pts',(-43.0298588401131,24.3413098128681,11.5712994880388));
#25525=CARTESIAN_POINT('Ctrl Pts',(-44.1838523429616,24.9571923172886,11.8688770148585));
#25526=CARTESIAN_POINT('Ctrl Pts',(-45.3675229389402,25.5889133878672,11.8688770148585));
#25527=CARTESIAN_POINT('Ctrl Pts',(-32.4262389885812,19.423823646631,1.04083408558608E-14));
#25528=CARTESIAN_POINT('Ctrl Pts',(-32.5420905923217,19.2435550324529,3.24562220582793));
#25529=CARTESIAN_POINT('Ctrl Pts',(-33.8426145161274,19.8246290891123,6.16982677025167));
#25530=CARTESIAN_POINT('Ctrl Pts',(-35.1431384399332,20.4057031457716,9.09403133467541));
#25531=CARTESIAN_POINT('Ctrl Pts',(-37.3936958017627,21.5973266200539,11.1176436806954));
#25532=CARTESIAN_POINT('Ctrl Pts',(-39.6442531635923,22.7889500943362,13.1412560267153));
#25533=CARTESIAN_POINT('Ctrl Pts',(-42.4220393076081,24.3194029329696,13.8634749112255));
#25534=CARTESIAN_POINT('Ctrl Pts',(-43.7933001162526,25.0749146564396,14.22));
#25535=CARTESIAN_POINT('Ctrl Pts',(-45.199825451624,25.849855771603,14.22));
#25536=CARTESIAN_POINT('',(-32.4262389885812,19.423823646631,6.93889390390723E-15));
#25537=CARTESIAN_POINT('Ctrl Pts',(-32.4262389885812,19.423823646631,6.93889390390723E-15));
#25538=CARTESIAN_POINT('Ctrl Pts',(-32.5420905923217,19.2435550324529,3.24562220582793));
#25539=CARTESIAN_POINT('Ctrl Pts',(-33.8426145161274,19.8246290891123,6.16982677025167));
#25540=CARTESIAN_POINT('Ctrl Pts',(-34.9283413471526,20.3097318100845,8.61106394927297));
#25541=CARTESIAN_POINT('Ctrl Pts',(-36.7013364119536,21.2335670650399,10.4489096280657));
#25542=CARTESIAN_POINT('Origin',(-40.0935818932913,3.13849734404836,0.));
#25543=CARTESIAN_POINT('Ctrl Pts',(-31.1388779521428,21.4269965203143,0.));
#25544=CARTESIAN_POINT('Ctrl Pts',(-31.2547295558833,21.2467279061362,3.24562220582793));
#25545=CARTESIAN_POINT('Ctrl Pts',(-32.555253479689,21.8278019627955,6.16982677025167));
#25546=CARTESIAN_POINT('Ctrl Pts',(-33.8557774034948,22.4088760194548,9.09403133467541));
#25547=CARTESIAN_POINT('Ctrl Pts',(-36.1063347653244,23.6004994937371,11.1176436806954));
#25548=CARTESIAN_POINT('Ctrl Pts',(-38.3568921271539,24.7921229680194,13.1412560267153));
#25549=CARTESIAN_POINT('Ctrl Pts',(-41.1346782711698,26.3225758066528,13.8634749112255));
#25550=CARTESIAN_POINT('Ctrl Pts',(-42.5059390798142,27.0780875301229,14.22));
#25551=CARTESIAN_POINT('Ctrl Pts',(-43.9124644151856,27.8530286452862,14.22));
#25552=CARTESIAN_POINT('Ctrl Pts',(-32.9490709821975,22.9590519566756,-1.05434036998093E-14));
#25553=CARTESIAN_POINT('Ctrl Pts',(-33.0649225859379,22.7787833424975,2.70899372698069));
#25554=CARTESIAN_POINT('Ctrl Pts',(-34.1695737726434,23.2339776345313,5.14971273833322));
#25555=CARTESIAN_POINT('Ctrl Pts',(-35.2742249593488,23.6891719265651,7.59043174968576));
#25556=CARTESIAN_POINT('Ctrl Pts',(-37.171831844782,24.6539679027944,9.27946171175751));
#25557=CARTESIAN_POINT('Ctrl Pts',(-39.0694387302151,25.6187638790238,10.9684916738292));
#25558=CARTESIAN_POINT('Ctrl Pts',(-41.4071028290422,26.8663674540228,11.5712994880388));
#25559=CARTESIAN_POINT('Ctrl Pts',(-42.5610963318907,27.4822499584433,11.8688770148585));
#25560=CARTESIAN_POINT('Ctrl Pts',(-43.7447669278693,28.1139710290219,11.8688770148584));
#25561=CARTESIAN_POINT('Ctrl Pts',(-34.4255873115187,24.8148246247011,0.));
#25562=CARTESIAN_POINT('Ctrl Pts',(-34.5414389152592,24.634556010523,2.19648874705822));
#25563=CARTESIAN_POINT('Ctrl Pts',(-35.459022592222,24.9695293139491,4.17545672685568));
#25564=CARTESIAN_POINT('Ctrl Pts',(-36.3766062691848,25.3045026173752,6.15442470665313));
#25565=CARTESIAN_POINT('Ctrl Pts',(-37.9371291496695,26.0526678575966,7.52391304034139));
#25566=CARTESIAN_POINT('Ctrl Pts',(-39.4976520301543,26.800833097818,8.89340137402967));
#25567=CARTESIAN_POINT('Ctrl Pts',(-41.4149792500714,27.7783025634769,9.38216610144959));
#25568=CARTESIAN_POINT('Ctrl Pts',(-42.361472442027,28.2608327153362,9.62344598428098));
#25569=CARTESIAN_POINT('Ctrl Pts',(-43.3323064699885,28.7557720291358,9.62344598428096));
#25570=CARTESIAN_POINT('Ctrl Pts',(-35.5116836434675,26.92299620782,0.));
#25571=CARTESIAN_POINT('Ctrl Pts',(-35.627535247208,26.7427275936419,1.72780310113342));
#25572=CARTESIAN_POINT('Ctrl Pts',(-36.3740457442603,26.9677588400994,3.28449990511991));
#25573=CARTESIAN_POINT('Ctrl Pts',(-37.1205562413126,27.192790086557,4.84119670910638));
#25574=CARTESIAN_POINT('Ctrl Pts',(-38.3728159033326,27.7428465855748,5.91846432228297));
#25575=CARTESIAN_POINT('Ctrl Pts',(-39.6250755653526,28.2929030845925,6.99573193545956));
#25576=CARTESIAN_POINT('Ctrl Pts',(-41.1580048392677,29.0233349906523,7.38020429521639));
#25577=CARTESIAN_POINT('Ctrl Pts',(-41.9147390609688,29.3839144572614,7.56999999999998));
#25578=CARTESIAN_POINT('Ctrl Pts',(-42.6909341131829,29.7537668967121,7.56999999999998));
#25579=CARTESIAN_POINT('',(-31.1388779521918,21.4269965202911,2.36793890025575E-9));
#25580=CARTESIAN_POINT('Origin',(-19.5103534449751,35.1666259835202,0.));
#25581=CARTESIAN_POINT('Ctrl Pts',(-31.1388779521428,21.4269965203143,0.));
#25582=CARTESIAN_POINT('Ctrl Pts',(-31.2547295558833,21.2467279061362,3.24562220582793));
#25583=CARTESIAN_POINT('Ctrl Pts',(-32.555253479689,21.8278019627955,6.16982677025167));
#25584=CARTESIAN_POINT('Ctrl Pts',(-33.6474974511926,22.3158165419706,8.62571762198518));
#25585=CARTESIAN_POINT('Ctrl Pts',(-35.4345298797236,23.2474528526982,10.4701702229061));
#25586=CARTESIAN_POINT('Ctrl Pts',(-32.4262389885812,19.423823646631,1.04083408558608E-14));
#25587=CARTESIAN_POINT('Ctrl Pts',(-32.5420905923217,19.2435550324529,3.24562220582793));
#25588=CARTESIAN_POINT('Ctrl Pts',(-33.8426145161274,19.8246290891122,6.16982677025167));
#25589=CARTESIAN_POINT('Ctrl Pts',(-35.1431384399332,20.4057031457716,9.09403133467541));
#25590=CARTESIAN_POINT('Ctrl Pts',(-37.3936958017627,21.5973266200539,11.1176436806954));
#25591=CARTESIAN_POINT('Ctrl Pts',(-39.6442531635923,22.7889500943362,13.1412560267153));
#25592=CARTESIAN_POINT('Ctrl Pts',(-42.4220393076081,24.3194029329696,13.8634749112255));
#25593=CARTESIAN_POINT('Ctrl Pts',(-43.7933001162526,25.0749146564396,14.22));
#25594=CARTESIAN_POINT('Ctrl Pts',(-45.199825451624,25.849855771603,14.22));
#25595=CARTESIAN_POINT('Ctrl Pts',(-31.510040951966,19.684171793739,0.));
#25596=CARTESIAN_POINT('Ctrl Pts',(-31.6258925557065,19.5039031795609,3.38941559469373));
#25597=CARTESIAN_POINT('Ctrl Pts',(-32.9789019620468,20.118707607713,6.44317352589574));
#25598=CARTESIAN_POINT('Ctrl Pts',(-34.3319113683871,20.7335120358651,9.49693145709775));
#25599=CARTESIAN_POINT('Ctrl Pts',(-36.6770443017776,21.985915539383,11.6101975146502));
#25600=CARTESIAN_POINT('Ctrl Pts',(-39.0221772351681,23.2383190429009,13.7234635722027));
#25601=CARTESIAN_POINT('Ctrl Pts',(-41.9178971879302,24.8445633383044,14.4776794959001));
#25602=CARTESIAN_POINT('Ctrl Pts',(-43.3473763048115,25.637489696635,14.85));
#25603=CARTESIAN_POINT('Ctrl Pts',(-44.8136171406925,26.4508076337079,14.85));
#25604=CARTESIAN_POINT('Ctrl Pts',(-30.9950965373907,20.4854409432123,0.));
#25605=CARTESIAN_POINT('Ctrl Pts',(-31.1109481411311,20.3051723290341,3.38941559469373));
#25606=CARTESIAN_POINT('Ctrl Pts',(-32.4639575474714,20.9199767571863,6.44317352589574));
#25607=CARTESIAN_POINT('Ctrl Pts',(-33.8169669538117,21.5347811853384,9.49693145709776));
#25608=CARTESIAN_POINT('Ctrl Pts',(-36.1620998872022,22.7871846888563,11.6101975146503));
#25609=CARTESIAN_POINT('Ctrl Pts',(-38.5072328205927,24.0395881923742,13.7234635722027));
#25610=CARTESIAN_POINT('Ctrl Pts',(-41.4029527733549,25.6458324877777,14.4776794959001));
#25611=CARTESIAN_POINT('Ctrl Pts',(-42.8324318902361,26.4387588461083,14.85));
#25612=CARTESIAN_POINT('Ctrl Pts',(-44.2986727261171,27.2520767831812,14.85));
#25613=CARTESIAN_POINT('Ctrl Pts',(-31.1388779521428,21.4269965203143,0.));
#25614=CARTESIAN_POINT('Ctrl Pts',(-31.2547295558833,21.2467279061362,3.24562220582793));
#25615=CARTESIAN_POINT('Ctrl Pts',(-32.555253479689,21.8278019627955,6.16982677025168));
#25616=CARTESIAN_POINT('Ctrl Pts',(-33.8557774034948,22.4088760194548,9.09403133467541));
#25617=CARTESIAN_POINT('Ctrl Pts',(-36.1063347653244,23.6004994937371,11.1176436806954));
#25618=CARTESIAN_POINT('Ctrl Pts',(-38.3568921271539,24.7921229680194,13.1412560267153));
#25619=CARTESIAN_POINT('Ctrl Pts',(-41.1346782711697,26.3225758066528,13.8634749112255));
#25620=CARTESIAN_POINT('Ctrl Pts',(-42.5059390798142,27.0780875301229,14.22));
#25621=CARTESIAN_POINT('Ctrl Pts',(-43.9124644151856,27.8530286452862,14.22));
#25622=CARTESIAN_POINT('',(-31.403991691448,20.1821259000137,-1.84276521465446E-29));
#25623=CARTESIAN_POINT('Origin',(-32.9182507396841,21.1552751870377,0.));
#25624=CARTESIAN_POINT('Origin',(-32.9182507396841,21.1552751870377,0.));
#25625=CARTESIAN_POINT('Ctrl Pts',(-27.7725495286736,25.640424970686,0.));
#25626=CARTESIAN_POINT('Ctrl Pts',(-27.9128768288047,25.4784786333244,3.24562220582793));
#25627=CARTESIAN_POINT('Ctrl Pts',(-29.1174678338685,26.2387220458134,6.16982677025167));
#25628=CARTESIAN_POINT('Ctrl Pts',(-30.3220588389323,26.9989654583025,9.09403133467541));
#25629=CARTESIAN_POINT('Ctrl Pts',(-32.3801230698291,28.4987476307693,11.1176436806954));
#25630=CARTESIAN_POINT('Ctrl Pts',(-34.4381873007258,29.9985298032361,13.1412560267153));
#25631=CARTESIAN_POINT('Ctrl Pts',(-36.9698934388174,31.9087250245464,13.8634749112255));
#25632=CARTESIAN_POINT('Ctrl Pts',(-39.501599576909,33.8189202458566,14.5856937957357));
#25633=CARTESIAN_POINT('Ctrl Pts',(-42.0333057150006,35.7291154671669,13.8634749112255));
#25634=CARTESIAN_POINT('Ctrl Pts',(-29.3462831821136,27.4145036200623,0.));
#25635=CARTESIAN_POINT('Ctrl Pts',(-29.4866104822448,27.2525572827007,2.70899372698069));
#25636=CARTESIAN_POINT('Ctrl Pts',(-30.5152370105913,27.8603266081619,5.14971273833323));
#25637=CARTESIAN_POINT('Ctrl Pts',(-31.5438635389379,28.4680959336232,7.59043174968578));
#25638=CARTESIAN_POINT('Ctrl Pts',(-33.2848507390767,29.6931292949421,9.27946171175752));
#25639=CARTESIAN_POINT('Ctrl Pts',(-35.0258379392155,30.9181626562611,10.9684916738293));
#25640=CARTESIAN_POINT('Ctrl Pts',(-37.1621554871447,32.4857517139243,11.5712994880388));
#25641=CARTESIAN_POINT('Ctrl Pts',(-39.2984730350738,34.0533407715876,12.1741073022483));
#25642=CARTESIAN_POINT('Ctrl Pts',(-41.434790583003,35.6209298292508,11.5712994880388));
#25643=CARTESIAN_POINT('Ctrl Pts',(-30.5436667170411,29.4615173807457,0.));
#25644=CARTESIAN_POINT('Ctrl Pts',(-30.6839940171722,29.2995710433841,2.19648874705824));
#25645=CARTESIAN_POINT('Ctrl Pts',(-31.544566343847,29.7617205741622,4.17545672685568));
#25646=CARTESIAN_POINT('Ctrl Pts',(-32.4051386705217,30.2238701049402,6.15442470665313));
#25647=CARTESIAN_POINT('Ctrl Pts',(-33.8433026630076,31.1865056631393,7.5239130403414));
#25648=CARTESIAN_POINT('Ctrl Pts',(-35.2814666554934,32.1491412213384,8.89340137402968));
#25649=CARTESIAN_POINT('Ctrl Pts',(-37.040169839947,33.3895255704509,9.3821661014496));
#25650=CARTESIAN_POINT('Ctrl Pts',(-38.7988730244006,34.6299099195635,9.87093082886954));
#25651=CARTESIAN_POINT('Ctrl Pts',(-40.5575762088542,35.870294268676,9.38216610144961));
#25652=CARTESIAN_POINT('Ctrl Pts',(-31.3186840564483,31.7027984407114,0.));
#25653=CARTESIAN_POINT('Ctrl Pts',(-31.4590113565795,31.5408521033498,1.72780310113343));
#25654=CARTESIAN_POINT('Ctrl Pts',(-32.165898167705,31.869832376844,3.28449990511991));
#25655=CARTESIAN_POINT('Ctrl Pts',(-32.8727849788305,32.1988126503382,4.84119670910639));
#25656=CARTESIAN_POINT('Ctrl Pts',(-34.0340172414016,32.9214854985885,5.91846432228298));
#25657=CARTESIAN_POINT('Ctrl Pts',(-35.1952495039727,33.6441583468387,6.99573193545957));
#25658=CARTESIAN_POINT('Ctrl Pts',(-36.6086244696003,34.5853140909923,7.38020429521639));
#25659=CARTESIAN_POINT('Ctrl Pts',(-38.021999435228,35.5264698351459,7.76467665497321));
#25660=CARTESIAN_POINT('Ctrl Pts',(-39.4353744008557,36.4676255792995,7.38020429521639));
#25661=CARTESIAN_POINT('',(-27.7725495286901,25.6404249707042,1.57950157595365E-9));
#25662=CARTESIAN_POINT('Origin',(-14.30703348905,37.5852932322718,0.));
#25663=CARTESIAN_POINT('Ctrl Pts',(-27.7725495288657,25.6404249705938,3.13107855620726E-9));
#25664=CARTESIAN_POINT('Ctrl Pts',(-27.7831439665412,25.6281983378205,0.245038153335483));
#25665=CARTESIAN_POINT('Ctrl Pts',(-27.7986217084843,25.620014287052,0.490791160521711));
#25666=CARTESIAN_POINT('Ctrl Pts',(-27.8190271851149,25.615952633098,0.736766500725353));
#25667=CARTESIAN_POINT('Ctrl Pts',(-27.8393656717117,25.6119043133258,0.981934317701018));
#25668=CARTESIAN_POINT('Ctrl Pts',(-27.8645996505508,25.6119514551674,1.22732257376568));
#25669=CARTESIAN_POINT('Ctrl Pts',(-27.8947338787562,25.6161410294535,1.47243294816347));
#25670=CARTESIAN_POINT('Ctrl Pts',(-27.9248227237927,25.6203242940987,1.7171741780302));
#25671=CARTESIAN_POINT('Ctrl Pts',(-27.9597970874097,25.6286375769735,1.96163791541586));
#25672=CARTESIAN_POINT('Ctrl Pts',(-27.9996219245318,25.6410945477696,2.20532408778522));
#25673=CARTESIAN_POINT('Ctrl Pts',(-28.0394126058352,25.65354083483,2.44880126242065));
#25674=CARTESIAN_POINT('Ctrl Pts',(-28.0840454126419,25.6701237175579,2.69150175431052));
#25675=CARTESIAN_POINT('Ctrl Pts',(-28.1334457426219,25.6908232719759,2.93292951866812));
#25676=CARTESIAN_POINT('Ctrl Pts',(-28.1828357379544,25.7115184960059,3.17430677585587));
#25677=CARTESIAN_POINT('Ctrl Pts',(-28.2369911812593,25.7363286400398,3.41441139318335));
#25678=CARTESIAN_POINT('Ctrl Pts',(-28.2957987052584,25.7652003562646,3.65275710614621));
#25679=CARTESIAN_POINT('Ctrl Pts',(-28.354680902112,25.7941087333334,3.89140546668766));
#25680=CARTESIAN_POINT('Ctrl Pts',(-28.4182268780896,25.8270889373971,4.12829002081136));
#25681=CARTESIAN_POINT('Ctrl Pts',(-28.4862854384143,25.8640546001338,4.36293874377775));
#25682=CARTESIAN_POINT('Ctrl Pts',(-28.5544134456108,25.9010579825875,4.59782690201417));
#25683=CARTESIAN_POINT('Ctrl Pts',(-28.6270630772619,25.9420548501734,4.83047425894929));
#25684=CARTESIAN_POINT('Ctrl Pts',(-28.7040474659736,25.9869270447948,5.06042975959402));
#25685=CARTESIAN_POINT('Ctrl Pts',(-28.781256926861,26.0319304281238,5.29105755998291));
#25686=CARTESIAN_POINT('Ctrl Pts',(-28.862826319325,26.0808316886118,5.51897736305688));
#25687=CARTESIAN_POINT('Ctrl Pts',(-28.9485346007075,26.1334818341725,5.74376259354345));
#25688=CARTESIAN_POINT('Ctrl Pts',(-29.0031847495426,26.1670531325894,5.88709234072629));
#25689=CARTESIAN_POINT('Ctrl Pts',(-29.0595170057057,26.2021480259522,6.02914825314197));
#25690=CARTESIAN_POINT('Ctrl Pts',(-29.1174678338916,26.2387220458402,6.16982677023484));
#25691=CARTESIAN_POINT('Ctrl Pts',(-29.2083364372325,26.2960711849263,6.39041482339091));
#25692=CARTESIAN_POINT('Ctrl Pts',(-29.3038406779898,26.3572486158601,6.60890054011807));
#25693=CARTESIAN_POINT('Ctrl Pts',(-29.4038573838825,26.4221888209395,6.82480412008045));
#25694=CARTESIAN_POINT('Ctrl Pts',(-29.5036482964479,26.4869824198611,7.04022028559295));
#25695=CARTESIAN_POINT('Ctrl Pts',(-29.607931238224,26.5555217851615,7.25306552029639));
#25696=CARTESIAN_POINT('Ctrl Pts',(-29.7165449255438,26.6277100364535,7.46287566269419));
#25697=CARTESIAN_POINT('Ctrl Pts',(-29.8249839175527,26.6997821794601,7.67234834441887));
#25698=CARTESIAN_POINT('Ctrl Pts',(-29.9377396021008,26.7754914030013,7.87879526533038));
#25699=CARTESIAN_POINT('Ctrl Pts',(-30.0546142350032,26.854710408865,8.08177334612208));
#25700=CARTESIAN_POINT('Ctrl Pts',(-30.1713767224895,26.9338534012418,8.28455666214101));
#25701=CARTESIAN_POINT('Ctrl Pts',(-30.2922500787579,27.0164993284346,8.48387739272823));
#25702=CARTESIAN_POINT('Ctrl Pts',(-30.4170022653822,27.1024918458753,8.67931873611042));
#25703=CARTESIAN_POINT('Ctrl Pts',(-30.5417604522567,27.1884884993287,8.87476947970428));
#25704=CARTESIAN_POINT('Ctrl Pts',(-30.6703976233159,27.2778319154178,9.06634009532753));
#25705=CARTESIAN_POINT('Ctrl Pts',(-30.8026498047312,27.3703382785457,9.25364450340897));
#25706=CARTESIAN_POINT('Ctrl Pts',(-30.934950501554,27.46287857672,9.44101762226397));
#25707=CARTESIAN_POINT('Ctrl Pts',(-31.0708686028426,27.5585839591967,9.62412107874923));
#25708=CARTESIAN_POINT('Ctrl Pts',(-31.2101115092129,27.6572454428932,9.80260437466004));
#25709=CARTESIAN_POINT('Ctrl Pts',(-31.3495815496047,27.7560678639054,9.98137881379558));
#25710=CARTESIAN_POINT('Ctrl Pts',(-31.4923869622799,27.8578558275192,10.1555177270912));
#25711=CARTESIAN_POINT('Ctrl Pts',(-31.6382093995766,27.9623772429043,10.3247095747696));
#25712=CARTESIAN_POINT('Ctrl Pts',(-31.6803570199432,27.9925874699277,10.3736117457747));
#25713=CARTESIAN_POINT('Ctrl Pts',(-31.7227565449037,28.0230259217675,10.4221009095753));
#25714=CARTESIAN_POINT('Ctrl Pts',(-31.7653999649278,28.0536866918426,10.4701702229111));
#25715=CARTESIAN_POINT('Ctrl Pts',(-35.8372231206708,26.488126377667,1.04083408558608E-14));
#25716=CARTESIAN_POINT('Ctrl Pts',(-35.977550420802,26.3261800403054,1.72780310113343));
#25717=CARTESIAN_POINT('Ctrl Pts',(-36.6844372319275,26.6551603137996,3.28449990511992));
#25718=CARTESIAN_POINT('Ctrl Pts',(-37.391324043053,26.9841405872938,4.84119670910639));
#25719=CARTESIAN_POINT('Ctrl Pts',(-38.5525563056241,27.7068134355441,5.91846432228298));
#25720=CARTESIAN_POINT('Ctrl Pts',(-39.7137885681951,28.4294862837944,6.99573193545956));
#25721=CARTESIAN_POINT('Ctrl Pts',(-41.1271635338228,29.3706420279479,7.3802042952164));
#25722=CARTESIAN_POINT('Ctrl Pts',(-42.5405384994505,30.3117977721015,7.76467665497322));
#25723=CARTESIAN_POINT('Ctrl Pts',(-43.9539134650781,31.2529535162551,7.38020429521639));
#25724=CARTESIAN_POINT('Ctrl Pts',(-33.5084586029185,26.0399651488662,-1.05434036998093E-14));
#25725=CARTESIAN_POINT('Ctrl Pts',(-33.6487859030496,25.8780188115046,2.19648874705822));
#25726=CARTESIAN_POINT('Ctrl Pts',(-34.5093582297244,26.3401683422826,4.17545672685568));
#25727=CARTESIAN_POINT('Ctrl Pts',(-35.3699305563991,26.8023178730606,6.15442470665313));
#25728=CARTESIAN_POINT('Ctrl Pts',(-36.8080945488849,27.7649534312597,7.5239130403414));
#25729=CARTESIAN_POINT('Ctrl Pts',(-38.2462585413708,28.7275889894589,8.89340137402966));
#25730=CARTESIAN_POINT('Ctrl Pts',(-40.0049617258244,29.9679733385714,9.3821661014496));
#25731=CARTESIAN_POINT('Ctrl Pts',(-41.7636649102779,31.2083576876839,9.87093082886953));
#25732=CARTESIAN_POINT('Ctrl Pts',(-43.5223680947315,32.4487420367965,9.3821661014496));
#25733=CARTESIAN_POINT('Ctrl Pts',(-31.3118750466444,25.1460896841346,0.));
#25734=CARTESIAN_POINT('Ctrl Pts',(-31.4522023467755,24.984143346773,2.7089937269807));
#25735=CARTESIAN_POINT('Ctrl Pts',(-32.4808288751221,25.5919126722343,5.14971273833323));
#25736=CARTESIAN_POINT('Ctrl Pts',(-33.5094554034686,26.1996819976955,7.59043174968577));
#25737=CARTESIAN_POINT('Ctrl Pts',(-35.2504426036075,27.4247153590145,9.27946171175751));
#25738=CARTESIAN_POINT('Ctrl Pts',(-36.9914298037463,28.6497487203334,10.9684916738293));
#25739=CARTESIAN_POINT('Ctrl Pts',(-39.1277473516755,30.2173377779966,11.5712994880388));
#25740=CARTESIAN_POINT('Ctrl Pts',(-41.2640648996046,31.7849268356598,12.1741073022483));
#25741=CARTESIAN_POINT('Ctrl Pts',(-43.4003824475338,33.3525158933231,11.5712994880388));
#25742=CARTESIAN_POINT('Ctrl Pts',(-29.331888309534,23.8408520862201,0.));
#25743=CARTESIAN_POINT('Ctrl Pts',(-29.4722156096651,23.6789057488585,3.24562220582793));
#25744=CARTESIAN_POINT('Ctrl Pts',(-30.6768066147289,24.4391491613476,6.16982677025168));
#25745=CARTESIAN_POINT('Ctrl Pts',(-31.8813976197927,25.1993925738367,9.09403133467541));
#25746=CARTESIAN_POINT('Ctrl Pts',(-33.9394618506895,26.6991747463035,11.1176436806954));
#25747=CARTESIAN_POINT('Ctrl Pts',(-35.9975260815862,28.1989569187703,13.1412560267153));
#25748=CARTESIAN_POINT('Ctrl Pts',(-38.5292322196779,30.1091521400805,13.8634749112255));
#25749=CARTESIAN_POINT('Ctrl Pts',(-41.0609383577695,32.0193473613908,14.5856937957357));
#25750=CARTESIAN_POINT('Ctrl Pts',(-43.5926444958611,33.929542582701,13.8634749112255));
#25751=CARTESIAN_POINT('',(-29.331888309534,23.8408520862201,0.));
#25752=CARTESIAN_POINT('Ctrl Pts',(-29.331888309534,23.8408520862201,0.));
#25753=CARTESIAN_POINT('Ctrl Pts',(-29.4722156096651,23.6789057488585,3.24562220582793));
#25754=CARTESIAN_POINT('Ctrl Pts',(-30.6768066147289,24.4391491613476,6.16982677025168));
#25755=CARTESIAN_POINT('Ctrl Pts',(-31.6824449968207,25.0738292744462,8.61106394926976));
#25756=CARTESIAN_POINT('Ctrl Pts',(-33.305918063411,26.2405847244739,10.4489096280657));
#25757=CARTESIAN_POINT('Origin',(-39.2388322978494,8.81246358936587,0.));
#25758=CARTESIAN_POINT('Ctrl Pts',(-29.331888309534,23.8408520862201,0.));
#25759=CARTESIAN_POINT('Ctrl Pts',(-29.4722156096651,23.6789057488585,3.24562220582793));
#25760=CARTESIAN_POINT('Ctrl Pts',(-30.6768066147289,24.4391491613476,6.16982677025168));
#25761=CARTESIAN_POINT('Ctrl Pts',(-31.8813976197927,25.1993925738367,9.09403133467541));
#25762=CARTESIAN_POINT('Ctrl Pts',(-33.9394618506895,26.6991747463035,11.1176436806954));
#25763=CARTESIAN_POINT('Ctrl Pts',(-35.9975260815862,28.1989569187703,13.1412560267153));
#25764=CARTESIAN_POINT('Ctrl Pts',(-38.5292322196779,30.1091521400805,13.8634749112255));
#25765=CARTESIAN_POINT('Ctrl Pts',(-41.0609383577695,32.0193473613908,14.5856937957357));
#25766=CARTESIAN_POINT('Ctrl Pts',(-43.5926444958611,33.929542582701,13.8634749112255));
#25767=CARTESIAN_POINT('Ctrl Pts',(-28.3879644434327,23.9681616891744,0.));
#25768=CARTESIAN_POINT('Ctrl Pts',(-28.5282917435638,23.8062153518127,3.38941559469371));
#25769=CARTESIAN_POINT('Ctrl Pts',(-29.7800336722639,24.6073152722066,6.44317352589573));
#25770=CARTESIAN_POINT('Ctrl Pts',(-31.0317756009639,25.4084151926005,9.49693145709774));
#25771=CARTESIAN_POINT('Ctrl Pts',(-33.1748028604389,26.9818182484141,11.6101975146502));
#25772=CARTESIAN_POINT('Ctrl Pts',(-35.3178301199139,28.5552213042277,13.7234635722027));
#25773=CARTESIAN_POINT('Ctrl Pts',(-37.9554834217126,30.5572202654791,14.4776794959001));
#25774=CARTESIAN_POINT('Ctrl Pts',(-40.5931367235113,32.5592192267305,15.2318954195974));
#25775=CARTESIAN_POINT('Ctrl Pts',(-43.23079002531,34.5612181879819,14.4776794959001));
#25776=CARTESIAN_POINT('Ctrl Pts',(-27.7642289310885,24.6879908429607,6.24500451351651E-15));
#25777=CARTESIAN_POINT('Ctrl Pts',(-27.9045562312196,24.5260445055991,3.38941559469371));
#25778=CARTESIAN_POINT('Ctrl Pts',(-29.1562981599197,25.3271444259929,6.44317352589573));
#25779=CARTESIAN_POINT('Ctrl Pts',(-30.4080400886198,26.1282443463868,9.49693145709773));
#25780=CARTESIAN_POINT('Ctrl Pts',(-32.5510673480947,27.7016474022004,11.6101975146502));
#25781=CARTESIAN_POINT('Ctrl Pts',(-34.6940946075697,29.275050458014,13.7234635722027));
#25782=CARTESIAN_POINT('Ctrl Pts',(-37.3317479093684,31.2770494192654,14.4776794959001));
#25783=CARTESIAN_POINT('Ctrl Pts',(-39.9694012111672,33.2790483805169,15.2318954195974));
#25784=CARTESIAN_POINT('Ctrl Pts',(-42.6070545129659,35.2810473417683,14.4776794959001));
#25785=CARTESIAN_POINT('Ctrl Pts',(-27.7725495286736,25.640424970686,0.));
#25786=CARTESIAN_POINT('Ctrl Pts',(-27.9128768288047,25.4784786333244,3.24562220582793));
#25787=CARTESIAN_POINT('Ctrl Pts',(-29.1174678338685,26.2387220458134,6.16982677025167));
#25788=CARTESIAN_POINT('Ctrl Pts',(-30.3220588389323,26.9989654583025,9.09403133467541));
#25789=CARTESIAN_POINT('Ctrl Pts',(-32.3801230698291,28.4987476307693,11.1176436806954));
#25790=CARTESIAN_POINT('Ctrl Pts',(-34.4381873007258,29.9985298032361,13.1412560267153));
#25791=CARTESIAN_POINT('Ctrl Pts',(-36.9698934388174,31.9087250245464,13.8634749112255));
#25792=CARTESIAN_POINT('Ctrl Pts',(-39.501599576909,33.8189202458566,14.5856937957357));
#25793=CARTESIAN_POINT('Ctrl Pts',(-42.0333057150006,35.7291154671669,13.8634749112255));
#25794=CARTESIAN_POINT('',(-28.2121283533394,24.4459549573185,-1.89568229885776E-29));
#25795=CARTESIAN_POINT('Origin',(-29.572480844482,25.6247005192792,0.));
#25796=CARTESIAN_POINT('Origin',(-29.572480844482,25.6247005192792,0.));
#25797=CARTESIAN_POINT('Ctrl Pts',(-23.8408520862198,29.3318883095343,0.));
#25798=CARTESIAN_POINT('Ctrl Pts',(-24.0027984235814,29.1915610094031,3.24562220582793));
#25799=CARTESIAN_POINT('Ctrl Pts',(-25.0869345107938,30.1154974142047,6.16982677025168));
#25800=CARTESIAN_POINT('Ctrl Pts',(-26.1710705980061,31.0394338190062,9.09403133467542));
#25801=CARTESIAN_POINT('Ctrl Pts',(-27.9947454451961,32.8168434496407,11.1176436806954));
#25802=CARTESIAN_POINT('Ctrl Pts',(-29.8184202923862,34.5942530802753,13.1412560267153));
#25803=CARTESIAN_POINT('Ctrl Pts',(-32.0525081884196,36.8453046181046,13.8634749112255));
#25804=CARTESIAN_POINT('Ctrl Pts',(-34.2865960844531,39.096356155934,14.5856937957357));
#25805=CARTESIAN_POINT('Ctrl Pts',(-36.5206839804866,41.3474076937634,13.8634749112255));
#25806=CARTESIAN_POINT('Ctrl Pts',(-25.1460896841343,31.3118750466447,0.));
#25807=CARTESIAN_POINT('Ctrl Pts',(-25.3080360214959,31.1715477465136,2.70899372698069));
#25808=CARTESIAN_POINT('Ctrl Pts',(-26.2396980216804,31.9195196745979,5.14971273833323));
#25809=CARTESIAN_POINT('Ctrl Pts',(-27.1713600218649,32.6674916026822,7.59043174968577));
#25810=CARTESIAN_POINT('Ctrl Pts',(-28.7202860579071,34.1278242025587,9.27946171175752));
#25811=CARTESIAN_POINT('Ctrl Pts',(-30.2692120939493,35.5881568024353,10.9684916738293));
#25812=CARTESIAN_POINT('Ctrl Pts',(-32.1606938263357,37.4438197501022,11.5712994880388));
#25813=CARTESIAN_POINT('Ctrl Pts',(-34.0521755587222,39.2994826977691,12.1741073022483));
#25814=CARTESIAN_POINT('Ctrl Pts',(-35.9436572911087,41.1551456454361,11.5712994880388));
#25815=CARTESIAN_POINT('Ctrl Pts',(-26.0399651488659,33.5084586029188,0.));
#25816=CARTESIAN_POINT('Ctrl Pts',(-26.2019114862275,33.3681313027876,2.19648874705823));
#25817=CARTESIAN_POINT('Ctrl Pts',(-26.9879536917288,33.9480490292001,4.17545672685568));
#25818=CARTESIAN_POINT('Ctrl Pts',(-27.7739958972301,34.5279667556126,6.15442470665314));
#25819=CARTESIAN_POINT('Ctrl Pts',(-29.0605241301524,35.6854761478362,7.5239130403414));
#25820=CARTESIAN_POINT('Ctrl Pts',(-30.3470523630747,36.8429855400598,8.89340137402968));
#25821=CARTESIAN_POINT('Ctrl Pts',(-31.9113293869105,38.3210341242511,9.38216610144961));
#25822=CARTESIAN_POINT('Ctrl Pts',(-33.4756064107463,39.7990827084424,9.87093082886954));
#25823=CARTESIAN_POINT('Ctrl Pts',(-35.039883434582,41.2771312926338,9.38216610144961));
#25824=CARTESIAN_POINT('Ctrl Pts',(-26.4881263776667,35.8372231206711,0.));
#25825=CARTESIAN_POINT('Ctrl Pts',(-26.6500727150283,35.69689582054,1.72780310113343));
#25826=CARTESIAN_POINT('Ctrl Pts',(-27.3029456632458,36.1231280314033,3.28449990511992));
#25827=CARTESIAN_POINT('Ctrl Pts',(-27.9558186114632,36.5493602422666,4.84119670910639));
#25828=CARTESIAN_POINT('Ctrl Pts',(-29.0023841344367,37.4299379045754,5.91846432228298));
#25829=CARTESIAN_POINT('Ctrl Pts',(-30.0489496574102,38.3105155668841,6.99573193545957));
#25830=CARTESIAN_POINT('Ctrl Pts',(-31.313998076287,39.4432359322496,7.3802042952164));
#25831=CARTESIAN_POINT('Ctrl Pts',(-32.5790464951638,40.575956297615,7.76467665497322));
#25832=CARTESIAN_POINT('Ctrl Pts',(-33.8440949140406,41.7086766629804,7.38020429521639));
#25833=CARTESIAN_POINT('',(-23.8408520862339,29.3318883095431,1.5794998097385E-9));
#25834=CARTESIAN_POINT('Origin',(-8.81246358936545,39.2388322978495,0.));
#25835=CARTESIAN_POINT('Ctrl Pts',(-23.8408520864231,29.3318883094703,3.1310741434434E-9));
#25836=CARTESIAN_POINT('Ctrl Pts',(-23.8530787192647,29.3212938718737,0.24503815333526));
#25837=CARTESIAN_POINT('Ctrl Pts',(-23.8695636319734,29.3153958352831,0.490791160521269));
#25838=CARTESIAN_POINT('Ctrl Pts',(-23.8903394438997,29.3142795252165,0.736766500724692));
#25839=CARTESIAN_POINT('Ctrl Pts',(-23.9110470500023,29.3131668799331,0.981934317700348));
#25840=CARTESIAN_POINT('Ctrl Pts',(-23.9360174743377,29.3168047115562,1.22732257376501));
#25841=CARTESIAN_POINT('Ctrl Pts',(-23.965248740963,29.3252401898305,1.47243294816278));
#25842=CARTESIAN_POINT('Ctrl Pts',(-23.99443598431,29.3336629639885,1.71717417802956));
#25843=CARTESIAN_POINT('Ctrl Pts',(-24.0278712558265,29.3468690005323,1.96163791541528));
#25844=CARTESIAN_POINT('Ctrl Pts',(-24.0655179217451,29.3648668425815,2.20532408778468));
#25845=CARTESIAN_POINT('Ctrl Pts',(-24.1031322999561,29.3828492487602,2.44880126242007));
#25846=CARTESIAN_POINT('Ctrl Pts',(-24.1449508188712,29.4056152523348,2.69150175430988));
#25847=CARTESIAN_POINT('Ctrl Pts',(-24.190902470982,29.4331345151068,2.93292951866742));
#25848=CARTESIAN_POINT('Ctrl Pts',(-24.2368445099157,29.4606480207943,3.17430677585524));
#25849=CARTESIAN_POINT('Ctrl Pts',(-24.2869178772577,29.4929127564908,3.41441139318279));
#25850=CARTESIAN_POINT('Ctrl Pts',(-24.3410179518308,29.5298597835412,3.65275710614572));
#25851=CARTESIAN_POINT('Ctrl Pts',(-24.3951867218143,29.5668537253362,3.89140546668722));
#25852=CARTESIAN_POINT('Ctrl Pts',(-24.4533923189746,29.6085417737703,4.12829002081097));
#25853=CARTESIAN_POINT('Ctrl Pts',(-24.5154973789735,29.6548169223661,4.3629387437774));
#25854=CARTESIAN_POINT('Ctrl Pts',(-24.5776658108998,29.7011392900669,4.59782690201371));
#25855=CARTESIAN_POINT('Ctrl Pts',(-24.6437415114725,29.7520579892324,4.83047425894872));
#25856=CARTESIAN_POINT('Ctrl Pts',(-24.7135563309889,29.8074294704419,5.06042975959335));
#25857=CARTESIAN_POINT('Ctrl Pts',(-24.783575261671,29.8629628361575,5.29105755998213));
#25858=CARTESIAN_POINT('Ctrl Pts',(-24.8573550203554,29.92297488722,5.51897736305601));
#25859=CARTESIAN_POINT('Ctrl Pts',(-24.9346980180639,29.9872866904179,5.7437625935425));
#25860=CARTESIAN_POINT('Ctrl Pts',(-24.9840142132781,30.0282938085158,5.88709234072565));
#25861=CARTESIAN_POINT('Ctrl Pts',(-25.0347785642249,30.0710484023923,6.02914825314166));
#25862=CARTESIAN_POINT('Ctrl Pts',(-25.0869345108128,30.1154974142344,6.16982677023484));
#25863=CARTESIAN_POINT('Ctrl Pts',(-25.1687165693393,30.1851947723639,6.39041482339095));
#25864=CARTESIAN_POINT('Ctrl Pts',(-25.2545422584421,30.2593411758391,6.60890054011814));
#25865=CARTESIAN_POINT('Ctrl Pts',(-25.3442989836977,30.3378542445906,6.82480412008054));
#25866=CARTESIAN_POINT('Ctrl Pts',(-25.4338530781081,30.4161900656827,7.040220285593));
#25867=CARTESIAN_POINT('Ctrl Pts',(-25.5273204012124,30.4988728090635,7.2530655202964));
#25868=CARTESIAN_POINT('Ctrl Pts',(-25.6245550984954,30.5857836273893,7.46287566269415));
#25869=CARTESIAN_POINT('Ctrl Pts',(-25.7216334025458,30.6725546575099,7.6723483444188));
#25870=CARTESIAN_POINT('Ctrl Pts',(-25.8224668509014,30.76354007733,7.87879526533026));
#25871=CARTESIAN_POINT('Ctrl Pts',(-25.9268778285525,30.8585857424181,8.08177334612193));
#25872=CARTESIAN_POINT('Ctrl Pts',(-26.0311886201134,30.9535402077704,8.2845566621412));
#25873=CARTESIAN_POINT('Ctrl Pts',(-26.1390699181377,31.052546990739,8.48387739272874));
#25874=CARTESIAN_POINT('Ctrl Pts',(-26.2503142961679,31.155418315607,8.67931873611125));
#25875=CARTESIAN_POINT('Ctrl Pts',(-26.3615640247582,31.2582945883135,8.8747694797051));
#25876=CARTESIAN_POINT('Ctrl Pts',(-26.476176961084,31.3650355954446,9.06634009532834));
#25877=CARTESIAN_POINT('Ctrl Pts',(-26.5939179778766,31.4754218249885,9.25364450340976));
#25878=CARTESIAN_POINT('Ctrl Pts',(-26.7117021867993,31.5858485486313,9.44101762226492));
#25879=CARTESIAN_POINT('Ctrl Pts',(-26.8326165417655,31.6999229509135,9.62412107875032));
#25880=CARTESIAN_POINT('Ctrl Pts',(-26.9564011630247,31.8173965346651,9.80260437466126));
#25881=CARTESIAN_POINT('Ctrl Pts',(-27.0803877026406,31.935061742164,9.98137881379697));
#25882=CARTESIAN_POINT('Ctrl Pts',(-27.2072536245434,32.0561369802839,10.1555177270928));
#25883=CARTESIAN_POINT('Ctrl Pts',(-27.3367168513606,32.1803472149485,10.3247095747713));
#25884=CARTESIAN_POINT('Ctrl Pts',(-27.3741361061489,32.2162481771947,10.3736117457742));
#25885=CARTESIAN_POINT('Ctrl Pts',(-27.4117722217278,32.2524108910194,10.4221009095725));
#25886=CARTESIAN_POINT('Ctrl Pts',(-27.4496181106865,32.2888283700868,10.4701702229062));
#25887=CARTESIAN_POINT('Ctrl Pts',(-31.7027984407111,31.3186840564487,0.));
#25888=CARTESIAN_POINT('Ctrl Pts',(-31.8647447780727,31.1783567563176,1.72780310113342));
#25889=CARTESIAN_POINT('Ctrl Pts',(-32.5176177262902,31.6045889671808,3.28449990511991));
#25890=CARTESIAN_POINT('Ctrl Pts',(-33.1704906745076,32.0308211780441,4.84119670910638));
#25891=CARTESIAN_POINT('Ctrl Pts',(-34.2170561974811,32.9113988403529,5.91846432228298));
#25892=CARTESIAN_POINT('Ctrl Pts',(-35.2636217204547,33.7919765026617,6.99573193545956));
#25893=CARTESIAN_POINT('Ctrl Pts',(-36.5286701393314,34.9246968680271,7.38020429521639));
#25894=CARTESIAN_POINT('Ctrl Pts',(-37.7937185582083,36.0574172333925,7.76467665497321));
#25895=CARTESIAN_POINT('Ctrl Pts',(-39.0587669770851,37.1901375987579,7.38020429521639));
#25896=CARTESIAN_POINT('Ctrl Pts',(-29.4615173807454,30.5436667170414,0.));
#25897=CARTESIAN_POINT('Ctrl Pts',(-29.6234637181071,30.4033394169103,2.19648874705824));
#25898=CARTESIAN_POINT('Ctrl Pts',(-30.4095059236083,30.9832571433228,4.17545672685567));
#25899=CARTESIAN_POINT('Ctrl Pts',(-31.1955481291096,31.5631748697353,6.15442470665313));
#25900=CARTESIAN_POINT('Ctrl Pts',(-32.4820763620319,32.7206842619589,7.5239130403414));
#25901=CARTESIAN_POINT('Ctrl Pts',(-33.7686045949543,33.8781936541824,8.89340137402967));
#25902=CARTESIAN_POINT('Ctrl Pts',(-35.3328816187901,35.3562422383738,9.3821661014496));
#25903=CARTESIAN_POINT('Ctrl Pts',(-36.8971586426258,36.8342908225651,9.87093082886954));
#25904=CARTESIAN_POINT('Ctrl Pts',(-38.4614356664616,38.3123394067564,9.3821661014496));
#25905=CARTESIAN_POINT('Ctrl Pts',(-27.414503620062,29.3462831821139,0.));
#25906=CARTESIAN_POINT('Ctrl Pts',(-27.5764499574236,29.2059558819828,2.70899372698069));
#25907=CARTESIAN_POINT('Ctrl Pts',(-28.5081119576081,29.9539278100671,5.14971273833323));
#25908=CARTESIAN_POINT('Ctrl Pts',(-29.4397739577926,30.7018997381514,7.59043174968578));
#25909=CARTESIAN_POINT('Ctrl Pts',(-30.9886999938348,32.162232338028,9.27946171175752));
#25910=CARTESIAN_POINT('Ctrl Pts',(-32.537626029877,33.6225649379046,10.9684916738293));
#25911=CARTESIAN_POINT('Ctrl Pts',(-34.4291077622634,35.4782278855715,11.5712994880388));
#25912=CARTESIAN_POINT('Ctrl Pts',(-36.3205894946499,37.3338908332384,12.1741073022483));
#25913=CARTESIAN_POINT('Ctrl Pts',(-38.2120712270364,39.1895537809053,11.5712994880388));
#25914=CARTESIAN_POINT('Ctrl Pts',(-25.6404249706857,27.7725495286739,1.04083408558608E-14));
#25915=CARTESIAN_POINT('Ctrl Pts',(-25.8023713080473,27.6322222285427,3.24562220582793));
#25916=CARTESIAN_POINT('Ctrl Pts',(-26.8865073952596,28.5561586333443,6.16982677025167));
#25917=CARTESIAN_POINT('Ctrl Pts',(-27.970643482472,29.4800950381458,9.09403133467541));
#25918=CARTESIAN_POINT('Ctrl Pts',(-29.794318329662,31.2575046687803,11.1176436806954));
#25919=CARTESIAN_POINT('Ctrl Pts',(-31.617993176852,33.0349142994148,13.1412560267153));
#25920=CARTESIAN_POINT('Ctrl Pts',(-33.8520810728855,35.2859658372442,13.8634749112255));
#25921=CARTESIAN_POINT('Ctrl Pts',(-36.086168968919,37.5370173750736,14.5856937957357));
#25922=CARTESIAN_POINT('Ctrl Pts',(-38.3202568649525,39.7880689129029,13.8634749112255));
#25923=CARTESIAN_POINT('',(-25.6404249706857,27.7725495286739,1.04083408558608E-14));
#25924=CARTESIAN_POINT('Ctrl Pts',(-25.6404249706857,27.7725495286739,1.04083408558608E-14));
#25925=CARTESIAN_POINT('Ctrl Pts',(-25.8023713080473,27.6322222285427,3.24562220582793));
#25926=CARTESIAN_POINT('Ctrl Pts',(-26.8865073952596,28.5561586333443,6.16982677025167));
#25927=CARTESIAN_POINT('Ctrl Pts',(-27.7915854309816,29.3274958817335,8.61106394926976));
#25928=CARTESIAN_POINT('Ctrl Pts',(-29.2324872694337,30.7134197505152,10.4489096280657));
#25929=CARTESIAN_POINT('Origin',(-37.5852932322716,14.3070334890504,0.));
#25930=CARTESIAN_POINT('Ctrl Pts',(-25.6404249706857,27.7725495286739,1.04083408558608E-14));
#25931=CARTESIAN_POINT('Ctrl Pts',(-25.8023713080473,27.6322222285427,3.24562220582793));
#25932=CARTESIAN_POINT('Ctrl Pts',(-26.8865073952596,28.5561586333443,6.16982677025167));
#25933=CARTESIAN_POINT('Ctrl Pts',(-27.970643482472,29.4800950381458,9.09403133467541));
#25934=CARTESIAN_POINT('Ctrl Pts',(-29.794318329662,31.2575046687803,11.1176436806954));
#25935=CARTESIAN_POINT('Ctrl Pts',(-31.617993176852,33.0349142994148,13.1412560267153));
#25936=CARTESIAN_POINT('Ctrl Pts',(-33.8520810728855,35.2859658372442,13.8634749112255));
#25937=CARTESIAN_POINT('Ctrl Pts',(-36.086168968919,37.5370173750736,14.5856937957357));
#25938=CARTESIAN_POINT('Ctrl Pts',(-38.3202568649525,39.7880689129029,13.8634749112255));
#25939=CARTESIAN_POINT('Ctrl Pts',(-24.6879908429604,27.7642289310888,0.));
#25940=CARTESIAN_POINT('Ctrl Pts',(-24.849937180322,27.6239016309577,3.38941559469372));
#25941=CARTESIAN_POINT('Ctrl Pts',(-25.9749297754391,28.5949889593955,6.44317352589574));
#25942=CARTESIAN_POINT('Ctrl Pts',(-27.0999223705562,29.5660762878332,9.49693145709774));
#25943=CARTESIAN_POINT('Ctrl Pts',(-28.9972181010931,31.428448947046,11.6101975146502));
#25944=CARTESIAN_POINT('Ctrl Pts',(-30.89451383163,33.2908216062587,13.7234635722027));
#25945=CARTESIAN_POINT('Ctrl Pts',(-33.2204054676046,35.6478203077952,14.4776794959001));
#25946=CARTESIAN_POINT('Ctrl Pts',(-35.5462971035792,38.0048190093317,15.2318954195974));
#25947=CARTESIAN_POINT('Ctrl Pts',(-37.8721887395538,40.3618177108681,14.4776794959001));
#25948=CARTESIAN_POINT('Ctrl Pts',(-23.9681616891741,28.3879644434329,0.));
#25949=CARTESIAN_POINT('Ctrl Pts',(-24.1301080265357,28.2476371433018,3.38941559469372));
#25950=CARTESIAN_POINT('Ctrl Pts',(-25.2551006216528,29.2187244717396,6.44317352589574));
#25951=CARTESIAN_POINT('Ctrl Pts',(-26.3800932167699,30.1898118001774,9.49693145709774));
#25952=CARTESIAN_POINT('Ctrl Pts',(-28.2773889473068,32.0521844593901,11.6101975146502));
#25953=CARTESIAN_POINT('Ctrl Pts',(-30.1746846778436,33.9145571186029,13.7234635722027));
#25954=CARTESIAN_POINT('Ctrl Pts',(-32.5005763138183,36.2715558201394,14.4776794959001));
#25955=CARTESIAN_POINT('Ctrl Pts',(-34.8264679497929,38.6285545216759,15.2318954195974));
#25956=CARTESIAN_POINT('Ctrl Pts',(-37.1523595857675,40.9855532232123,14.4776794959001));
#25957=CARTESIAN_POINT('Ctrl Pts',(-23.8408520862198,29.3318883095343,0.));
#25958=CARTESIAN_POINT('Ctrl Pts',(-24.0027984235814,29.1915610094031,3.24562220582793));
#25959=CARTESIAN_POINT('Ctrl Pts',(-25.0869345107938,30.1154974142047,6.16982677025168));
#25960=CARTESIAN_POINT('Ctrl Pts',(-26.1710705980061,31.0394338190062,9.09403133467541));
#25961=CARTESIAN_POINT('Ctrl Pts',(-27.9947454451961,32.8168434496407,11.1176436806954));
#25962=CARTESIAN_POINT('Ctrl Pts',(-29.8184202923862,34.5942530802752,13.1412560267153));
#25963=CARTESIAN_POINT('Ctrl Pts',(-32.0525081884196,36.8453046181046,13.8634749112255));
#25964=CARTESIAN_POINT('Ctrl Pts',(-34.2865960844531,39.096356155934,14.5856937957357));
#25965=CARTESIAN_POINT('Ctrl Pts',(-36.5206839804866,41.3474076937634,13.8634749112255));
#25966=CARTESIAN_POINT('',(-24.4459474390652,28.212134867943,-1.91000875816707E-29));
#25967=CARTESIAN_POINT('Origin',(-25.6247005192789,29.5724808444823,0.));
#25968=CARTESIAN_POINT('Origin',(-25.6247005192789,29.5724808444823,0.));
#25969=CARTESIAN_POINT('Ctrl Pts',(-19.4238236466307,32.4262389885814,0.));
#25970=CARTESIAN_POINT('Ctrl Pts',(-19.6040922608088,32.3103873848409,3.24562220582793));
#25971=CARTESIAN_POINT('Ctrl Pts',(-20.5457035458243,33.3792081011657,6.16982677025167));
#25972=CARTESIAN_POINT('Ctrl Pts',(-21.4873148308399,34.4480288174905,9.09403133467541));
#25973=CARTESIAN_POINT('Ctrl Pts',(-23.0394755334784,36.4668829718391,11.1176436806954));
#25974=CARTESIAN_POINT('Ctrl Pts',(-24.5916362361169,38.4857371261877,13.1412560267153));
#25975=CARTESIAN_POINT('Ctrl Pts',(-26.4826263031064,41.0318200627226,13.8634749112255));
#25976=CARTESIAN_POINT('Ctrl Pts',(-28.373616370096,43.5779029992574,14.5856937957357));
#25977=CARTESIAN_POINT('Ctrl Pts',(-30.2646064370856,46.1239859357923,13.8634749112255));
#25978=CARTESIAN_POINT('Ctrl Pts',(-20.4339943155205,34.5718269932685,0.));
#25979=CARTESIAN_POINT('Ctrl Pts',(-20.6142629296986,34.4559753895281,2.70899372698069));
#25980=CARTESIAN_POINT('Ctrl Pts',(-21.4299944500886,35.3289233687526,5.14971273833323));
#25981=CARTESIAN_POINT('Ctrl Pts',(-22.2457259704786,36.201871347977,7.59043174968577));
#25982=CARTESIAN_POINT('Ctrl Pts',(-23.5710591750642,37.8677750259292,9.27946171175751));
#25983=CARTESIAN_POINT('Ctrl Pts',(-24.8963923796497,39.5336787038814,10.9684916738292));
#25984=CARTESIAN_POINT('Ctrl Pts',(-26.504533183005,41.6396395952276,11.5712994880388));
#25985=CARTESIAN_POINT('Ctrl Pts',(-28.1126739863603,43.7456004865737,12.1741073022483));
#25986=CARTESIAN_POINT('Ctrl Pts',(-29.7208147897155,45.8515613779198,11.5712994880388));
#25987=CARTESIAN_POINT('Ctrl Pts',(-21.0061649833182,36.8732642383514,0.));
#25988=CARTESIAN_POINT('Ctrl Pts',(-21.1864335974963,36.7574126346109,2.19648874705823));
#25989=CARTESIAN_POINT('Ctrl Pts',(-21.8819441292786,37.4432931040927,4.17545672685567));
#25990=CARTESIAN_POINT('Ctrl Pts',(-22.577454661061,38.1291735735745,6.15442470665313));
#25991=CARTESIAN_POINT('Ctrl Pts',(-23.6861571296386,39.4579932465784,7.5239130403414));
#25992=CARTESIAN_POINT('Ctrl Pts',(-24.7948595982162,40.7868129195822,8.89340137402966));
#25993=CARTESIAN_POINT('Ctrl Pts',(-26.1328662922313,42.4724369320184,9.3821661014496));
#25994=CARTESIAN_POINT('Ctrl Pts',(-27.4708729862464,44.1580609444545,9.87093082886953));
#25995=CARTESIAN_POINT('Ctrl Pts',(-28.8088796802615,45.8436849568906,9.3821661014496));
#25996=CARTESIAN_POINT('Ctrl Pts',(-21.1183468312844,39.2421052839113,0.));
#25997=CARTESIAN_POINT('Ctrl Pts',(-21.2986154454625,39.1262536801709,1.72780310113342));
#25998=CARTESIAN_POINT('Ctrl Pts',(-21.8841839202763,39.6410609697422,3.28449990511991));
#25999=CARTESIAN_POINT('Ctrl Pts',(-22.4697523950901,40.1558682593136,4.84119670910639));
#26000=CARTESIAN_POINT('Ctrl Pts',(-23.3803461224641,41.1764247138526,5.91846432228298));
#26001=CARTESIAN_POINT('Ctrl Pts',(-24.2909398498381,42.1969811683916,6.99573193545957));
#26002=CARTESIAN_POINT('Ctrl Pts',(-25.381908984254,43.4982072348258,7.3802042952164));
#26003=CARTESIAN_POINT('Ctrl Pts',(-26.4728781186701,44.7994333012601,7.76467665497322));
#26004=CARTESIAN_POINT('Ctrl Pts',(-27.563847253086,46.1006593676943,7.3802042952164));
#26005=CARTESIAN_POINT('',(-19.4238236466434,32.4262389885921,1.57949801804089E-9));
#26006=CARTESIAN_POINT('Origin',(-3.13849734404791,40.0935818932913,0.));
#26007=CARTESIAN_POINT('Ctrl Pts',(-19.423823646841,32.426238988547,3.13107091193051E-9));
#26008=CARTESIAN_POINT('Ctrl Pts',(-19.4374335758628,32.4174924183247,0.24503815333528));
#26009=CARTESIAN_POINT('Ctrl Pts',(-19.4545900740529,32.4140004629284,0.490791160521312));
#26010=CARTESIAN_POINT('Ctrl Pts',(-19.4753132856567,32.415852221603,0.736766500724757));
#26011=CARTESIAN_POINT('Ctrl Pts',(-19.4959684641206,32.4176979010578,0.981934317700416));
#26012=CARTESIAN_POINT('Ctrl Pts',(-19.5201670081215,32.4248523667012,1.22732257376508));
#26013=CARTESIAN_POINT('Ctrl Pts',(-19.5479002488742,32.4373620269519,1.47243294816285));
#26014=CARTESIAN_POINT('Ctrl Pts',(-19.5755917224264,32.4498528472302,1.71717417802963));
#26015=CARTESIAN_POINT('Ctrl Pts',(-19.6068072561335,32.467682800622,1.96163791541534));
#26016=CARTESIAN_POINT('Ctrl Pts',(-19.6415093732946,32.4908551297616,2.20532408778474));
#26017=CARTESIAN_POINT('Ctrl Pts',(-19.6761817281438,32.5140075851257,2.44880126242014));
#26018=CARTESIAN_POINT('Ctrl Pts',(-19.7143346547168,32.542493259366,2.69150175430997));
#26019=CARTESIAN_POINT('Ctrl Pts',(-19.7559021858352,32.5762720176612,2.93292951866755));
#26020=CARTESIAN_POINT('Ctrl Pts',(-19.7974610209432,32.6100437093727,3.17430677585542));
#26021=CARTESIAN_POINT('Ctrl Pts',(-19.842432962963,32.6491062197568,3.41441139318301));
#26022=CARTESIAN_POINT('Ctrl Pts',(-19.8907242666034,32.6933764227085,3.65275710614599));
#26023=CARTESIAN_POINT('Ctrl Pts',(-19.9390768897698,32.7377028392566,3.89140546668751));
#26024=CARTESIAN_POINT('Ctrl Pts',(-19.9907572100057,32.7872500836133,4.12829002081127));
#26025=CARTESIAN_POINT('Ctrl Pts',(-20.0456444897535,32.8418926894894,4.36293874377772));
#26026=CARTESIAN_POINT('Ctrl Pts',(-20.1005877764144,32.8965910526137,4.59782690201416));
#26027=CARTESIAN_POINT('Ctrl Pts',(-20.1587444351919,32.9563950254812,4.83047425894931));
#26028=CARTESIAN_POINT('Ctrl Pts',(-20.219968457117,33.0211385895997,5.06042975959406));
#26029=CARTESIAN_POINT('Ctrl Pts',(-20.2813714740831,33.0860714385209,5.29105755998281));
#26030=CARTESIAN_POINT('Ctrl Pts',(-20.3458596558643,33.1559726078588,5.51897736305664));
#26031=CARTESIAN_POINT('Ctrl Pts',(-20.4132628895043,33.2306368658405,5.74376259354308));
#26032=CARTESIAN_POINT('Ctrl Pts',(-20.4562411955792,33.2782450169497,5.88709234072604));
#26033=CARTESIAN_POINT('Ctrl Pts',(-20.5004042255164,33.3277889511026,6.02914825314185));
#26034=CARTESIAN_POINT('Ctrl Pts',(-20.5457035458389,33.3792081011979,6.16982677023484));
#26035=CARTESIAN_POINT('Ctrl Pts',(-20.6167342126794,33.4598348411497,6.39041482339097));
#26036=CARTESIAN_POINT('Ctrl Pts',(-20.6911341865984,33.5454408102122,6.60890054011819));
#26037=CARTESIAN_POINT('Ctrl Pts',(-20.7688037431277,33.635928442969,6.82480412008062));
#26038=CARTESIAN_POINT('Ctrl Pts',(-20.8462979562736,33.7262117948161,7.04022028559307));
#26039=CARTESIAN_POINT('Ctrl Pts',(-20.9270469355453,33.8213547340593,7.25306552029646));
#26040=CARTESIAN_POINT('Ctrl Pts',(-21.0109232247565,33.921218865788,7.46287566269421));
#26041=CARTESIAN_POINT('Ctrl Pts',(-21.0946646065287,34.0209223750762,7.67234834441885));
#26042=CARTESIAN_POINT('Ctrl Pts',(-21.1815231404629,34.1253317904079,7.87879526533032));
#26043=CARTESIAN_POINT('Ctrl Pts',(-21.2713449564541,34.2342692590683,8.08177334612198));
#26044=CARTESIAN_POINT('Ctrl Pts',(-21.3610805851806,34.3431021983075,8.28455666214104));
#26045=CARTESIAN_POINT('Ctrl Pts',(-21.4537736728368,34.4564543444623,8.48387739272837));
#26046=CARTESIAN_POINT('Ctrl Pts',(-21.5492456275381,34.5741103132394,8.67931873611069));
#26047=CARTESIAN_POINT('Ctrl Pts',(-21.6447221741878,34.6917719409573,8.87476947970451));
#26048=CARTESIAN_POINT('Ctrl Pts',(-21.742977686913,34.8137376000409,9.06634009532771));
#26049=CARTESIAN_POINT('Ctrl Pts',(-21.843810671518,34.9397565506947,9.25364450340911));
#26050=CARTESIAN_POINT('Ctrl Pts',(-21.9446806457083,35.0658217301568,9.44101762226398));
#26051=CARTESIAN_POINT('Ctrl Pts',(-22.048129786773,35.1959429263773,9.62412107874912));
#26052=CARTESIAN_POINT('Ctrl Pts',(-22.1539362249973,35.3298371867842,9.80260437465981));
#26053=CARTESIAN_POINT('Ctrl Pts',(-22.259915255438,35.4639498564633,9.98137881379536));
#26054=CARTESIAN_POINT('Ctrl Pts',(-22.3682590622493,35.601847626393,10.155517727091));
#26055=CARTESIAN_POINT('Ctrl Pts',(-22.4787275806297,35.7432181181518,10.3247095747694));
#26056=CARTESIAN_POINT('Ctrl Pts',(-22.5106567217229,35.7840789755613,10.3736117457729));
#26057=CARTESIAN_POINT('Ctrl Pts',(-22.5427632651429,35.8252297828039,10.4221009095719));
#26058=CARTESIAN_POINT('Ctrl Pts',(-22.5750411898779,35.8666626160111,10.4701702229062));
#26059=CARTESIAN_POINT('Ctrl Pts',(-26.9229962078196,35.5116836434678,0.));
#26060=CARTESIAN_POINT('Ctrl Pts',(-27.1032648219977,35.3958320397273,1.72780310113342));
#26061=CARTESIAN_POINT('Ctrl Pts',(-27.6888332968115,35.9106393292986,3.28449990511991));
#26062=CARTESIAN_POINT('Ctrl Pts',(-28.2744017716253,36.42544661887,4.84119670910639));
#26063=CARTESIAN_POINT('Ctrl Pts',(-29.1849954989993,37.446003073409,5.91846432228298));
#26064=CARTESIAN_POINT('Ctrl Pts',(-30.0955892263732,38.466559527948,6.99573193545957));
#26065=CARTESIAN_POINT('Ctrl Pts',(-31.1865583607892,39.7677855943822,7.38020429521639));
#26066=CARTESIAN_POINT('Ctrl Pts',(-32.2775274952052,41.0690116608165,7.76467665497322));
#26067=CARTESIAN_POINT('Ctrl Pts',(-33.3684966296212,42.3702377272507,7.38020429521639));
#26068=CARTESIAN_POINT('Ctrl Pts',(-24.8148246247007,34.425587311519,0.));
#26069=CARTESIAN_POINT('Ctrl Pts',(-24.9950932388788,34.3097357077785,2.19648874705824));
#26070=CARTESIAN_POINT('Ctrl Pts',(-25.6906037706612,34.9956161772603,4.17545672685568));
#26071=CARTESIAN_POINT('Ctrl Pts',(-26.3861143024435,35.6814966467421,6.15442470665314));
#26072=CARTESIAN_POINT('Ctrl Pts',(-27.4948167710211,37.0103163197459,7.5239130403414));
#26073=CARTESIAN_POINT('Ctrl Pts',(-28.6035192395987,38.3391359927498,8.89340137402968));
#26074=CARTESIAN_POINT('Ctrl Pts',(-29.9415259336138,40.0247600051859,9.38216610144961));
#26075=CARTESIAN_POINT('Ctrl Pts',(-31.2795326276289,41.710384017622,9.87093082886954));
#26076=CARTESIAN_POINT('Ctrl Pts',(-32.617539321644,43.3960080300582,9.38216610144961));
#26077=CARTESIAN_POINT('Ctrl Pts',(-22.9590519566753,32.9490709821977,0.));
#26078=CARTESIAN_POINT('Ctrl Pts',(-23.1393205708534,32.8332193784572,2.70899372698069));
#26079=CARTESIAN_POINT('Ctrl Pts',(-23.9550520912434,33.7061673576817,5.14971273833323));
#26080=CARTESIAN_POINT('Ctrl Pts',(-24.7707836116334,34.5791153369062,7.59043174968577));
#26081=CARTESIAN_POINT('Ctrl Pts',(-26.0961168162189,36.2450190148584,9.27946171175751));
#26082=CARTESIAN_POINT('Ctrl Pts',(-27.4214500208045,37.9109226928106,10.9684916738293));
#26083=CARTESIAN_POINT('Ctrl Pts',(-29.0295908241597,40.0168835841567,11.5712994880388));
#26084=CARTESIAN_POINT('Ctrl Pts',(-30.637731627515,42.1228444755028,12.1741073022483));
#26085=CARTESIAN_POINT('Ctrl Pts',(-32.2458724308703,44.228805366849,11.5712994880388));
#26086=CARTESIAN_POINT('Ctrl Pts',(-21.4269965203139,31.138877952143,0.));
#26087=CARTESIAN_POINT('Ctrl Pts',(-21.6072651344921,31.0230263484025,3.24562220582793));
#26088=CARTESIAN_POINT('Ctrl Pts',(-22.5488764195076,32.0918470647273,6.16982677025168));
#26089=CARTESIAN_POINT('Ctrl Pts',(-23.4904877045231,33.1606677810521,9.0940313346754));
#26090=CARTESIAN_POINT('Ctrl Pts',(-25.0426484071616,35.1795219354007,11.1176436806954));
#26091=CARTESIAN_POINT('Ctrl Pts',(-26.5948091098001,37.1983760897494,13.1412560267153));
#26092=CARTESIAN_POINT('Ctrl Pts',(-28.4857991767897,39.7444590262842,13.8634749112255));
#26093=CARTESIAN_POINT('Ctrl Pts',(-30.3767892437793,42.2905419628191,14.5856937957357));
#26094=CARTESIAN_POINT('Ctrl Pts',(-32.2677793107688,44.8366248993539,13.8634749112255));
#26095=CARTESIAN_POINT('',(-21.4269965203139,31.138877952143,0.));
#26096=CARTESIAN_POINT('Ctrl Pts',(-21.4269965203139,31.138877952143,0.));
#26097=CARTESIAN_POINT('Ctrl Pts',(-21.6072651344921,31.0230263484025,3.24562220582793));
#26098=CARTESIAN_POINT('Ctrl Pts',(-22.5488764195076,32.0918470647273,6.16982677025167));
#26099=CARTESIAN_POINT('Ctrl Pts',(-23.334969330082,32.9841392463829,8.61106394926975));
#26100=CARTESIAN_POINT('Ctrl Pts',(-24.5639673341827,34.5610181206246,10.4489096280657));
#26101=CARTESIAN_POINT('Origin',(-35.1666259835201,19.5103534449754,0.));
#26102=CARTESIAN_POINT('Ctrl Pts',(-21.4269965203139,31.138877952143,0.));
#26103=CARTESIAN_POINT('Ctrl Pts',(-21.6072651344921,31.0230263484025,3.24562220582793));
#26104=CARTESIAN_POINT('Ctrl Pts',(-22.5488764195076,32.0918470647273,6.16982677025167));
#26105=CARTESIAN_POINT('Ctrl Pts',(-23.4904877045231,33.1606677810521,9.0940313346754));
#26106=CARTESIAN_POINT('Ctrl Pts',(-25.0426484071616,35.1795219354008,11.1176436806954));
#26107=CARTESIAN_POINT('Ctrl Pts',(-26.5948091098001,37.1983760897494,13.1412560267153));
#26108=CARTESIAN_POINT('Ctrl Pts',(-28.4857991767897,39.7444590262842,13.8634749112255));
#26109=CARTESIAN_POINT('Ctrl Pts',(-30.3767892437793,42.2905419628191,14.5856937957357));
#26110=CARTESIAN_POINT('Ctrl Pts',(-32.2677793107688,44.8366248993539,13.8634749112255));
#26111=CARTESIAN_POINT('Ctrl Pts',(-20.4854409432119,30.9950965373909,0.));
#26112=CARTESIAN_POINT('Ctrl Pts',(-20.6657095573901,30.8792449336504,3.38941559469373));
#26113=CARTESIAN_POINT('Ctrl Pts',(-21.6410512138984,32.0005511325097,6.44317352589574));
#26114=CARTESIAN_POINT('Ctrl Pts',(-22.6163928704067,33.1218573313691,9.49693145709775));
#26115=CARTESIAN_POINT('Ctrl Pts',(-24.2293336022808,35.2352870572786,11.6101975146502));
#26116=CARTESIAN_POINT('Ctrl Pts',(-25.8422743341549,37.3487167831881,13.7234635722027));
#26117=CARTESIAN_POINT('Ctrl Pts',(-27.8090558579146,40.0127335284694,14.4776794959001));
#26118=CARTESIAN_POINT('Ctrl Pts',(-29.7758373816743,42.6767502737506,15.2318954195974));
#26119=CARTESIAN_POINT('Ctrl Pts',(-31.742618905434,45.3407670190318,14.4776794959001));
#26120=CARTESIAN_POINT('Ctrl Pts',(-19.6841717937386,31.5100409519662,0.));
#26121=CARTESIAN_POINT('Ctrl Pts',(-19.8644404079168,31.3941893482258,3.38941559469373));
#26122=CARTESIAN_POINT('Ctrl Pts',(-20.8397820644251,32.5154955470851,6.44317352589574));
#26123=CARTESIAN_POINT('Ctrl Pts',(-21.8151237209334,33.6368017459444,9.49693145709774));
#26124=CARTESIAN_POINT('Ctrl Pts',(-23.4280644528075,35.7502314718539,11.6101975146502));
#26125=CARTESIAN_POINT('Ctrl Pts',(-25.0410051846816,37.8636611977635,13.7234635722027));
#26126=CARTESIAN_POINT('Ctrl Pts',(-27.0077867084413,40.5276779430447,14.4776794959001));
#26127=CARTESIAN_POINT('Ctrl Pts',(-28.974568232201,43.191694688326,15.2318954195974));
#26128=CARTESIAN_POINT('Ctrl Pts',(-30.9413497559607,45.8557114336071,14.4776794959001));
#26129=CARTESIAN_POINT('Ctrl Pts',(-19.4238236466307,32.4262389885814,0.));
#26130=CARTESIAN_POINT('Ctrl Pts',(-19.6040922608088,32.3103873848409,3.24562220582793));
#26131=CARTESIAN_POINT('Ctrl Pts',(-20.5457035458243,33.3792081011657,6.16982677025167));
#26132=CARTESIAN_POINT('Ctrl Pts',(-21.4873148308399,34.4480288174905,9.09403133467541));
#26133=CARTESIAN_POINT('Ctrl Pts',(-23.0394755334784,36.4668829718391,11.1176436806954));
#26134=CARTESIAN_POINT('Ctrl Pts',(-24.5916362361169,38.4857371261877,13.1412560267153));
#26135=CARTESIAN_POINT('Ctrl Pts',(-26.4826263031064,41.0318200627226,13.8634749112255));
#26136=CARTESIAN_POINT('Ctrl Pts',(-28.373616370096,43.5779029992574,14.5856937957357));
#26137=CARTESIAN_POINT('Ctrl Pts',(-30.2646064370856,46.1239859357923,13.8634749112255));
#26138=CARTESIAN_POINT('',(-20.1821175312213,31.4039970697443,-1.88545294716389E-29));
#26139=CARTESIAN_POINT('Origin',(-21.1552751870374,32.9182507396843,0.));
#26140=CARTESIAN_POINT('Origin',(-21.1552751870374,32.9182507396843,0.));
#26141=CARTESIAN_POINT('Ctrl Pts',(-14.6113821712781,34.8604849513724,0.));
#26142=CARTESIAN_POINT('Ctrl Pts',(-14.8063033131398,34.7714674485863,3.24562220582792));
#26143=CARTESIAN_POINT('Ctrl Pts',(-15.5862213055783,35.9634143688744,6.16982677025168));
#26144=CARTESIAN_POINT('Ctrl Pts',(-16.3661392980168,37.1553612891625,9.09403133467541));
#26145=CARTESIAN_POINT('Ctrl Pts',(-17.6151883402599,39.3745619185373,11.1176436806954));
#26146=CARTESIAN_POINT('Ctrl Pts',(-18.864237382503,41.5937625479121,13.1412560267153));
#26147=CARTESIAN_POINT('Ctrl Pts',(-20.3736345158498,44.3830459768615,13.8634749112255));
#26148=CARTESIAN_POINT('Ctrl Pts',(-21.8830316491966,47.1723294058109,14.5856937957357));
#26149=CARTESIAN_POINT('Ctrl Pts',(-23.3924287825434,49.9616128347603,13.8634749112255));
#26150=CARTESIAN_POINT('Ctrl Pts',(-15.3059217494163,37.1279962392257,0.));
#26151=CARTESIAN_POINT('Ctrl Pts',(-15.500842891278,37.0389787364396,2.70899372698069));
#26152=CARTESIAN_POINT('Ctrl Pts',(-16.1840379904938,38.0191320633214,5.14971273833323));
#26153=CARTESIAN_POINT('Ctrl Pts',(-16.8672330897096,38.9992853902031,7.59043174968578));
#26154=CARTESIAN_POINT('Ctrl Pts',(-17.9419935007385,40.8368471514173,9.27946171175752));
#26155=CARTESIAN_POINT('Ctrl Pts',(-19.0167539117674,42.6744089126315,10.9684916738293));
#26156=CARTESIAN_POINT('Ctrl Pts',(-20.3088166768303,44.9877964569988,11.5712994880388));
#26157=CARTESIAN_POINT('Ctrl Pts',(-21.6008794418932,47.3011840013661,12.1741073022483));
#26158=CARTESIAN_POINT('Ctrl Pts',(-22.8929422069561,49.6145715457333,11.5712994880388));
#26159=CARTESIAN_POINT('Ctrl Pts',(-15.5447398754877,39.4874365476045,0.));
#26160=CARTESIAN_POINT('Ctrl Pts',(-15.7396610173493,39.3984190448184,2.19648874705824));
#26161=CARTESIAN_POINT('Ctrl Pts',(-16.3304812866724,40.1762997089268,4.17545672685568));
#26162=CARTESIAN_POINT('Ctrl Pts',(-16.9213015559955,40.9541803730352,6.15442470665313));
#26163=CARTESIAN_POINT('Ctrl Pts',(-17.829608275202,42.4272593902765,7.5239130403414));
#26164=CARTESIAN_POINT('Ctrl Pts',(-18.7379149944086,43.9003384075177,8.89340137402968));
#26165=CARTESIAN_POINT('Ctrl Pts',(-19.8224134008055,45.7592234042437,9.3821661014496));
#26166=CARTESIAN_POINT('Ctrl Pts',(-20.9069118072024,47.6181084009697,9.87093082886953));
#26167=CARTESIAN_POINT('Ctrl Pts',(-21.9914102135993,49.4769933976957,9.3821661014496));
#26168=CARTESIAN_POINT('Ctrl Pts',(-15.3186586437005,41.8481313484579,0.));
#26169=CARTESIAN_POINT('Ctrl Pts',(-15.5135797855622,41.7591138456718,1.72780310113343));
#26170=CARTESIAN_POINT('Ctrl Pts',(-16.0199233014651,42.3520162221172,3.28449990511991));
#26171=CARTESIAN_POINT('Ctrl Pts',(-16.5262668173681,42.9449185985626,4.84119670910638));
#26172=CARTESIAN_POINT('Ctrl Pts',(-17.2823516867886,44.0846782589592,5.91846432228297));
#26173=CARTESIAN_POINT('Ctrl Pts',(-18.0384365562092,45.2244379193558,6.99573193545956));
#26174=CARTESIAN_POINT('Ctrl Pts',(-18.9331174206828,46.6676804765723,7.38020429521639));
#26175=CARTESIAN_POINT('Ctrl Pts',(-19.8277982851565,48.1109230337888,7.76467665497321));
#26176=CARTESIAN_POINT('Ctrl Pts',(-20.7224791496302,49.5541655910054,7.38020429521638));
#26177=CARTESIAN_POINT('',(-14.6113821712892,34.8604849513849,1.57949266918924E-9));
#26178=CARTESIAN_POINT('Origin',(2.5993596565155,40.1321417817282,0.));
#26179=CARTESIAN_POINT('Ctrl Pts',(-14.6113821714912,34.8604849513683,3.13106059869152E-9));
#26180=CARTESIAN_POINT('Ctrl Pts',(-14.626098337786,34.853764303467,0.245038153335648));
#26181=CARTESIAN_POINT('Ctrl Pts',(-14.6435771646297,34.8527495154069,0.490791160522061));
#26182=CARTESIAN_POINT('Ctrl Pts',(-14.6638259110835,34.8575316463561,0.736766500725887));
#26183=CARTESIAN_POINT('Ctrl Pts',(-14.6840081820399,34.8622980778379,0.981934317701575));
#26184=CARTESIAN_POINT('Ctrl Pts',(-14.7069422331333,34.8728235332129,1.22732257376626));
#26185=CARTESIAN_POINT('Ctrl Pts',(-14.7326128792078,34.8891527148322,1.47243294816407));
#26186=CARTESIAN_POINT('Ctrl Pts',(-14.7582448644192,34.9054573041506,1.71717417803084));
#26187=CARTESIAN_POINT('Ctrl Pts',(-14.7866052020689,34.9275482079566,1.96163791541655));
#26188=CARTESIAN_POINT('Ctrl Pts',(-14.8176563354397,34.9554233023889,2.20532408778594));
#26189=CARTESIAN_POINT('Ctrl Pts',(-14.8486808377692,34.9832744897134,2.44880126242133));
#26190=CARTESIAN_POINT('Ctrl Pts',(-14.882391488439,35.0168999484378,2.69150175431114));
#26191=CARTESIAN_POINT('Ctrl Pts',(-14.9187287035022,35.056250564147,2.9329295186687));
#26192=CARTESIAN_POINT('Ctrl Pts',(-14.9550583167476,35.0955929476289,3.17430677585636));
#26193=CARTESIAN_POINT('Ctrl Pts',(-14.9940133343939,35.1406580326361,3.41441139318375));
#26194=CARTESIAN_POINT('Ctrl Pts',(-15.0355127954201,35.1913501978217,3.65275710614652));
#26195=CARTESIAN_POINT('Ctrl Pts',(-15.0770649517991,35.2421067311088,3.89140546668806));
#26196=CARTESIAN_POINT('Ctrl Pts',(-15.1211679328244,35.2985045323754,4.12829002081184));
#26197=CARTESIAN_POINT('Ctrl Pts',(-15.1677200855872,35.3604022296524,4.3629387437783));
#26198=CARTESIAN_POINT('Ctrl Pts',(-15.2143197401098,35.422363087264,4.59782690201477));
#26199=CARTESIAN_POINT('Ctrl Pts',(-15.2633734552291,35.4898348974064,4.83047425894994));
#26200=CARTESIAN_POINT('Ctrl Pts',(-15.314760335032,35.5626325521734,5.06042975959473));
#26201=CARTESIAN_POINT('Ctrl Pts',(-15.3662974499284,35.6356430387471,5.2910575599835));
#26202=CARTESIAN_POINT('Ctrl Pts',(-15.4201812613939,35.714010340131,5.51897736305736));
#26203=CARTESIAN_POINT('Ctrl Pts',(-15.4762725955035,35.797507103918,5.74376259354382));
#26204=CARTESIAN_POINT('Ctrl Pts',(-15.5120380980665,35.8507471233724,5.88709234072653));
#26205=CARTESIAN_POINT('Ctrl Pts',(-15.5487007750603,35.9060718261752,6.0291482531421));
#26206=CARTESIAN_POINT('Ctrl Pts',(-15.5862213055882,35.9634143689083,6.16982677023484));
#26207=CARTESIAN_POINT('Ctrl Pts',(-15.6450546012012,36.0533291627655,6.39041482339101));
#26208=CARTESIAN_POINT('Ctrl Pts',(-15.7065142910193,36.1486520067523,6.60890054011825));
#26209=CARTESIAN_POINT('Ctrl Pts',(-15.7705155506318,36.2492721362564,6.82480412008071));
#26210=CARTESIAN_POINT('Ctrl Pts',(-15.8343723238085,36.3496651101705,7.04022028559322));
#26211=CARTESIAN_POINT('Ctrl Pts',(-15.9007591428904,36.4553314094027,7.25306552029667));
#26212=CARTESIAN_POINT('Ctrl Pts',(-15.9695695446608,36.5661159087968,7.46287566269448));
#26213=CARTESIAN_POINT('Ctrl Pts',(-16.038269271112,36.6767222213247,7.67234834441917));
#26214=CARTESIAN_POINT('Ctrl Pts',(-16.1093847013533,36.7924301575639,7.87879526533069));
#26215=CARTESIAN_POINT('Ctrl Pts',(-16.1827888425358,36.9130417770844,8.0817733461224));
#26216=CARTESIAN_POINT('Ctrl Pts',(-16.2561225498034,37.0335376654159,8.28455666214169));
#26217=CARTESIAN_POINT('Ctrl Pts',(-16.3317404631319,37.1589276519422,8.48387739272926));
#26218=CARTESIAN_POINT('Ctrl Pts',(-16.4094964608252,37.2889731283962,8.67931873611179));
#26219=CARTESIAN_POINT('Ctrl Pts',(-16.4872561983762,37.4190248596934,8.87476947970566));
#26220=CARTESIAN_POINT('Ctrl Pts',(-16.5671540886073,37.5537323016305,9.06634009532891));
#26221=CARTESIAN_POINT('Ctrl Pts',(-16.6490263722365,37.6928185909677,9.25364450341035));
#26222=CARTESIAN_POINT('Ctrl Pts',(-16.7309286899051,37.8319559027375,9.44101762226545));
#26223=CARTESIAN_POINT('Ctrl Pts',(-16.8148066908792,37.9754750005801,9.62412107875081));
#26224=CARTESIAN_POINT('Ctrl Pts',(-16.9004810321072,38.12306423662,9.80260437466171));
#26225=CARTESIAN_POINT('Ctrl Pts',(-16.9862951259314,38.2708942212739,9.98137881379724));
#26226=CARTESIAN_POINT('Ctrl Pts',(-17.0739112501825,38.4228073220822,10.1555177270929));
#26227=CARTESIAN_POINT('Ctrl Pts',(-17.163136239657,38.5784601754019,10.3247095747712));
#26228=CARTESIAN_POINT('Ctrl Pts',(-17.1889252818185,38.6234491187513,10.3736117457758));
#26229=CARTESIAN_POINT('Ctrl Pts',(-17.2148486564433,38.6687503076461,10.4221009095758));
#26230=CARTESIAN_POINT('Ctrl Pts',(-17.2409015314889,38.7143550419919,10.4701702229111));
#26231=CARTESIAN_POINT('Ctrl Pts',(-21.5951194116467,38.9817677587449,1.04083408558608E-14));
#26232=CARTESIAN_POINT('Ctrl Pts',(-21.7900405535084,38.8927502559588,1.72780310113342));
#26233=CARTESIAN_POINT('Ctrl Pts',(-22.2963840694113,39.4856526324042,3.28449990511991));
#26234=CARTESIAN_POINT('Ctrl Pts',(-22.8027275853143,40.0785550088496,4.84119670910639));
#26235=CARTESIAN_POINT('Ctrl Pts',(-23.5588124547348,41.2183146692462,5.91846432228298));
#26236=CARTESIAN_POINT('Ctrl Pts',(-24.3148973241554,42.3580743296428,6.99573193545956));
#26237=CARTESIAN_POINT('Ctrl Pts',(-25.209578188629,43.8013168868593,7.38020429521639));
#26238=CARTESIAN_POINT('Ctrl Pts',(-26.1042590531027,45.2445594440758,7.76467665497322));
#26239=CARTESIAN_POINT('Ctrl Pts',(-26.9989399175764,46.6878020012924,7.38020429521639));
#26240=CARTESIAN_POINT('Ctrl Pts',(-19.662973599342,37.6067022235299,0.));
#26241=CARTESIAN_POINT('Ctrl Pts',(-19.8578947412037,37.5176847207437,2.19648874705823));
#26242=CARTESIAN_POINT('Ctrl Pts',(-20.4487150105268,38.2955653848522,4.17545672685568));
#26243=CARTESIAN_POINT('Ctrl Pts',(-21.0395352798499,39.0734460489606,6.15442470665314));
#26244=CARTESIAN_POINT('Ctrl Pts',(-21.9478419990564,40.5465250662018,7.5239130403414));
#26245=CARTESIAN_POINT('Ctrl Pts',(-22.856148718263,42.019604083443,8.89340137402967));
#26246=CARTESIAN_POINT('Ctrl Pts',(-23.9406471246599,43.878489080169,9.38216610144961));
#26247=CARTESIAN_POINT('Ctrl Pts',(-25.0251455310568,45.737374076895,9.87093082886953));
#26248=CARTESIAN_POINT('Ctrl Pts',(-26.1096439374538,47.596259073621,9.3821661014496));
#26249=CARTESIAN_POINT('Ctrl Pts',(-18.0362202038891,35.8811107143583,0.));
#26250=CARTESIAN_POINT('Ctrl Pts',(-18.2311413457508,35.7920932115722,2.70899372698069));
#26251=CARTESIAN_POINT('Ctrl Pts',(-18.9143364449666,36.772246538454,5.14971273833323));
#26252=CARTESIAN_POINT('Ctrl Pts',(-19.5975315441824,37.7523998653357,7.59043174968577));
#26253=CARTESIAN_POINT('Ctrl Pts',(-20.6722919552113,39.5899616265499,9.27946171175751));
#26254=CARTESIAN_POINT('Ctrl Pts',(-21.7470523662402,41.4275233877641,10.9684916738293));
#26255=CARTESIAN_POINT('Ctrl Pts',(-23.0391151313031,43.7409109321314,11.5712994880388));
#26256=CARTESIAN_POINT('Ctrl Pts',(-24.331177896366,46.0542984764986,12.1741073022483));
#26257=CARTESIAN_POINT('Ctrl Pts',(-25.6232406614289,48.3676860208659,11.5712994880388));
#26258=CARTESIAN_POINT('Ctrl Pts',(-16.7773762111441,33.8713086176153,0.));
#26259=CARTESIAN_POINT('Ctrl Pts',(-16.9722973530057,33.7822911148292,3.24562220582792));
#26260=CARTESIAN_POINT('Ctrl Pts',(-17.7522153454443,34.9742380351173,6.16982677025168));
#26261=CARTESIAN_POINT('Ctrl Pts',(-18.5321333378828,36.1661849554054,9.09403133467541));
#26262=CARTESIAN_POINT('Ctrl Pts',(-19.7811823801259,38.3853855847802,11.1176436806954));
#26263=CARTESIAN_POINT('Ctrl Pts',(-21.030231422369,40.604586214155,13.1412560267153));
#26264=CARTESIAN_POINT('Ctrl Pts',(-22.5396285557158,43.3938696431044,13.8634749112255));
#26265=CARTESIAN_POINT('Ctrl Pts',(-24.0490256890626,46.1831530720538,14.5856937957357));
#26266=CARTESIAN_POINT('Ctrl Pts',(-25.5584228224094,48.9724365010032,13.8634749112255));
#26267=CARTESIAN_POINT('',(-16.7773762111441,33.8713086176153,0.));
#26268=CARTESIAN_POINT('Ctrl Pts',(-16.7773762111441,33.8713086176153,0.));
#26269=CARTESIAN_POINT('Ctrl Pts',(-16.9722973530058,33.7822911148292,3.24562220582792));
#26270=CARTESIAN_POINT('Ctrl Pts',(-17.7522153454443,34.9742380351173,6.16982677025168));
#26271=CARTESIAN_POINT('Ctrl Pts',(-18.4033205461166,35.9693206543789,8.61106394926976));
#26272=CARTESIAN_POINT('Ctrl Pts',(-19.3953958606401,37.7050538275442,10.4489096280657));
#26273=CARTESIAN_POINT('Origin',(-32.032067641919,24.3164988679739,0.));
#26274=CARTESIAN_POINT('Ctrl Pts',(-16.7773762111441,33.8713086176153,0.));
#26275=CARTESIAN_POINT('Ctrl Pts',(-16.9722973530058,33.7822911148292,3.24562220582792));
#26276=CARTESIAN_POINT('Ctrl Pts',(-17.7522153454443,34.9742380351173,6.16982677025167));
#26277=CARTESIAN_POINT('Ctrl Pts',(-18.5321333378828,36.1661849554054,9.09403133467541));
#26278=CARTESIAN_POINT('Ctrl Pts',(-19.7811823801259,38.3853855847802,11.1176436806954));
#26279=CARTESIAN_POINT('Ctrl Pts',(-21.030231422369,40.604586214155,13.1412560267153));
#26280=CARTESIAN_POINT('Ctrl Pts',(-22.5396285557158,43.3938696431044,13.8634749112255));
#26281=CARTESIAN_POINT('Ctrl Pts',(-24.0490256890626,46.1831530720538,14.5856937957357));
#26282=CARTESIAN_POINT('Ctrl Pts',(-25.5584228224094,48.9724365010032,13.8634749112255));
#26283=CARTESIAN_POINT('Ctrl Pts',(-15.8658665409931,33.5949933606691,6.24500451351651E-15));
#26284=CARTESIAN_POINT('Ctrl Pts',(-16.0607876828548,33.505975857883,3.38941559469373));
#26285=CARTESIAN_POINT('Ctrl Pts',(-16.8666232572809,34.7546743665351,6.44317352589573));
#26286=CARTESIAN_POINT('Ctrl Pts',(-17.672458831707,36.0033728751873,9.49693145709774));
#26287=CARTESIAN_POINT('Ctrl Pts',(-18.9682097429543,38.3248363332021,11.6101975146502));
#26288=CARTESIAN_POINT('Ctrl Pts',(-20.2639606542016,40.646299791217,13.7234635722027));
#26289=CARTESIAN_POINT('Ctrl Pts',(-21.8315940656522,43.5631028816989,14.4776794959001));
#26290=CARTESIAN_POINT('Ctrl Pts',(-23.3992274771028,46.4799059721809,15.2318954195974));
#26291=CARTESIAN_POINT('Ctrl Pts',(-24.9668608885534,49.3967090626629,14.4776794959001));
#26292=CARTESIAN_POINT('Ctrl Pts',(-14.9994689250467,33.9906638941719,0.));
#26293=CARTESIAN_POINT('Ctrl Pts',(-15.1943900669084,33.9016463913858,3.38941559469373));
#26294=CARTESIAN_POINT('Ctrl Pts',(-16.0002256413345,35.150344900038,6.44317352589574));
#26295=CARTESIAN_POINT('Ctrl Pts',(-16.8060612157606,36.3990434086901,9.49693145709774));
#26296=CARTESIAN_POINT('Ctrl Pts',(-18.1018121270079,38.7205068667049,11.6101975146502));
#26297=CARTESIAN_POINT('Ctrl Pts',(-19.3975630382553,41.0419703247198,13.7234635722027));
#26298=CARTESIAN_POINT('Ctrl Pts',(-20.9651964497058,43.9587734152018,14.4776794959001));
#26299=CARTESIAN_POINT('Ctrl Pts',(-22.5328298611564,46.8755765056838,15.2318954195974));
#26300=CARTESIAN_POINT('Ctrl Pts',(-24.100463272607,49.7923795961657,14.4776794959001));
#26301=CARTESIAN_POINT('Ctrl Pts',(-14.6113821712781,34.8604849513724,0.));
#26302=CARTESIAN_POINT('Ctrl Pts',(-14.8063033131398,34.7714674485863,3.24562220582792));
#26303=CARTESIAN_POINT('Ctrl Pts',(-15.5862213055783,35.9634143688743,6.16982677025168));
#26304=CARTESIAN_POINT('Ctrl Pts',(-16.3661392980168,37.1553612891625,9.09403133467541));
#26305=CARTESIAN_POINT('Ctrl Pts',(-17.6151883402599,39.3745619185373,11.1176436806954));
#26306=CARTESIAN_POINT('Ctrl Pts',(-18.864237382503,41.5937625479121,13.1412560267153));
#26307=CARTESIAN_POINT('Ctrl Pts',(-20.3736345158498,44.3830459768615,13.8634749112255));
#26308=CARTESIAN_POINT('Ctrl Pts',(-21.8830316491966,47.1723294058109,14.5856937957357));
#26309=CARTESIAN_POINT('Ctrl Pts',(-23.3924287825434,49.9616128347603,13.8634749112255));
#26310=CARTESIAN_POINT('',(-15.507437910779,33.9565644528989,-1.82251475137849E-29));
#26311=CARTESIAN_POINT('Origin',(-16.2551894587636,35.5938999782225,0.));
#26312=CARTESIAN_POINT('Origin',(-16.2551894587636,35.5938999782225,0.));
#26313=CARTESIAN_POINT('Ctrl Pts',(-9.50149509066497,36.5850719698906,0.));
#26314=CARTESIAN_POINT('Ctrl Pts',(-9.70710072786806,36.5247007077103,3.24562220582793));
#26315=CARTESIAN_POINT('Ctrl Pts',(-10.3094485465013,37.8155092299557,6.16982677025168));
#26316=CARTESIAN_POINT('Ctrl Pts',(-10.9117963651345,39.1063177522011,9.09403133467541));
#26317=CARTESIAN_POINT('Ctrl Pts',(-11.8323067104422,41.4806883314342,11.1176436806954));
#26318=CARTESIAN_POINT('Ctrl Pts',(-12.7528170557497,43.8550589106673,13.1412560267153));
#26319=CARTESIAN_POINT('Ctrl Pts',(-13.8498942825608,46.830761065047,13.8634749112255));
#26320=CARTESIAN_POINT('Ctrl Pts',(-14.9469715093718,49.8064632194267,14.5856937957357));
#26321=CARTESIAN_POINT('Ctrl Pts',(-16.0440487361828,52.7821653738064,13.8634749112255));
#26322=CARTESIAN_POINT('Ctrl Pts',(-9.86626475512738,38.928346550052,0.));
#26323=CARTESIAN_POINT('Ctrl Pts',(-10.0718703923305,38.8679752878717,2.7089937269807));
#26324=CARTESIAN_POINT('Ctrl Pts',(-10.6086211883241,39.9353808672042,5.14971273833323));
#26325=CARTESIAN_POINT('Ctrl Pts',(-11.1453719843177,41.0027864465367,7.59043174968578));
#26326=CARTESIAN_POINT('Ctrl Pts',(-11.9476805791745,42.9745988326451,9.27946171175752));
#26327=CARTESIAN_POINT('Ctrl Pts',(-12.7499891740313,44.9464112187535,10.9684916738293));
#26328=CARTESIAN_POINT('Ctrl Pts',(-13.6996712289065,47.4201315169974,11.5712994880388));
#26329=CARTESIAN_POINT('Ctrl Pts',(-14.6493532837816,49.8938518152412,12.1741073022483));
#26330=CARTESIAN_POINT('Ctrl Pts',(-15.5990353386568,52.3675721134851,11.5712994880388));
#26331=CARTESIAN_POINT('Ctrl Pts',(-9.76686869112026,41.297758521112,0.));
#26332=CARTESIAN_POINT('Ctrl Pts',(-9.97247432832337,41.2373872589318,2.19648874705823));
#26333=CARTESIAN_POINT('Ctrl Pts',(-10.4465769382887,42.0914327105681,4.17545672685568));
#26334=CARTESIAN_POINT('Ctrl Pts',(-10.920679548254,42.9454781622045,6.15442470665314));
#26335=CARTESIAN_POINT('Ctrl Pts',(-11.6101000126267,44.5328288829012,7.5239130403414));
#26336=CARTESIAN_POINT('Ctrl Pts',(-12.2995204769994,46.1201796035979,8.89340137402967));
#26337=CARTESIAN_POINT('Ctrl Pts',(-13.1084333356591,48.114484046662,9.38216610144961));
#26338=CARTESIAN_POINT('Ctrl Pts',(-13.9173461943188,50.1087884897262,9.87093082886954));
#26339=CARTESIAN_POINT('Ctrl Pts',(-14.7262590529785,52.1030929327904,9.3821661014496));
#26340=CARTESIAN_POINT('Ctrl Pts',(-9.20712674149444,43.6022501387952,0.));
#26341=CARTESIAN_POINT('Ctrl Pts',(-9.41273237869755,43.5418788766149,1.72780310113343));
#26342=CARTESIAN_POINT('Ctrl Pts',(-9.82954324187999,44.2008065573391,3.28449990511991));
#26343=CARTESIAN_POINT('Ctrl Pts',(-10.2463541050624,44.8597342380634,4.84119670910639));
#26344=CARTESIAN_POINT('Ctrl Pts',(-10.8325384089569,46.0954948844273,5.91846432228299));
#26345=CARTESIAN_POINT('Ctrl Pts',(-11.4187227128513,47.3312555307913,6.99573193545957));
#26346=CARTESIAN_POINT('Ctrl Pts',(-12.0989021850286,48.887134322293,7.3802042952164));
#26347=CARTESIAN_POINT('Ctrl Pts',(-12.7790816572058,50.4430131137948,7.76467665497322));
#26348=CARTESIAN_POINT('Ctrl Pts',(-13.459261129383,51.9988919052966,7.38020429521639));
#26349=CARTESIAN_POINT('',(-9.50149509067415,36.5850719699045,1.57949201998838E-9));
#26350=CARTESIAN_POINT('Origin',(8.2843011904065,39.3537269950291,0.));
#26351=CARTESIAN_POINT('Ctrl Pts',(-9.50149509087647,36.5850719699169,3.13105443220166E-9));
#26352=CARTESIAN_POINT('Ctrl Pts',(-9.51701791573658,36.5805140573471,0.24503815333567));
#26353=CARTESIAN_POINT('Ctrl Pts',(-9.53446325272403,36.5819970947817,0.49079116052211));
#26354=CARTESIAN_POINT('Ctrl Pts',(-9.55382532794258,36.5896122476099,0.736766500725963));
#26355=CARTESIAN_POINT('Ctrl Pts',(-9.57312383855555,36.597202400319,0.981934317701606));
#26356=CARTESIAN_POINT('Ctrl Pts',(-9.59432652559756,36.6108845775071,1.22732257376625));
#26357=CARTESIAN_POINT('Ctrl Pts',(-9.6174119966677,36.6307008654467,1.47243294816401));
#26358=CARTESIAN_POINT('Ctrl Pts',(-9.64046270023601,36.650487309385,1.71717417803076));
#26359=CARTESIAN_POINT('Ctrl Pts',(-9.6653905071382,36.6763894565088,1.96163791541645));
#26360=CARTESIAN_POINT('Ctrl Pts',(-9.69215854518732,36.7083998596961,2.20532408778582));
#26361=CARTESIAN_POINT('Ctrl Pts',(-9.71890362559695,36.7403828091233,2.44880126242125));
#26362=CARTESIAN_POINT('Ctrl Pts',(-9.74748574872948,36.77846353496,2.6915017543111));
#26363=CARTESIAN_POINT('Ctrl Pts',(-9.77785292682669,36.8225849430252,2.9329295186687));
#26364=CARTESIAN_POINT('Ctrl Pts',(-9.80821375204967,36.8666971208038,3.17430677585648));
#26365=CARTESIAN_POINT('Ctrl Pts',(-9.84035883350025,36.9168473852605,3.41441139318398));
#26366=CARTESIAN_POINT('Ctrl Pts',(-9.87422164256049,36.9729295663809,3.65275710614687));
#26367=CARTESIAN_POINT('Ctrl Pts',(-9.9081274500747,37.029082959759,3.89140546668844));
#26368=CARTESIAN_POINT('Ctrl Pts',(-9.94375528237817,37.0911832213397,4.12829002081224));
#26369=CARTESIAN_POINT('Ctrl Pts',(-9.98102464057106,37.1590759513992,4.36293874377873));
#26370=CARTESIAN_POINT('Ctrl Pts',(-10.0183320283715,37.2270379591174,4.59782690201505));
#26371=CARTESIAN_POINT('Ctrl Pts',(-10.0572842076521,37.3008040750528,4.83047425895008));
#26372=CARTESIAN_POINT('Ctrl Pts',(-10.0977878566475,37.3801738701483,5.06042975959472));
#26373=CARTESIAN_POINT('Ctrl Pts',(-10.1384099224356,37.4597757114126,5.29105755998346));
#26374=CARTESIAN_POINT('Ctrl Pts',(-10.1805924445721,37.5450138125791,5.5189773630573));
#26375=CARTESIAN_POINT('Ctrl Pts',(-10.2242300213428,37.6356433288454,5.74376259354374));
#26376=CARTESIAN_POINT('Ctrl Pts',(-10.2520546379009,37.6934314033806,5.88709234072648));
#26377=CARTESIAN_POINT('Ctrl Pts',(-10.2804706155743,37.7534106234275,6.02914825314207));
#26378=CARTESIAN_POINT('Ctrl Pts',(-10.3094485465063,37.8155092299907,6.16982677023484));
#26379=CARTESIAN_POINT('Ctrl Pts',(-10.3548867946544,37.912881671843,6.39041482339094));
#26380=CARTESIAN_POINT('Ctrl Pts',(-10.4021550583219,38.015980892539,6.60890054011811));
#26381=CARTESIAN_POINT('Ctrl Pts',(-10.4511851399364,38.124685183118,6.8248041200805));
#26382=CARTESIAN_POINT('Ctrl Pts',(-10.5001045333897,38.2331440676597,7.04022028559304));
#26383=CARTESIAN_POINT('Ctrl Pts',(-10.550777748089,38.3471826657451,7.25306552029652));
#26384=CARTESIAN_POINT('Ctrl Pts',(-10.6031214810714,38.4666322798728,7.46287566269435));
#26385=CARTESIAN_POINT('Ctrl Pts',(-10.6553810238846,38.5858897700797,7.672348344419));
#26386=CARTESIAN_POINT('Ctrl Pts',(-10.7093056453533,38.7105407473185,7.87879526533047));
#26387=CARTESIAN_POINT('Ctrl Pts',(-10.7647978150926,38.8403712129408,8.08177334612214));
#26388=CARTESIAN_POINT('Ctrl Pts',(-10.8202367380982,38.9700771015595,8.28455666214125));
#26389=CARTESIAN_POINT('Ctrl Pts',(-10.8772401144473,39.1049523499262,8.48387739272865));
#26390=CARTESIAN_POINT('Ctrl Pts',(-10.9356972672492,39.2447399831763,8.67931873611101));
#26391=CARTESIAN_POINT('Ctrl Pts',(-10.9941572316855,39.3845343398417,8.87476947970485));
#26392=CARTESIAN_POINT('Ctrl Pts',(-11.0540710087838,39.5292413095786,9.06634009532808));
#26393=CARTESIAN_POINT('Ctrl Pts',(-11.1153159078427,39.6785635418399,9.25364450340949));
#26394=CARTESIAN_POINT('Ctrl Pts',(-11.1765832739884,39.8279405514883,9.4410176222643));
#26395=CARTESIAN_POINT('Ctrl Pts',(-11.2391826206559,39.9819359159954,9.62412107874938));
#26396=CARTESIAN_POINT('Ctrl Pts',(-11.3029807823645,40.1402156364342,9.80260437466002));
#26397=CARTESIAN_POINT('Ctrl Pts',(-11.3668830120893,40.2987535438817,9.98137881379555));
#26398=CARTESIAN_POINT('Ctrl Pts',(-11.4319878421544,40.4615894629173,10.1555177270912));
#26399=CARTESIAN_POINT('Ctrl Pts',(-11.4981529392408,40.62835603457,10.3247095747696));
#26400=CARTESIAN_POINT('Ctrl Pts',(-11.5172768919406,40.6765572187082,10.373611745773));
#26401=CARTESIAN_POINT('Ctrl Pts',(-11.5364893726185,40.725086587685,10.422100909572));
#26402=CARTESIAN_POINT('Ctrl Pts',(-11.5557868365679,40.7739348422893,10.4701702229062));
#26403=CARTESIAN_POINT('Ctrl Pts',(-15.8276282594345,41.6582954965894,0.));
#26404=CARTESIAN_POINT('Ctrl Pts',(-16.0332338966376,41.597924234409,1.72780310113343));
#26405=CARTESIAN_POINT('Ctrl Pts',(-16.45004475982,42.2568519151333,3.28449990511991));
#26406=CARTESIAN_POINT('Ctrl Pts',(-16.8668556230025,42.9157795958576,4.84119670910639));
#26407=CARTESIAN_POINT('Ctrl Pts',(-17.4530399268969,44.1515402422215,5.91846432228299));
#26408=CARTESIAN_POINT('Ctrl Pts',(-18.0392242307914,45.3873008885855,6.99573193545956));
#26409=CARTESIAN_POINT('Ctrl Pts',(-18.7194037029686,46.9431796800872,7.38020429521639));
#26410=CARTESIAN_POINT('Ctrl Pts',(-19.3995831751458,48.499058471589,7.76467665497322));
#26411=CARTESIAN_POINT('Ctrl Pts',(-20.079762647323,50.0549372630908,7.38020429521639));
#26412=CARTESIAN_POINT('Ctrl Pts',(-14.1108411348342,40.0222531270434,0.));
#26413=CARTESIAN_POINT('Ctrl Pts',(-14.3164467720373,39.9618818648631,2.19648874705823));
#26414=CARTESIAN_POINT('Ctrl Pts',(-14.7905493820026,40.8159273164995,4.17545672685568));
#26415=CARTESIAN_POINT('Ctrl Pts',(-15.264651991968,41.6699727681359,6.15442470665314));
#26416=CARTESIAN_POINT('Ctrl Pts',(-15.9540724563407,43.2573234888326,7.52391304034139));
#26417=CARTESIAN_POINT('Ctrl Pts',(-16.6434929207134,44.8446742095293,8.89340137402967));
#26418=CARTESIAN_POINT('Ctrl Pts',(-17.4524057793731,46.8389786525934,9.38216610144961));
#26419=CARTESIAN_POINT('Ctrl Pts',(-18.2613186380328,48.8332830956576,9.87093082886954));
#26420=CARTESIAN_POINT('Ctrl Pts',(-19.0702314966925,50.8275875387218,9.3821661014496));
#26421=CARTESIAN_POINT('Ctrl Pts',(-12.7462230199157,38.0827145049534,0.));
#26422=CARTESIAN_POINT('Ctrl Pts',(-12.9518286571189,38.0223432427731,2.70899372698069));
#26423=CARTESIAN_POINT('Ctrl Pts',(-13.4885794531125,39.0897488221056,5.14971273833323));
#26424=CARTESIAN_POINT('Ctrl Pts',(-14.0253302491061,40.1571544014381,7.59043174968578));
#26425=CARTESIAN_POINT('Ctrl Pts',(-14.8276388439629,42.1289667875465,9.27946171175752));
#26426=CARTESIAN_POINT('Ctrl Pts',(-15.6299474388197,44.1007791736549,10.9684916738293));
#26427=CARTESIAN_POINT('Ctrl Pts',(-16.5796294936948,46.5744994718987,11.5712994880388));
#26428=CARTESIAN_POINT('Ctrl Pts',(-17.52931154857,49.0482197701426,12.1741073022483));
#26429=CARTESIAN_POINT('Ctrl Pts',(-18.4789936034451,51.5219400683864,11.5712994880388));
#26430=CARTESIAN_POINT('Ctrl Pts',(-11.786216904273,35.9142171164211,0.));
#26431=CARTESIAN_POINT('Ctrl Pts',(-11.9918225414761,35.8538458542408,3.24562220582793));
#26432=CARTESIAN_POINT('Ctrl Pts',(-12.5941703601094,37.1446543764862,6.16982677025168));
#26433=CARTESIAN_POINT('Ctrl Pts',(-13.1965181787426,38.4354628987316,9.09403133467541));
#26434=CARTESIAN_POINT('Ctrl Pts',(-14.1170285240502,40.8098334779647,11.1176436806954));
#26435=CARTESIAN_POINT('Ctrl Pts',(-15.0375388693578,43.1842040571978,13.1412560267153));
#26436=CARTESIAN_POINT('Ctrl Pts',(-16.1346160961688,46.1599062115775,13.8634749112255));
#26437=CARTESIAN_POINT('Ctrl Pts',(-17.2316933229798,49.1356083659572,14.5856937957357));
#26438=CARTESIAN_POINT('Ctrl Pts',(-18.3287705497908,52.1113105203369,13.8634749112255));
#26439=CARTESIAN_POINT('',(-11.786216904273,35.9142171164211,0.));
#26440=CARTESIAN_POINT('Ctrl Pts',(-11.786216904273,35.9142171164211,0.));
#26441=CARTESIAN_POINT('Ctrl Pts',(-11.9918225414761,35.8538458542408,3.24562220582793));
#26442=CARTESIAN_POINT('Ctrl Pts',(-12.5941703601094,37.1446543764862,6.16982677025168));
#26443=CARTESIAN_POINT('Ctrl Pts',(-13.0970332266263,38.2222704208069,8.61106394926976));
#26444=CARTESIAN_POINT('Ctrl Pts',(-13.8319900590778,40.0815233709313,10.4489096280657));
#26445=CARTESIAN_POINT('Origin',(-28.2454287759836,28.6276304970127,1.04083408558608E-14));
#26446=CARTESIAN_POINT('Ctrl Pts',(-11.786216904273,35.9142171164211,0.));
#26447=CARTESIAN_POINT('Ctrl Pts',(-11.9918225414761,35.8538458542408,3.24562220582793));
#26448=CARTESIAN_POINT('Ctrl Pts',(-12.5941703601094,37.1446543764862,6.16982677025168));
#26449=CARTESIAN_POINT('Ctrl Pts',(-13.1965181787426,38.4354628987316,9.09403133467541));
#26450=CARTESIAN_POINT('Ctrl Pts',(-14.1170285240502,40.8098334779647,11.1176436806954));
#26451=CARTESIAN_POINT('Ctrl Pts',(-15.0375388693578,43.1842040571978,13.1412560267153));
#26452=CARTESIAN_POINT('Ctrl Pts',(-16.1346160961688,46.1599062115775,13.8634749112255));
#26453=CARTESIAN_POINT('Ctrl Pts',(-17.2316933229798,49.1356083659571,14.5856937957357));
#26454=CARTESIAN_POINT('Ctrl Pts',(-18.3287705497908,52.1113105203369,13.8634749112255));
#26455=CARTESIAN_POINT('Ctrl Pts',(-10.9233088493805,35.5109929990848,6.24500451351651E-15));
#26456=CARTESIAN_POINT('Ctrl Pts',(-11.1289144865836,35.4506217369045,3.38941559469372));
#26457=CARTESIAN_POINT('Ctrl Pts',(-11.7488394904701,36.8012926546625,6.44317352589573));
#26458=CARTESIAN_POINT('Ctrl Pts',(-12.3687644943566,38.1519635724204,9.49693145709774));
#26459=CARTESIAN_POINT('Ctrl Pts',(-13.3209478330612,40.6342024610832,11.6101975146502));
#26460=CARTESIAN_POINT('Ctrl Pts',(-14.2731311717658,43.116441349746,13.7234635722027));
#26461=CARTESIAN_POINT('Ctrl Pts',(-15.4097039753316,46.226653085872,14.4776794959001));
#26462=CARTESIAN_POINT('Ctrl Pts',(-16.5462767788974,49.336864821998,15.2318954195974));
#26463=CARTESIAN_POINT('Ctrl Pts',(-17.6828495824632,52.447076558124,14.4776794959001));
#26464=CARTESIAN_POINT('Ctrl Pts',(-10.0094201239373,35.7793349404726,6.24500451351651E-15));
#26465=CARTESIAN_POINT('Ctrl Pts',(-10.2150257611404,35.7189636782923,3.38941559469372));
#26466=CARTESIAN_POINT('Ctrl Pts',(-10.8349507650269,37.0696345960502,6.44317352589573));
#26467=CARTESIAN_POINT('Ctrl Pts',(-11.4548757689134,38.4203055138082,9.49693145709774));
#26468=CARTESIAN_POINT('Ctrl Pts',(-12.407059107618,40.902544402471,11.6101975146502));
#26469=CARTESIAN_POINT('Ctrl Pts',(-13.3592424463226,43.3847832911338,13.7234635722027));
#26470=CARTESIAN_POINT('Ctrl Pts',(-14.4958152498884,46.4949950272598,14.4776794959001));
#26471=CARTESIAN_POINT('Ctrl Pts',(-15.6323880534542,49.6052067633858,15.2318954195974));
#26472=CARTESIAN_POINT('Ctrl Pts',(-16.7689608570199,52.7154184995118,14.4776794959001));
#26473=CARTESIAN_POINT('Ctrl Pts',(-9.50149509066497,36.5850719698906,0.));
#26474=CARTESIAN_POINT('Ctrl Pts',(-9.70710072786808,36.5247007077103,3.24562220582793));
#26475=CARTESIAN_POINT('Ctrl Pts',(-10.3094485465013,37.8155092299557,6.16982677025168));
#26476=CARTESIAN_POINT('Ctrl Pts',(-10.9117963651345,39.1063177522011,9.09403133467541));
#26477=CARTESIAN_POINT('Ctrl Pts',(-11.8323067104422,41.4806883314342,11.1176436806954));
#26478=CARTESIAN_POINT('Ctrl Pts',(-12.7528170557497,43.8550589106673,13.1412560267153));
#26479=CARTESIAN_POINT('Ctrl Pts',(-13.8498942825608,46.830761065047,13.8634749112255));
#26480=CARTESIAN_POINT('Ctrl Pts',(-14.9469715093718,49.8064632194267,14.5856937957357));
#26481=CARTESIAN_POINT('Ctrl Pts',(-16.0440487361828,52.7821653738064,13.8634749112255));
#26482=CARTESIAN_POINT('',(-10.5170715742812,35.817874106401,1.04083408558608E-14));
#26483=CARTESIAN_POINT('Origin',(-11.0241949492049,37.5449600575354,1.04083408558608E-14));
#26484=CARTESIAN_POINT('Origin',(-11.0241949492049,37.5449600575354,1.04083408558608E-14));
#26485=CARTESIAN_POINT('Ctrl Pts',(-4.19818497005511,37.5648924257372,0.));
#26486=CARTESIAN_POINT('Ctrl Pts',(-4.41028956474387,37.5343963889644,3.24562220582793));
#26487=CARTESIAN_POINT('Ctrl Pts',(-4.82280514501214,38.8977893740386,6.16982677025167));
#26488=CARTESIAN_POINT('Ctrl Pts',(-5.23532072528038,40.2611823591128,9.09403133467542));
#26489=CARTESIAN_POINT('Ctrl Pts',(-5.80855343755468,42.7423875503303,11.1176436806954));
#26490=CARTESIAN_POINT('Ctrl Pts',(-6.38178614982895,45.2235927415478,13.1412560267153));
#26491=CARTESIAN_POINT('Ctrl Pts',(-7.04421014147575,48.325136906711,13.8634749112255));
#26492=CARTESIAN_POINT('Ctrl Pts',(-7.70663413312253,51.4266810718742,14.5856937957357));
#26493=CARTESIAN_POINT('Ctrl Pts',(-8.36905812476932,54.5282252370374,13.8634749112255));
#26494=CARTESIAN_POINT('Ctrl Pts',(-4.22575906238214,39.9362279852005,0.));
#26495=CARTESIAN_POINT('Ctrl Pts',(-4.43786365707092,39.9057319484276,2.70899372698069));
#26496=CARTESIAN_POINT('Ctrl Pts',(-4.81724345149735,41.0386604807592,5.14971273833323));
#26497=CARTESIAN_POINT('Ctrl Pts',(-5.19662324592377,42.1715890130907,7.59043174968577));
#26498=CARTESIAN_POINT('Ctrl Pts',(-5.71014733528412,44.2375116101495,9.27946171175751));
#26499=CARTESIAN_POINT('Ctrl Pts',(-6.22367142464447,46.3034342072084,10.9684916738293));
#26500=CARTESIAN_POINT('Ctrl Pts',(-6.81163998135152,48.8871294476768,11.5712994880388));
#26501=CARTESIAN_POINT('Ctrl Pts',(-7.39960853805857,51.4708246881453,12.1741073022483));
#26502=CARTESIAN_POINT('Ctrl Pts',(-7.98757709476562,54.0545199286138,11.5712994880388));
#26503=CARTESIAN_POINT('Ctrl Pts',(-3.79017222552514,42.2673772240309,0.));
#26504=CARTESIAN_POINT('Ctrl Pts',(-4.00227682021391,42.2368811872581,2.19648874705823));
#26505=CARTESIAN_POINT('Ctrl Pts',(-4.35001040888163,43.1497055238908,4.17545672685568));
#26506=CARTESIAN_POINT('Ctrl Pts',(-4.69774399754935,44.0625298605236,6.15442470665314));
#26507=CARTESIAN_POINT('Ctrl Pts',(-5.15424359455804,45.7318384015438,7.5239130403414));
#26508=CARTESIAN_POINT('Ctrl Pts',(-5.61074319156672,47.401146942564,8.89340137402968));
#26509=CARTESIAN_POINT('Ctrl Pts',(-6.12760336939892,49.4902725446046,9.38216610144961));
#26510=CARTESIAN_POINT('Ctrl Pts',(-6.64446354723112,51.5793981466453,9.87093082886954));
#26511=CARTESIAN_POINT('Ctrl Pts',(-7.1613237250633,53.668523748686,9.38216610144961));
#26512=CARTESIAN_POINT('Ctrl Pts',(-2.90816428999254,44.4687528548128,0.));
#26513=CARTESIAN_POINT('Ctrl Pts',(-3.12026888468131,44.4382568180399,1.72780310113343));
#26514=CARTESIAN_POINT('Ctrl Pts',(-3.43906202795212,45.149795935654,3.28449990511991));
#26515=CARTESIAN_POINT('Ctrl Pts',(-3.75785517122293,45.8613350532681,4.84119670910639));
#26516=CARTESIAN_POINT('Ctrl Pts',(-4.16220588757996,47.1679401624789,5.91846432228298));
#26517=CARTESIAN_POINT('Ctrl Pts',(-4.56655660393696,48.4745452716896,6.99573193545957));
#26518=CARTESIAN_POINT('Ctrl Pts',(-5.0183881912398,50.1113870920656,7.3802042952164));
#26519=CARTESIAN_POINT('Ctrl Pts',(-5.47021977854266,51.7482289124415,7.76467665497322));
#26520=CARTESIAN_POINT('Ctrl Pts',(-5.9220513658455,53.3850707328175,7.38020429521639));
#26521=CARTESIAN_POINT('',(-4.19818497005564,37.5648924257619,1.57948538796959E-9));
#26522=CARTESIAN_POINT('Origin',(13.8005982420127,37.7741838134884,0.));
#26523=CARTESIAN_POINT('Ctrl Pts',(-4.19818497026072,37.5648924257933,3.13104705197686E-9));
#26524=CARTESIAN_POINT('Ctrl Pts',(-4.21419845373604,37.562590034511,0.245038153335374));
#26525=CARTESIAN_POINT('Ctrl Pts',(-4.23125516411437,37.5665407070749,0.490791160521525));
#26526=CARTESIAN_POINT('Ctrl Pts',(-4.24933641208181,37.5768338592308,0.736766500725089));
#26527=CARTESIAN_POINT('Ctrl Pts',(-4.26735830032762,37.5870932195462,0.981934317700738));
#26528=CARTESIAN_POINT('Ctrl Pts',(-4.28639799775355,37.6036535888759,1.22732257376539));
#26529=CARTESIAN_POINT('Ctrl Pts',(-4.30642834020139,37.6265535806588,1.47243294816316));
#26530=CARTESIAN_POINT('Ctrl Pts',(-4.32642851627465,37.649419084278,1.71717417802993));
#26531=CARTESIAN_POINT('Ctrl Pts',(-4.34741633416666,37.6786051816996,1.96163791541563));
#26532=CARTESIAN_POINT('Ctrl Pts',(-4.3693563568321,37.7140992541435,2.20532408778503));
#26533=CARTESIAN_POINT('Ctrl Pts',(-4.39127756261114,37.7495628850543,2.44880126242043));
#26534=CARTESIAN_POINT('Ctrl Pts',(-4.41414930860342,37.7913236642408,2.69150175431026));
#26535=CARTESIAN_POINT('Ctrl Pts',(-4.43792826156026,37.8393176800295,2.93292951866782));
#26536=CARTESIAN_POINT('Ctrl Pts',(-4.46170223991271,37.8873016553743,3.17430677585565));
#26537=CARTESIAN_POINT('Ctrl Pts',(-4.48638300400801,37.9415161845174,3.4144113931832));
#26538=CARTESIAN_POINT('Ctrl Pts',(-4.51191981196198,38.0018467100927,3.65275710614614));
#26539=CARTESIAN_POINT('Ctrl Pts',(-4.53748904614673,38.0622538424056,3.89140546668764));
#26540=CARTESIAN_POINT('Ctrl Pts',(-4.56391644980485,38.1287923820568,4.1282900208114));
#26541=CARTESIAN_POINT('Ctrl Pts',(-4.59114431677095,38.2012980447013,4.36293874377783));
#26542=CARTESIAN_POINT('Ctrl Pts',(-4.61839996701919,38.2738776920353,4.59782690201414));
#26543=CARTESIAN_POINT('Ctrl Pts',(-4.64645765641973,38.3524364483671,4.83047425894916));
#26544=CARTESIAN_POINT('Ctrl Pts',(-4.67525353711703,38.4367626436465,5.06042975959379));
#26545=CARTESIAN_POINT('Ctrl Pts',(-4.70413360568184,38.5213353756661,5.29105755998255));
#26546=CARTESIAN_POINT('Ctrl Pts',(-4.73375612398288,38.6117090746817,5.5189773630564));
#26547=CARTESIAN_POINT('Ctrl Pts',(-4.76405160819203,38.7076263878302,5.74376259354286));
#26548=CARTESIAN_POINT('Ctrl Pts',(-4.78336890979181,38.7687861188957,5.88709234072589));
#26549=CARTESIAN_POINT('Ctrl Pts',(-4.80295972078426,38.8321988522325,6.02914825314178));
#26550=CARTESIAN_POINT('Ctrl Pts',(-4.82280514501204,38.8977893740739,6.16982677023483));
#26551=CARTESIAN_POINT('Ctrl Pts',(-4.85392335399607,39.0006372418043,6.39041482339097));
#26552=CARTESIAN_POINT('Ctrl Pts',(-4.88603794597525,39.1094140363897,6.60890054011818));
#26553=CARTESIAN_POINT('Ctrl Pts',(-4.91909873852106,39.2239895821647,6.82480412008061));
#26554=CARTESIAN_POINT('Ctrl Pts',(-4.95208489447207,39.3383064672143,7.04022028559306));
#26555=CARTESIAN_POINT('Ctrl Pts',(-4.986012944267,39.458395867156,7.25306552029644));
#26556=CARTESIAN_POINT('Ctrl Pts',(-5.02082444100466,39.5840789463379,7.46287566269419));
#26557=CARTESIAN_POINT('Ctrl Pts',(-5.05557994659247,39.7095598756332,7.67234834441872));
#26558=CARTESIAN_POINT('Ctrl Pts',(-5.09121600950109,39.8406163594388,7.87879526533008));
#26559=CARTESIAN_POINT('Ctrl Pts',(-5.12766654724752,39.9770226972829,8.08177334612164));
#26560=CARTESIAN_POINT('Ctrl Pts',(-5.16408210939133,40.1132981483374,8.2845566621406));
#26561=CARTESIAN_POINT('Ctrl Pts',(-5.20131052440292,40.2549129874358,8.48387739272784));
#26562=CARTESIAN_POINT('Ctrl Pts',(-5.23927881325894,40.4015971043833,8.67931873611006));
#26563=CARTESIAN_POINT('Ctrl Pts',(-5.27724892828921,40.5482882764489,8.87476947970389));
#26564=CARTESIAN_POINT('Ctrl Pts',(-5.31595892053002,40.700048957382,9.0663400953271));
#26565=CARTESIAN_POINT('Ctrl Pts',(-5.3553296654895,40.8565673625284,9.25364450340851));
#26566=CARTESIAN_POINT('Ctrl Pts',(-5.39471485321827,41.0131431849073,9.44101762226374));
#26567=CARTESIAN_POINT('Ctrl Pts',(-5.434761203403,41.174479914544,9.62412107874923));
#26568=CARTESIAN_POINT('Ctrl Pts',(-5.47538443899858,41.3402280007153,9.80260437466025));
#26569=CARTESIAN_POINT('Ctrl Pts',(-5.51607393950566,41.5062464563465,9.98137881379592));
#26570=CARTESIAN_POINT('Ctrl Pts',(-5.55734212879153,41.6766903238779,10.1555177270917));
#26571=CARTESIAN_POINT('Ctrl Pts',(-5.59910040291772,41.8511757273801,10.3247095747702));
#26572=CARTESIAN_POINT('Ctrl Pts',(-5.61116995762818,41.9016079151995,10.3736117457735));
#26573=CARTESIAN_POINT('Ctrl Pts',(-5.62328043365746,41.952377546254,10.4221009095722));
#26574=CARTESIAN_POINT('Ctrl Pts',(-5.63542964579449,42.0034749115207,10.4701702229062));
#26575=CARTESIAN_POINT('Ctrl Pts',(-9.73793223897099,43.4867804707271,0.));
#26576=CARTESIAN_POINT('Ctrl Pts',(-9.95003683365976,43.4562844339543,1.72780310113343));
#26577=CARTESIAN_POINT('Ctrl Pts',(-10.2688299769306,44.1678235515684,3.28449990511991));
#26578=CARTESIAN_POINT('Ctrl Pts',(-10.5876231202014,44.8793626691825,4.84119670910639));
#26579=CARTESIAN_POINT('Ctrl Pts',(-10.9919738365584,46.1859677783933,5.91846432228298));
#26580=CARTESIAN_POINT('Ctrl Pts',(-11.3963245529154,47.492572887604,6.99573193545957));
#26581=CARTESIAN_POINT('Ctrl Pts',(-11.8481561402183,49.1294147079799,7.3802042952164));
#26582=CARTESIAN_POINT('Ctrl Pts',(-12.2999877275211,50.7662565283559,7.76467665497323));
#26583=CARTESIAN_POINT('Ctrl Pts',(-12.751819314824,52.4030983487319,7.3802042952164));
#26584=CARTESIAN_POINT('Ctrl Pts',(-8.27145263712669,41.6230663715378,0.));
#26585=CARTESIAN_POINT('Ctrl Pts',(-8.48355723181546,41.5925703347649,2.19648874705823));
#26586=CARTESIAN_POINT('Ctrl Pts',(-8.83129082048318,42.5053946713977,4.17545672685569));
#26587=CARTESIAN_POINT('Ctrl Pts',(-9.1790244091509,43.4182190080304,6.15442470665315));
#26588=CARTESIAN_POINT('Ctrl Pts',(-9.6355240061596,45.0875275490506,7.52391304034141));
#26589=CARTESIAN_POINT('Ctrl Pts',(-10.0920236031683,46.7568360900709,8.89340137402968));
#26590=CARTESIAN_POINT('Ctrl Pts',(-10.6088837810005,48.8459616921115,9.38216610144962));
#26591=CARTESIAN_POINT('Ctrl Pts',(-11.1257439588327,50.9350872941522,9.87093082886955));
#26592=CARTESIAN_POINT('Ctrl Pts',(-11.6426041366649,53.0242128961928,9.38216610144962));
#26593=CARTESIAN_POINT('Ctrl Pts',(-7.1967494923288,39.5090640497074,0.));
#26594=CARTESIAN_POINT('Ctrl Pts',(-7.40885408701757,39.4785680129345,2.70899372698069));
#26595=CARTESIAN_POINT('Ctrl Pts',(-7.78823388144401,40.6114965452661,5.14971273833323));
#26596=CARTESIAN_POINT('Ctrl Pts',(-8.16761367587042,41.7444250775976,7.59043174968577));
#26597=CARTESIAN_POINT('Ctrl Pts',(-8.68113776523077,43.8103476746564,9.27946171175751));
#26598=CARTESIAN_POINT('Ctrl Pts',(-9.19466185459112,45.8762702717153,10.9684916738292));
#26599=CARTESIAN_POINT('Ctrl Pts',(-9.78263041129817,48.4599655121837,11.5712994880388));
#26600=CARTESIAN_POINT('Ctrl Pts',(-10.3705989680052,51.0436607526522,12.1741073022483));
#26601=CARTESIAN_POINT('Ctrl Pts',(-10.9585675247123,53.6273559931207,11.5712994880388));
#26602=CARTESIAN_POINT('Ctrl Pts',(-6.55512420987382,37.2260157227863,1.04083408558608E-14));
#26603=CARTESIAN_POINT('Ctrl Pts',(-6.76722880456258,37.1955196860134,3.24562220582793));
#26604=CARTESIAN_POINT('Ctrl Pts',(-7.17974438483085,38.5589126710877,6.16982677025168));
#26605=CARTESIAN_POINT('Ctrl Pts',(-7.5922599650991,39.9223056561619,9.09403133467541));
#26606=CARTESIAN_POINT('Ctrl Pts',(-8.16549267737338,42.4035108473794,11.1176436806954));
#26607=CARTESIAN_POINT('Ctrl Pts',(-8.73872538964765,44.8847160385968,13.1412560267153));
#26608=CARTESIAN_POINT('Ctrl Pts',(-9.40114938129445,47.9862602037601,13.8634749112255));
#26609=CARTESIAN_POINT('Ctrl Pts',(-10.0635733729412,51.0878043689232,14.5856937957357));
#26610=CARTESIAN_POINT('Ctrl Pts',(-10.725997364588,54.1893485340865,13.8634749112255));
#26611=CARTESIAN_POINT('',(-6.55512420987382,37.2260157227863,1.04083408558608E-14));
#26612=CARTESIAN_POINT('Ctrl Pts',(-6.55512420987382,37.2260157227863,1.04083408558608E-14));
#26613=CARTESIAN_POINT('Ctrl Pts',(-6.76722880456259,37.1955196860134,3.24562220582793));
#26614=CARTESIAN_POINT('Ctrl Pts',(-7.17974438483084,38.5589126710876,6.16982677025168));
#26615=CARTESIAN_POINT('Ctrl Pts',(-7.52412807936677,39.6971249853932,8.61106394926976));
#26616=CARTESIAN_POINT('Ctrl Pts',(-7.98700482807814,41.6420486840549,10.4489096280657));
#26617=CARTESIAN_POINT('Origin',(-23.8837944332596,32.3559861244013,0.));
#26618=CARTESIAN_POINT('Ctrl Pts',(-6.55512420987382,37.2260157227863,1.04083408558608E-14));
#26619=CARTESIAN_POINT('Ctrl Pts',(-6.76722880456258,37.1955196860134,3.24562220582793));
#26620=CARTESIAN_POINT('Ctrl Pts',(-7.17974438483084,38.5589126710876,6.16982677025167));
#26621=CARTESIAN_POINT('Ctrl Pts',(-7.59225996509909,39.9223056561619,9.09403133467541));
#26622=CARTESIAN_POINT('Ctrl Pts',(-8.16549267737337,42.4035108473794,11.1176436806954));
#26623=CARTESIAN_POINT('Ctrl Pts',(-8.73872538964765,44.8847160385968,13.1412560267153));
#26624=CARTESIAN_POINT('Ctrl Pts',(-9.40114938129445,47.9862602037601,13.8634749112255));
#26625=CARTESIAN_POINT('Ctrl Pts',(-10.0635733729412,51.0878043689232,14.5856937957357));
#26626=CARTESIAN_POINT('Ctrl Pts',(-10.725997364588,54.1893485340865,13.8634749112255));
#26627=CARTESIAN_POINT('Ctrl Pts',(-5.75838408981604,36.7040912252865,0.));
#26628=CARTESIAN_POINT('Ctrl Pts',(-5.97048868450482,36.6735951885138,3.38941559469372));
#26629=CARTESIAN_POINT('Ctrl Pts',(-6.39188323248862,38.0987427505052,6.44317352589573));
#26630=CARTESIAN_POINT('Ctrl Pts',(-6.81327778047242,39.5238903124967,9.49693145709775));
#26631=CARTESIAN_POINT('Ctrl Pts',(-7.40250983972833,42.1163734062201,11.6101975146502));
#26632=CARTESIAN_POINT('Ctrl Pts',(-7.99174189898427,44.7088564999435,13.7234635722027));
#26633=CARTESIAN_POINT('Ctrl Pts',(-8.67411674998994,47.949161939876,14.4776794959001));
#26634=CARTESIAN_POINT('Ctrl Pts',(-9.35649160099562,51.1894673798086,15.2318954195974));
#26635=CARTESIAN_POINT('Ctrl Pts',(-10.0388664520013,54.4297728197411,14.4776794959001));
#26636=CARTESIAN_POINT('Ctrl Pts',(-4.81560839388856,36.8396419064669,0.));
#26637=CARTESIAN_POINT('Ctrl Pts',(-5.02771298857735,36.8091458696941,3.38941559469373));
#26638=CARTESIAN_POINT('Ctrl Pts',(-5.44910753656113,38.2342934316856,6.44317352589574));
#26639=CARTESIAN_POINT('Ctrl Pts',(-5.87050208454493,39.6594409936771,9.49693145709774));
#26640=CARTESIAN_POINT('Ctrl Pts',(-6.45973414380086,42.2519240874005,11.6101975146502));
#26641=CARTESIAN_POINT('Ctrl Pts',(-7.04896620305677,44.8444071811238,13.7234635722027));
#26642=CARTESIAN_POINT('Ctrl Pts',(-7.73134105406246,48.0847126210563,14.4776794959001));
#26643=CARTESIAN_POINT('Ctrl Pts',(-8.41371590506814,51.3250180609889,15.2318954195974));
#26644=CARTESIAN_POINT('Ctrl Pts',(-9.09609075607382,54.5653235009214,14.4776794959001));
#26645=CARTESIAN_POINT('Ctrl Pts',(-4.19818497005511,37.5648924257372,0.));
#26646=CARTESIAN_POINT('Ctrl Pts',(-4.41028956474389,37.5343963889644,3.24562220582793));
#26647=CARTESIAN_POINT('Ctrl Pts',(-4.82280514501214,38.8977893740386,6.16982677025167));
#26648=CARTESIAN_POINT('Ctrl Pts',(-5.2353207252804,40.2611823591128,9.09403133467541));
#26649=CARTESIAN_POINT('Ctrl Pts',(-5.80855343755469,42.7423875503303,11.1176436806954));
#26650=CARTESIAN_POINT('Ctrl Pts',(-6.38178614982895,45.2235927415478,13.1412560267153));
#26651=CARTESIAN_POINT('Ctrl Pts',(-7.04421014147574,48.325136906711,13.8634749112255));
#26652=CARTESIAN_POINT('Ctrl Pts',(-7.70663413312253,51.4266810718742,14.5856937957357));
#26653=CARTESIAN_POINT('Ctrl Pts',(-8.36905812476932,54.5282252370374,13.8634749112255));
#26654=CARTESIAN_POINT('',(-5.31260798925235,36.9500351333131,-1.58737143836679E-29));
#26655=CARTESIAN_POINT('Origin',(-5.56877962163339,38.731713020801,0.));
#26656=CARTESIAN_POINT('Origin',(-5.56877962163339,38.731713020801,0.));
#26657=CARTESIAN_POINT('Ctrl Pts',(1.19058808997905,37.78,0.));
#26658=CARTESIAN_POINT('Ctrl Pts',(0.976302375693351,37.7800000000001,3.24562220582793));
#26659=CARTESIAN_POINT('Ctrl Pts',(0.762016661407626,39.1882226984276,6.16982677025168));
#26660=CARTESIAN_POINT('Ctrl Pts',(0.547730947121928,40.5964453968553,9.09403133467541));
#26661=CARTESIAN_POINT('Ctrl Pts',(0.333445232836203,43.1339750175689,11.1176436806954));
#26662=CARTESIAN_POINT('Ctrl Pts',(0.119159518550494,45.6715046382825,13.1412560267153));
#26663=CARTESIAN_POINT('Ctrl Pts',(-0.095126195735231,48.8357523191413,
13.8634749112255));
#26664=CARTESIAN_POINT('Ctrl Pts',(-0.309411910020934,52.0000000000001,
14.5856937957357));
#26665=CARTESIAN_POINT('Ctrl Pts',(-0.523697624306645,55.1642476808589,
13.8634749112255));
#26666=CARTESIAN_POINT('Ctrl Pts',(1.50077089879005,40.1311229851416,0.));
#26667=CARTESIAN_POINT('Ctrl Pts',(1.28648518450433,40.1311229851416,2.7089937269807));
#26668=CARTESIAN_POINT('Ctrl Pts',(1.07219947021862,41.30651131265,5.14971273833323));
#26669=CARTESIAN_POINT('Ctrl Pts',(0.857913755932912,42.4818996401584,7.59043174968578));
#26670=CARTESIAN_POINT('Ctrl Pts',(0.643628041647182,44.5998762217203,9.27946171175751));
#26671=CARTESIAN_POINT('Ctrl Pts',(0.429342327361475,46.7178528032822,10.9684916738293));
#26672=CARTESIAN_POINT('Ctrl Pts',(0.215056613075752,49.3589264016411,11.5712994880388));
#26673=CARTESIAN_POINT('Ctrl Pts',(0.000770898790061796,52.0000000000001,
12.1741073022483));
#26674=CARTESIAN_POINT('Ctrl Pts',(-0.213514815495672,54.641073598359,11.5712994880388));
#26675=CARTESIAN_POINT('Ctrl Pts',(2.26368121662724,42.3765540157191,0.));
#26676=CARTESIAN_POINT('Ctrl Pts',(2.04939550234153,42.3765540157191,2.19648874705824));
#26677=CARTESIAN_POINT('Ctrl Pts',(1.83510978805581,43.3295747662223,4.17545672685568));
#26678=CARTESIAN_POINT('Ctrl Pts',(1.62082407377009,44.2825955167256,6.15442470665314));
#26679=CARTESIAN_POINT('Ctrl Pts',(1.40653835948437,45.9998795700625,7.5239130403414));
#26680=CARTESIAN_POINT('Ctrl Pts',(1.19225264519867,47.7171636233994,8.89340137402968));
#26681=CARTESIAN_POINT('Ctrl Pts',(0.97796693091297,49.8585818116997,9.3821661014496));
#26682=CARTESIAN_POINT('Ctrl Pts',(0.763681216627241,52.0000000000001,9.87093082886954));
#26683=CARTESIAN_POINT('Ctrl Pts',(0.549395502341525,54.1414181883004,9.3821661014496));
#26684=CARTESIAN_POINT('Ctrl Pts',(3.44999999999997,44.4300000000001,0.));
#26685=CARTESIAN_POINT('Ctrl Pts',(3.23571428571429,44.43,1.72780310113342));
#26686=CARTESIAN_POINT('Ctrl Pts',(3.02142857142856,45.1796656699788,3.28449990511991));
#26687=CARTESIAN_POINT('Ctrl Pts',(2.80714285714285,45.9293313399575,4.84119670910638));
#26688=CARTESIAN_POINT('Ctrl Pts',(2.59285714285713,47.2801821999295,5.91846432228297));
#26689=CARTESIAN_POINT('Ctrl Pts',(2.37857142857142,48.6310330599015,6.99573193545956));
#26690=CARTESIAN_POINT('Ctrl Pts',(2.16428571428571,50.3155165299508,7.38020429521639));
#26691=CARTESIAN_POINT('Ctrl Pts',(1.95,52.0000000000001,7.76467665497322));
#26692=CARTESIAN_POINT('Ctrl Pts',(1.73571428571429,53.6844834700494,7.38020429521638));
#26693=CARTESIAN_POINT('',(1.19058808997418,37.780000000016,1.57947905961937E-9));
#26694=CARTESIAN_POINT('Origin',(19.0359549110502,35.425667181256,0.));
#26695=CARTESIAN_POINT('Ctrl Pts',(1.19058808978352,37.7800000000849,3.13103292922399E-9));
#26696=CARTESIAN_POINT('Ctrl Pts',(1.17440993603746,37.7800000001371,0.245038153335428));
#26697=CARTESIAN_POINT('Ctrl Pts',(1.15808907770404,37.7863378835296,0.490791160521648));
#26698=CARTESIAN_POINT('Ctrl Pts',(1.14165673905428,37.7990994961183,0.73676650072528));
#26699=CARTESIAN_POINT('Ctrl Pts',(1.12527834684947,37.8118192130496,0.981934317700951));
#26700=CARTESIAN_POINT('Ctrl Pts',(1.10878923237326,37.8309206531575,1.22732257376562));
#26701=CARTESIAN_POINT('Ctrl Pts',(1.09222177855721,37.8564381709892,1.47243294816341));
#26702=CARTESIAN_POINT('Ctrl Pts',(1.0756792758881,37.8819172585741,1.7171741780302));
#26703=CARTESIAN_POINT('Ctrl Pts',(1.05905869845468,37.9137931615159,1.96163791541591));
#26704=CARTESIAN_POINT('Ctrl Pts',(1.0423933267646,37.952048346258,2.20532408778532));
#26705=CARTESIAN_POINT('Ctrl Pts',(1.02574224815027,37.9902707213956,2.44880126242073));
#26706=CARTESIAN_POINT('Ctrl Pts',(1.00904648208995,38.034861424896,2.69150175431056));
#26707=CARTESIAN_POINT('Ctrl Pts',(0.992339825182841,38.0857510286499,2.93292951866814));
#26708=CARTESIAN_POINT('Ctrl Pts',(0.97563666334167,38.1366299861973,3.17430677585596));
#26709=CARTESIAN_POINT('Ctrl Pts',(0.958922645785205,38.1938051285552,3.4144113931835));
#26710=CARTESIAN_POINT('Ctrl Pts',(0.942231694705361,38.2571558430637,3.65275710614643));
#26711=CARTESIAN_POINT('Ctrl Pts',(0.925519549722483,38.3205869992973,3.89140546668797));
#26712=CARTESIAN_POINT('Ctrl Pts',(0.908830560437842,38.3902092842331,4.12829002081175));
#26713=CARTESIAN_POINT('Ctrl Pts',(0.892198465551259,38.4658518732603,4.36293874377821));
#26714=CARTESIAN_POINT('Ctrl Pts',(0.875549399295395,38.5415716478927,4.59782690201461));
#26715=CARTESIAN_POINT('Ctrl Pts',(0.858957373419405,38.6233238148868,4.83047425894972));
#26716=CARTESIAN_POINT('Ctrl Pts',(0.842455462110767,38.7108897721911,5.06042975959445));
#26717=CARTESIAN_POINT('Ctrl Pts',(0.825905305682021,38.7987117380296,5.29105755998316));
#26718=CARTESIAN_POINT('Ctrl Pts',(0.809445820264702,38.8923812869986,5.51897736305698));
#26719=CARTESIAN_POINT('Ctrl Pts',(0.793109157310668,38.9916337971362,5.74376259354339));
#26720=CARTESIAN_POINT('Ctrl Pts',(0.78269241522336,39.0549201489775,5.88709234072624));
#26721=CARTESIAN_POINT('Ctrl Pts',(0.7723255833285,39.1204754952205,6.02914825314194));
#26722=CARTESIAN_POINT('Ctrl Pts',(0.762016661412751,39.1882226984626,6.16982677023482));
#26723=CARTESIAN_POINT('Ctrl Pts',(0.745851968590237,39.2944523060728,6.39041482339095));
#26724=CARTESIAN_POINT('Ctrl Pts',(0.729544808781299,39.4066922926963,6.60890054011817));
#26725=CARTESIAN_POINT('Ctrl Pts',(0.713126327700918,39.524806665964,6.8248041200806));
#26726=CARTESIAN_POINT('Ctrl Pts',(0.696744912263108,39.6426543894045,7.04022028559308));
#26727=CARTESIAN_POINT('Ctrl Pts',(0.680252704625916,39.7663499173289,7.2530655202965));
#26728=CARTESIAN_POINT('Ctrl Pts',(0.663682105818481,39.8957079165131,7.46287566269427));
#26729=CARTESIAN_POINT('Ctrl Pts',(0.647138159323281,40.0248578550338,7.67234834441905));
#26730=CARTESIAN_POINT('Ctrl Pts',(0.63051610244954,40.1596519133317,7.87879526533066));
#26731=CARTESIAN_POINT('Ctrl Pts',(0.61384922452975,40.2998572837229,8.08177334612246));
#26732=CARTESIAN_POINT('Ctrl Pts',(0.597198339079101,40.4399281220157,8.28455666214133));
#26733=CARTESIAN_POINT('Ctrl Pts',(0.580502748576783,40.5853996821053,8.4838773927285));
#26734=CARTESIAN_POINT('Ctrl Pts',(0.563796248536221,40.7359942171314,8.67931873611065));
#26735=CARTESIAN_POINT('Ctrl Pts',(0.547088944957196,40.8865959953563,8.87476947970448));
#26736=CARTESIAN_POINT('Ctrl Pts',(0.530370761385448,41.0423209776637,9.06634009532769));
#26737=CARTESIAN_POINT('Ctrl Pts',(0.513675645356928,41.2028492923282,9.2536445034091));
#26738=CARTESIAN_POINT('Ctrl Pts',(0.496974404889857,41.3634364952207,9.4410176222641));
#26739=CARTESIAN_POINT('Ctrl Pts',(0.480296279393738,41.5288302394279,9.62412107874937));
#26740=CARTESIAN_POINT('Ctrl Pts',(0.463674941840256,41.6986725382748,9.80260437466018));
#26741=CARTESIAN_POINT('Ctrl Pts',(0.447026491442446,41.8687918850905,9.98137881379588));
#26742=CARTESIAN_POINT('Ctrl Pts',(0.430435044262104,42.0433739554943,10.1555177270917));
#26743=CARTESIAN_POINT('Ctrl Pts',(0.413933671136519,42.2220261712049,10.3247095747702));
#26744=CARTESIAN_POINT('Ctrl Pts',(0.409164215743436,42.2736627087962,10.3736117457734));
#26745=CARTESIAN_POINT('Ctrl Pts',(0.40440227873099,42.3256390786478,10.4221009095721));
#26746=CARTESIAN_POINT('Ctrl Pts',(0.399648641329916,42.3779453595728,10.4701702229061));
#26747=CARTESIAN_POINT('Ctrl Pts',(-3.45000000000002,44.43,0.));
#26748=CARTESIAN_POINT('Ctrl Pts',(-3.66428571428572,44.43,1.72780310113343));
#26749=CARTESIAN_POINT('Ctrl Pts',(-3.87857142857143,45.1796656699787,3.28449990511991));
#26750=CARTESIAN_POINT('Ctrl Pts',(-4.09285714285714,45.9293313399575,4.84119670910638));
#26751=CARTESIAN_POINT('Ctrl Pts',(-4.30714285714287,47.2801821999295,5.91846432228298));
#26752=CARTESIAN_POINT('Ctrl Pts',(-4.52142857142858,48.6310330599015,6.99573193545957));
#26753=CARTESIAN_POINT('Ctrl Pts',(-4.73571428571429,50.3155165299508,7.38020429521639));
#26754=CARTESIAN_POINT('Ctrl Pts',(-4.95000000000001,52.0000000000001,7.76467665497321));
#26755=CARTESIAN_POINT('Ctrl Pts',(-5.16428571428572,53.6844834700494,7.38020429521639));
#26756=CARTESIAN_POINT('Ctrl Pts',(-2.26368121662727,42.3765540157191,0.));
#26757=CARTESIAN_POINT('Ctrl Pts',(-2.47796693091298,42.3765540157191,2.19648874705824));
#26758=CARTESIAN_POINT('Ctrl Pts',(-2.6922526451987,43.3295747662223,4.17545672685568));
#26759=CARTESIAN_POINT('Ctrl Pts',(-2.90653835948441,44.2825955167256,6.15442470665314));
#26760=CARTESIAN_POINT('Ctrl Pts',(-3.12082407377012,45.9998795700625,7.5239130403414));
#26761=CARTESIAN_POINT('Ctrl Pts',(-3.33510978805584,47.7171636233994,8.89340137402967));
#26762=CARTESIAN_POINT('Ctrl Pts',(-3.54939550234154,49.8585818116997,9.38216610144961));
#26763=CARTESIAN_POINT('Ctrl Pts',(-3.76368121662726,52.0000000000001,9.87093082886954));
#26764=CARTESIAN_POINT('Ctrl Pts',(-3.97796693091297,54.1414181883004,9.3821661014496));
#26765=CARTESIAN_POINT('Ctrl Pts',(-1.50077089879007,40.1311229851416,0.));
#26766=CARTESIAN_POINT('Ctrl Pts',(-1.71505661307578,40.1311229851416,2.70899372698069));
#26767=CARTESIAN_POINT('Ctrl Pts',(-1.9293423273615,41.30651131265,5.14971273833323));
#26768=CARTESIAN_POINT('Ctrl Pts',(-2.14362804164721,42.4818996401584,7.59043174968578));
#26769=CARTESIAN_POINT('Ctrl Pts',(-2.35791375593293,44.5998762217203,9.27946171175751));
#26770=CARTESIAN_POINT('Ctrl Pts',(-2.57219947021866,46.7178528032822,10.9684916738293));
#26771=CARTESIAN_POINT('Ctrl Pts',(-2.78648518450437,49.3589264016411,11.5712994880388));
#26772=CARTESIAN_POINT('Ctrl Pts',(-3.00077089879007,52.0000000000001,12.1741073022483));
#26773=CARTESIAN_POINT('Ctrl Pts',(-3.21505661307579,54.641073598359,11.5712994880388));
#26774=CARTESIAN_POINT('Ctrl Pts',(-1.19058808997908,37.7800000000001,0.));
#26775=CARTESIAN_POINT('Ctrl Pts',(-1.40487380426479,37.7800000000001,3.24562220582792));
#26776=CARTESIAN_POINT('Ctrl Pts',(-1.61915951855051,39.1882226984277,6.16982677025167));
#26777=CARTESIAN_POINT('Ctrl Pts',(-1.83344523283622,40.5964453968552,9.09403133467541));
#26778=CARTESIAN_POINT('Ctrl Pts',(-2.04773094712195,43.1339750175689,11.1176436806954));
#26779=CARTESIAN_POINT('Ctrl Pts',(-2.26201666140765,45.6715046382825,13.1412560267153));
#26780=CARTESIAN_POINT('Ctrl Pts',(-2.47630237569339,48.8357523191413,13.8634749112255));
#26781=CARTESIAN_POINT('Ctrl Pts',(-2.69058808997909,52.0000000000001,14.5856937957357));
#26782=CARTESIAN_POINT('Ctrl Pts',(-2.90487380426479,55.1642476808589,13.8634749112255));
#26783=CARTESIAN_POINT('',(-1.19058808997908,37.7800000000001,0.));
#26784=CARTESIAN_POINT('Ctrl Pts',(-1.19058808997908,37.7800000000001,0.));
#26785=CARTESIAN_POINT('Ctrl Pts',(-1.40487380426479,37.7800000000001,3.24562220582792));
#26786=CARTESIAN_POINT('Ctrl Pts',(-1.61915951855051,39.1882226984277,6.16982677025167));
#26787=CARTESIAN_POINT('Ctrl Pts',(-1.79805338220529,40.363860562332,8.61106394926976));
#26788=CARTESIAN_POINT('Ctrl Pts',(-1.97942721139903,42.3548619717231,10.4489096280657));
#26789=CARTESIAN_POINT('Origin',(-19.0359549110502,35.425667181256,0.));
#26790=CARTESIAN_POINT('Ctrl Pts',(-1.19058808997907,37.7800000000001,0.));
#26791=CARTESIAN_POINT('Ctrl Pts',(-1.40487380426479,37.7800000000001,3.24562220582792));
#26792=CARTESIAN_POINT('Ctrl Pts',(-1.61915951855051,39.1882226984277,6.16982677025167));
#26793=CARTESIAN_POINT('Ctrl Pts',(-1.83344523283622,40.5964453968552,9.09403133467541));
#26794=CARTESIAN_POINT('Ctrl Pts',(-2.04773094712195,43.1339750175689,11.1176436806954));
#26795=CARTESIAN_POINT('Ctrl Pts',(-2.26201666140765,45.6715046382825,13.1412560267153));
#26796=CARTESIAN_POINT('Ctrl Pts',(-2.47630237569337,48.8357523191413,13.8634749112255));
#26797=CARTESIAN_POINT('Ctrl Pts',(-2.69058808997909,52.0000000000001,14.5856937957357));
#26798=CARTESIAN_POINT('Ctrl Pts',(-2.90487380426479,55.1642476808589,13.8634749112255));
#26799=CARTESIAN_POINT('Ctrl Pts',(-0.476235235991634,37.15,0.));
#26800=CARTESIAN_POINT('Ctrl Pts',(-0.690520950277348,37.15,3.38941559469372));
#26801=CARTESIAN_POINT('Ctrl Pts',(-0.904806664563067,38.6206123116491,
6.44317352589574));
#26802=CARTESIAN_POINT('Ctrl Pts',(-1.11909237884878,40.0912246232982,9.49693145709776));
#26803=CARTESIAN_POINT('Ctrl Pts',(-1.33337809313449,42.7411764423978,11.6101975146502));
#26804=CARTESIAN_POINT('Ctrl Pts',(-1.54766380742021,45.3911282614975,13.7234635722027));
#26805=CARTESIAN_POINT('Ctrl Pts',(-1.76194952170592,48.6955641307488,14.4776794959001));
#26806=CARTESIAN_POINT('Ctrl Pts',(-1.97623523599165,52.0000000000001,15.2318954195974));
#26807=CARTESIAN_POINT('Ctrl Pts',(-2.19052095027734,55.3044358692513,14.4776794959001));
#26808=CARTESIAN_POINT('Ctrl Pts',(0.476235235991609,37.15,0.));
#26809=CARTESIAN_POINT('Ctrl Pts',(0.261949521705892,37.15,3.38941559469373));
#26810=CARTESIAN_POINT('Ctrl Pts',(0.0476638074201876,38.6206123116491,
6.44317352589573));
#26811=CARTESIAN_POINT('Ctrl Pts',(-0.166621906865532,40.0912246232982,
9.49693145709774));
#26812=CARTESIAN_POINT('Ctrl Pts',(-0.38090762115124,42.7411764423979,11.6101975146502));
#26813=CARTESIAN_POINT('Ctrl Pts',(-0.595193335436943,45.3911282614975,
13.7234635722027));
#26814=CARTESIAN_POINT('Ctrl Pts',(-0.809479049722658,48.6955641307488,
14.4776794959001));
#26815=CARTESIAN_POINT('Ctrl Pts',(-1.02376476400838,52.0000000000001,15.2318954195974));
#26816=CARTESIAN_POINT('Ctrl Pts',(-1.23805047829409,55.3044358692513,14.4776794959001));
#26817=CARTESIAN_POINT('Ctrl Pts',(1.19058808997905,37.7800000000001,0.));
#26818=CARTESIAN_POINT('Ctrl Pts',(0.976302375693353,37.7800000000001,3.24562220582793));
#26819=CARTESIAN_POINT('Ctrl Pts',(0.762016661407622,39.1882226984276,6.16982677025167));
#26820=CARTESIAN_POINT('Ctrl Pts',(0.547730947121925,40.5964453968553,9.09403133467541));
#26821=CARTESIAN_POINT('Ctrl Pts',(0.333445232836203,43.1339750175689,11.1176436806954));
#26822=CARTESIAN_POINT('Ctrl Pts',(0.119159518550494,45.6715046382825,13.1412560267153));
#26823=CARTESIAN_POINT('Ctrl Pts',(-0.095126195735231,48.8357523191413,
13.8634749112255));
#26824=CARTESIAN_POINT('Ctrl Pts',(-0.309411910020934,52.0000000000001,
14.5856937957357));
#26825=CARTESIAN_POINT('Ctrl Pts',(-0.523697624306645,55.1642476808589,
13.8634749112255));
#26826=CARTESIAN_POINT('',(4.974042353288E-6,37.3300000000069,-1.41995316083721E-29));
#26827=CARTESIAN_POINT('Origin',(-1.04083408558608E-14,39.13,0.));
#26828=CARTESIAN_POINT('Origin',(-1.04083408558608E-14,39.13,0.));
#26829=CARTESIAN_POINT('Ctrl Pts',(6.55512420987434,37.2260157227862,0.));
#26830=CARTESIAN_POINT('Ctrl Pts',(6.34301961518558,37.256511759559,3.24562220582793));
#26831=CARTESIAN_POINT('Ctrl Pts',(6.33132600607631,38.6808968181789,6.16982677025168));
#26832=CARTESIAN_POINT('Ctrl Pts',(6.31963239696705,40.1052818767988,9.09403133467542));
#26833=CARTESIAN_POINT('Ctrl Pts',(6.46865591986383,42.647479141562,11.1176436806954));
#26834=CARTESIAN_POINT('Ctrl Pts',(6.61767944276062,45.1896764063252,13.1412560267153));
#26835=CARTESIAN_POINT('Ctrl Pts',(6.8558942450299,48.3522126450341,13.8634749112255));
#26836=CARTESIAN_POINT('Ctrl Pts',(7.09410904729919,51.514748883743,14.5856937957357));
#26837=CARTESIAN_POINT('Ctrl Pts',(7.33232384956847,54.6772851224519,13.8634749112255));
#26838=CARTESIAN_POINT('Ctrl Pts',(7.19674949232937,39.5090640497073,0.));
#26839=CARTESIAN_POINT('Ctrl Pts',(6.98464489764059,39.5395600864802,2.7089937269807));
#26840=CARTESIAN_POINT('Ctrl Pts',(6.93981550268949,40.7334806923574,5.14971273833323));
#26841=CARTESIAN_POINT('Ctrl Pts',(6.8949861077384,41.9274012982346,7.59043174968578));
#26842=CARTESIAN_POINT('Ctrl Pts',(6.98430100772122,44.0543159688391,9.27946171175751));
#26843=CARTESIAN_POINT('Ctrl Pts',(7.07361590770406,46.1812306394436,10.9684916738293));
#26844=CARTESIAN_POINT('Ctrl Pts',(7.23737527503361,48.8259179534577,11.5712994880388));
#26845=CARTESIAN_POINT('Ctrl Pts',(7.40113464236316,51.4706052674719,12.1741073022483));
#26846=CARTESIAN_POINT('Ctrl Pts',(7.5648940096927,54.1152925814861,11.5712994880388));
#26847=CARTESIAN_POINT('Ctrl Pts',(8.27145263712728,41.6230663715376,0.));
#26848=CARTESIAN_POINT('Ctrl Pts',(8.0593480424385,41.6535624083105,2.19648874705824));
#26849=CARTESIAN_POINT('Ctrl Pts',(7.98287244172871,42.6273788184889,4.17545672685568));
#26850=CARTESIAN_POINT('Ctrl Pts',(7.90639684101889,43.6011952286674,6.15442470665314));
#26851=CARTESIAN_POINT('Ctrl Pts',(7.93868724865007,45.3314958432333,7.5239130403414));
#26852=CARTESIAN_POINT('Ctrl Pts',(7.97097765628125,47.0617964577992,8.89340137402968));
#26853=CARTESIAN_POINT('Ctrl Pts',(8.06362864473592,49.2119141333855,9.38216610144961));
#26854=CARTESIAN_POINT('Ctrl Pts',(8.1562796331906,51.3620318089719,9.87093082886954));
#26855=CARTESIAN_POINT('Ctrl Pts',(8.24893062164529,53.5121494845582,9.38216610144961));
#26856=CARTESIAN_POINT('Ctrl Pts',(9.7379322389716,43.486780470727,1.04083408558608E-14));
#26857=CARTESIAN_POINT('Ctrl Pts',(9.52582764428285,43.5172765074998,1.72780310113343));
#26858=CARTESIAN_POINT('Ctrl Pts',(9.42041159817612,44.2898076986596,3.28449990511991));
#26859=CARTESIAN_POINT('Ctrl Pts',(9.31499555206944,45.0623388898195,4.84119670910639));
#26860=CARTESIAN_POINT('Ctrl Pts',(9.2951370790489,46.4299360725759,5.91846432228298));
#26861=CARTESIAN_POINT('Ctrl Pts',(9.27527860602838,47.7975332553323,6.99573193545956));
#26862=CARTESIAN_POINT('Ctrl Pts',(9.30290100395372,49.495367149254,7.38020429521639));
#26863=CARTESIAN_POINT('Ctrl Pts',(9.33052340187904,51.1932010431756,7.76467665497322));
#26864=CARTESIAN_POINT('Ctrl Pts',(9.35814579980438,52.8910349370973,7.38020429521639));
#26865=CARTESIAN_POINT('',(6.55512420987177,37.2260157228026,1.57948610458898E-9));
#26866=CARTESIAN_POINT('Origin',(23.88379443326,32.355986124401,0.));
#26867=CARTESIAN_POINT('Ctrl Pts',(6.55512420969287,37.2260157228979,3.13104631369862E-9));
#26868=CARTESIAN_POINT('Ctrl Pts',(6.5391107262324,37.2283181142835,0.245038153335441));
#26869=CARTESIAN_POINT('Ctrl Pts',(6.52385796555408,37.2369141874758,0.490791160521659));
#26870=CARTESIAN_POINT('Ctrl Pts',(6.50940905124996,37.2518844708665,0.736766500725291));
#26871=CARTESIAN_POINT('Ctrl Pts',(6.49500757192006,37.2668056076575,0.981934317700964));
#26872=CARTESIAN_POINT('Ctrl Pts',(6.48140471121363,37.2880592683071,1.22732257376564));
#26873=CARTESIAN_POINT('Ctrl Pts',(6.46863741161248,37.3156748491109,1.47243294816343));
#26874=CARTESIAN_POINT('Ctrl Pts',(6.45588933999723,37.343248839914,1.71717417803015));
#26875=CARTESIAN_POINT('Ctrl Pts',(6.44397435004916,37.3771656469145,1.9616379154158));
#26876=CARTESIAN_POINT('Ctrl Pts',(6.43292288824308,37.4174031787121,2.20532408778515));
#26877=CARTESIAN_POINT('Ctrl Pts',(6.4218809047363,37.457606200743,2.44880126242052));
#26878=CARTESIAN_POINT('Ctrl Pts',(6.41170099625834,37.5041190904231,2.69150175431031));
#26879=CARTESIAN_POINT('Ctrl Pts',(6.40240673475756,37.5568683165633,2.93292951866785));
#26880=CARTESIAN_POINT('Ctrl Pts',(6.39311441763482,37.6096065074603,3.17430677585579));
#26881=CARTESIAN_POINT('Ctrl Pts',(6.38470739581538,37.6685783420143,3.41441139318347));
#26882=CARTESIAN_POINT('Ctrl Pts',(6.37720208124093,37.7336596075968,3.65275710614652));
#26883=CARTESIAN_POINT('Ctrl Pts',(6.36968723653793,37.7988235123306,3.89140546668802));
#26884=CARTESIAN_POINT('Ctrl Pts',(6.36307640132153,37.8701122336038,4.12829002081177));
#26885=CARTESIAN_POINT('Ctrl Pts',(6.35737866000337,37.9473518840362,4.3629387437782));
#26886=CARTESIAN_POINT('Ctrl Pts',(6.35167510471693,38.0246703497133,4.59782690201454));
#26887=CARTESIAN_POINT('Ctrl Pts',(6.34688650816488,38.1079516890035,4.83047425894959));
#26888=CARTESIAN_POINT('Ctrl Pts',(6.34301449757158,38.1969748179611,5.06042975959426));
#26889=CARTESIAN_POINT('Ctrl Pts',(6.33913116673708,38.2862582156518,5.291057559983));
#26890=CARTESIAN_POINT('Ctrl Pts',(6.33616978186134,38.3813167726778,5.51897736305682));
#26891=CARTESIAN_POINT('Ctrl Pts',(6.33412450750911,38.4818839849188,5.74376259354325));
#26892=CARTESIAN_POINT('Ctrl Pts',(6.33282037976375,38.5460086299152,5.88709234072615));
#26893=CARTESIAN_POINT('Ctrl Pts',(6.33188856576836,38.612372071261,6.0291482531419));
#26894=CARTESIAN_POINT('Ctrl Pts',(6.33132600608635,38.6808968182128,6.16982677023484));
#26895=CARTESIAN_POINT('Ctrl Pts',(6.33044389595609,38.7883456372327,6.39041482339094));
#26896=CARTESIAN_POINT('Ctrl Pts',(6.33027613506514,38.90176393344,6.60890054011813));
#26897=CARTESIAN_POINT('Ctrl Pts',(6.330834198378,39.0210126661743,6.82480412008054));
#26898=CARTESIAN_POINT('Ctrl Pts',(6.33139100183161,39.1399921882013,7.04022028559307));
#26899=CARTESIAN_POINT('Ctrl Pts',(6.33267037014005,39.2647757598683,7.25306552029654));
#26900=CARTESIAN_POINT('Ctrl Pts',(6.33467799886891,39.3951753232291,7.46287566269436));
#26901=CARTESIAN_POINT('Ctrl Pts',(6.3366823985082,39.5253651506641,7.67234834441888));
#26902=CARTESIAN_POINT('Ctrl Pts',(6.33941272481327,39.6611527651411,7.87879526533023));
#26903=CARTESIAN_POINT('Ctrl Pts',(6.34286879629131,39.8023029910567,8.08177334612178));
#26904=CARTESIAN_POINT('Ctrl Pts',(6.3463215515444,39.9433177782513,8.28455666214088));
#26905=CARTESIAN_POINT('Ctrl Pts',(6.35049865962787,40.0896846778742,8.48387739272826));
#26906=CARTESIAN_POINT('Ctrl Pts',(6.35539404456602,40.2411239605247,8.67931873611061));
#26907=CARTESIAN_POINT('Ctrl Pts',(6.36028966495923,40.3925705270039,8.87476947970449));
#26908=CARTESIAN_POINT('Ctrl Pts',(6.3659036240628,40.5490896991196,9.06634009532774));
#26909=CARTESIAN_POINT('Ctrl Pts',(6.37222400138285,40.7103600297412,9.25364450340919));
#26910=CARTESIAN_POINT('Ctrl Pts',(6.37854669727095,40.871689520792,9.44101762226431));
#26911=CARTESIAN_POINT('Ctrl Pts',(6.38557631500277,41.037773339894,9.62412107874969));
#26912=CARTESIAN_POINT('Ctrl Pts',(6.39329523799196,41.2082523519969,9.80260437466061));
#26913=CARTESIAN_POINT('Ctrl Pts',(6.40102675214335,41.3790094506796,9.98137881379614));
#26914=CARTESIAN_POINT('Ctrl Pts',(6.40944980108734,41.5541757364553,10.1555177270918));
#26915=CARTESIAN_POINT('Ctrl Pts',(6.41854124933317,41.7333579204527,10.3247095747701));
#26916=CARTESIAN_POINT('Ctrl Pts',(6.42116898561529,41.7851476368179,10.3736117457734));
#26917=CARTESIAN_POINT('Ctrl Pts',(6.42385252692496,41.8372726564641,10.4221009095722));
#26918=CARTESIAN_POINT('Ctrl Pts',(6.42659123460897,41.8897230480066,10.4701702229062));
#26919=CARTESIAN_POINT('Ctrl Pts',(2.90816428999319,44.4687528548127,0.));
#26920=CARTESIAN_POINT('Ctrl Pts',(2.69605969530443,44.4992488915856,1.72780310113343));
#26921=CARTESIAN_POINT('Ctrl Pts',(2.5906436491977,45.2717800827453,3.28449990511991));
#26922=CARTESIAN_POINT('Ctrl Pts',(2.48522760309099,46.0443112739052,4.84119670910639));
#26923=CARTESIAN_POINT('Ctrl Pts',(2.46536913007047,47.4119084566616,5.91846432228298));
#26924=CARTESIAN_POINT('Ctrl Pts',(2.44551065704996,48.7795056394181,6.99573193545957));
#26925=CARTESIAN_POINT('Ctrl Pts',(2.47313305497529,50.4773395333397,7.38020429521639));
#26926=CARTESIAN_POINT('Ctrl Pts',(2.50075545290062,52.1751734272613,7.76467665497322));
#26927=CARTESIAN_POINT('Ctrl Pts',(2.52837785082596,53.873007321183,7.3802042952164));
#26928=CARTESIAN_POINT('Ctrl Pts',(3.79017222552573,42.2673772240308,0.));
#26929=CARTESIAN_POINT('Ctrl Pts',(3.57806763083696,42.2978732608037,2.19648874705823));
#26930=CARTESIAN_POINT('Ctrl Pts',(3.50159203012716,43.2716896709821,4.17545672685568));
#26931=CARTESIAN_POINT('Ctrl Pts',(3.42511642941735,44.2455060811606,6.15442470665314));
#26932=CARTESIAN_POINT('Ctrl Pts',(3.45740683704852,45.9758066957265,7.5239130403414));
#26933=CARTESIAN_POINT('Ctrl Pts',(3.48969724467969,47.7061073102924,8.89340137402968));
#26934=CARTESIAN_POINT('Ctrl Pts',(3.58234823313438,49.8562249858787,9.38216610144961));
#26935=CARTESIAN_POINT('Ctrl Pts',(3.67499922158908,52.006342661465,9.87093082886954));
#26936=CARTESIAN_POINT('Ctrl Pts',(3.76765021004374,54.1564603370514,9.38216610144961));
#26937=CARTESIAN_POINT('Ctrl Pts',(4.22575906238271,39.9362279852004,0.));
#26938=CARTESIAN_POINT('Ctrl Pts',(4.01365446769395,39.9667240219733,2.7089937269807));
#26939=CARTESIAN_POINT('Ctrl Pts',(3.96882507274284,41.1606446278505,5.14971273833323));
#26940=CARTESIAN_POINT('Ctrl Pts',(3.92399567779176,42.3545652337277,7.59043174968578));
#26941=CARTESIAN_POINT('Ctrl Pts',(4.01331057777458,44.4814799043322,9.27946171175752));
#26942=CARTESIAN_POINT('Ctrl Pts',(4.10262547775741,46.6083945749368,10.9684916738293));
#26943=CARTESIAN_POINT('Ctrl Pts',(4.26638484508696,49.2530818889509,11.5712994880388));
#26944=CARTESIAN_POINT('Ctrl Pts',(4.43014421241652,51.8977692029651,12.1741073022483));
#26945=CARTESIAN_POINT('Ctrl Pts',(4.59390357974606,54.5424565169792,11.5712994880388));
#26946=CARTESIAN_POINT('Ctrl Pts',(4.19818497005566,37.5648924257371,0.));
#26947=CARTESIAN_POINT('Ctrl Pts',(3.98608037536688,37.59538846251,3.24562220582792));
#26948=CARTESIAN_POINT('Ctrl Pts',(3.97438676625761,39.0197735211299,6.16982677025168));
#26949=CARTESIAN_POINT('Ctrl Pts',(3.96269315714836,40.4441585797498,9.09403133467541));
#26950=CARTESIAN_POINT('Ctrl Pts',(4.11171668004512,42.986355844513,11.1176436806954));
#26951=CARTESIAN_POINT('Ctrl Pts',(4.26074020294192,45.5285531092761,13.1412560267153));
#26952=CARTESIAN_POINT('Ctrl Pts',(4.49895500521119,48.6910893479851,13.8634749112255));
#26953=CARTESIAN_POINT('Ctrl Pts',(4.73716980748048,51.853625586694,14.5856937957357));
#26954=CARTESIAN_POINT('Ctrl Pts',(4.97538460974978,55.0161618254029,13.8634749112255));
#26955=CARTESIAN_POINT('',(4.19818497005567,37.5648924257371,0.));
#26956=CARTESIAN_POINT('Ctrl Pts',(4.19818497005567,37.5648924257371,0.));
#26957=CARTESIAN_POINT('Ctrl Pts',(3.98608037536688,37.59538846251,3.24562220582792));
#26958=CARTESIAN_POINT('Ctrl Pts',(3.97438676625761,39.0197735211299,6.16982677025168));
#26959=CARTESIAN_POINT('Ctrl Pts',(3.96462449666071,40.2089043379837,8.61106394926976));
#26960=CARTESIAN_POINT('Ctrl Pts',(4.06844583510807,42.2054524109828,10.4489096280657));
#26961=CARTESIAN_POINT('Origin',(-13.8005982420121,37.7741838134886,0.));
#26962=CARTESIAN_POINT('Ctrl Pts',(4.19818497005566,37.5648924257371,0.));
#26963=CARTESIAN_POINT('Ctrl Pts',(3.98608037536688,37.59538846251,3.24562220582792));
#26964=CARTESIAN_POINT('Ctrl Pts',(3.97438676625761,39.0197735211299,6.16982677025168));
#26965=CARTESIAN_POINT('Ctrl Pts',(3.96269315714836,40.4441585797498,9.09403133467541));
#26966=CARTESIAN_POINT('Ctrl Pts',(4.11171668004512,42.986355844513,11.1176436806954));
#26967=CARTESIAN_POINT('Ctrl Pts',(4.26074020294192,45.5285531092761,13.1412560267153));
#26968=CARTESIAN_POINT('Ctrl Pts',(4.49895500521119,48.6910893479851,13.8634749112255));
#26969=CARTESIAN_POINT('Ctrl Pts',(4.73716980748048,51.853625586694,14.5856937957357));
#26970=CARTESIAN_POINT('Ctrl Pts',(4.97538460974978,55.0161618254029,13.8634749112255));
#26971=CARTESIAN_POINT('Ctrl Pts',(4.81560839388908,36.8396419064669,6.24500451351651E-15));
#26972=CARTESIAN_POINT('Ctrl Pts',(4.60350379920032,36.8701379432397,3.38941559469373));
#26973=CARTESIAN_POINT('Ctrl Pts',(4.60068915780659,38.3562775787769,6.44317352589574));
#26974=CARTESIAN_POINT('Ctrl Pts',(4.59787451641287,39.8424172143141,9.49693145709774));
#26975=CARTESIAN_POINT('Ctrl Pts',(4.7628973862913,42.4958923815831,11.6101975146502));
#26976=CARTESIAN_POINT('Ctrl Pts',(4.92792025616971,45.1493675488522,13.7234635722027));
#26977=CARTESIAN_POINT('Ctrl Pts',(5.18608591779791,48.4506650623305,14.4776794959001));
#26978=CARTESIAN_POINT('Ctrl Pts',(5.4442515794261,51.7519625758087,15.2318954195974));
#26979=CARTESIAN_POINT('Ctrl Pts',(5.70241724105428,55.0532600892868,14.4776794959001));
#26980=CARTESIAN_POINT('Ctrl Pts',(5.75838408981657,36.7040912252865,0.));
#26981=CARTESIAN_POINT('Ctrl Pts',(5.54627949512779,36.7345872620593,3.38941559469373));
#26982=CARTESIAN_POINT('Ctrl Pts',(5.54346485373408,38.2207268975965,6.44317352589574));
#26983=CARTESIAN_POINT('Ctrl Pts',(5.54065021234035,39.7068665331337,9.49693145709774));
#26984=CARTESIAN_POINT('Ctrl Pts',(5.70567308221878,42.3603417004028,11.6101975146502));
#26985=CARTESIAN_POINT('Ctrl Pts',(5.87069595209718,45.0138168676718,13.7234635722027));
#26986=CARTESIAN_POINT('Ctrl Pts',(6.12886161372538,48.31511438115,14.4776794959001));
#26987=CARTESIAN_POINT('Ctrl Pts',(6.38702727535358,51.6164118946283,15.2318954195974));
#26988=CARTESIAN_POINT('Ctrl Pts',(6.64519293698177,54.9177094081064,14.4776794959001));
#26989=CARTESIAN_POINT('Ctrl Pts',(6.55512420987434,37.2260157227862,0.));
#26990=CARTESIAN_POINT('Ctrl Pts',(6.34301961518558,37.2565117595591,3.24562220582793));
#26991=CARTESIAN_POINT('Ctrl Pts',(6.33132600607631,38.6808968181789,6.16982677025167));
#26992=CARTESIAN_POINT('Ctrl Pts',(6.31963239696705,40.1052818767988,9.09403133467541));
#26993=CARTESIAN_POINT('Ctrl Pts',(6.46865591986383,42.647479141562,11.1176436806954));
#26994=CARTESIAN_POINT('Ctrl Pts',(6.61767944276062,45.1896764063252,13.1412560267153));
#26995=CARTESIAN_POINT('Ctrl Pts',(6.85589424502988,48.3522126450341,13.8634749112255));
#26996=CARTESIAN_POINT('Ctrl Pts',(7.09410904729919,51.514748883743,14.5856937957357));
#26997=CARTESIAN_POINT('Ctrl Pts',(7.33232384956847,54.6772851224519,13.8634749112255));
#26998=CARTESIAN_POINT('',(5.3126178361619,36.9500337175413,-1.22362873180948E-29));
#26999=CARTESIAN_POINT('Origin',(5.56877962163395,38.7317130208009,0.));
#27000=CARTESIAN_POINT('Origin',(5.56877962163395,38.7317130208009,0.));
#27001=CARTESIAN_POINT('Ctrl Pts',(11.7862169042735,35.9142171164209,0.));
#27002=CARTESIAN_POINT('Ctrl Pts',(11.5806112670704,35.9745883786013,3.24562220582793));
#27003=CARTESIAN_POINT('Ctrl Pts',(11.7717478112975,37.3861394252072,6.16982677025168));
#27004=CARTESIAN_POINT('Ctrl Pts',(11.9628843555245,38.7976904718133,9.09403133467541));
#27005=CARTESIAN_POINT('Ctrl Pts',(12.4721834264259,41.292803575407,11.1176436806954));
#27006=CARTESIAN_POINT('Ctrl Pts',(12.9814824973274,43.7879166790007,13.1412560267153));
#27007=CARTESIAN_POINT('Ctrl Pts',(13.6673484497322,46.884361357741,13.8634749112255));
#27008=CARTESIAN_POINT('Ctrl Pts',(14.353214402137,49.9808060364812,14.5856937957357));
#27009=CARTESIAN_POINT('Ctrl Pts',(15.0390803545419,53.0772507152215,13.8634749112255));
#27010=CARTESIAN_POINT('Ctrl Pts',(12.7462230199163,38.0827145049532,0.));
#27011=CARTESIAN_POINT('Ctrl Pts',(12.5406173827132,38.1430857671335,2.70899372698069));
#27012=CARTESIAN_POINT('Ctrl Pts',(12.6661569043006,39.3312338708266,5.14971273833323));
#27013=CARTESIAN_POINT('Ctrl Pts',(12.791696425888,40.5193819745197,7.59043174968577));
#27014=CARTESIAN_POINT('Ctrl Pts',(13.1827937463386,42.6119368849887,9.27946171175751));
#27015=CARTESIAN_POINT('Ctrl Pts',(13.5738910667892,44.7044917954577,10.9684916738292));
#27016=CARTESIAN_POINT('Ctrl Pts',(14.1123618472582,47.2989546180622,11.5712994880388));
#27017=CARTESIAN_POINT('Ctrl Pts',(14.6508326277272,49.8934174406666,12.1741073022483));
#27018=CARTESIAN_POINT('Ctrl Pts',(15.1893034081961,52.4878802632711,11.5712994880388));
#27019=CARTESIAN_POINT('Ctrl Pts',(14.1108411348348,40.0222531270432,-1.05434036998093E-14));
#27020=CARTESIAN_POINT('Ctrl Pts',(13.9052354976316,40.0826243892235,2.19648874705823));
#27021=CARTESIAN_POINT('Ctrl Pts',(13.9681268331908,41.0574123652206,4.17545672685568));
#27022=CARTESIAN_POINT('Ctrl Pts',(14.0310181687499,42.0322003412176,6.15442470665314));
#27023=CARTESIAN_POINT('Ctrl Pts',(14.3092273587164,43.7402935862748,7.52391304034139));
#27024=CARTESIAN_POINT('Ctrl Pts',(14.5874365486829,45.4483868313321,8.89340137402966));
#27025=CARTESIAN_POINT('Ctrl Pts',(14.9851381329364,47.5634337987569,9.3821661014496));
#27026=CARTESIAN_POINT('Ctrl Pts',(15.38283971719,49.6784807661817,9.87093082886953));
#27027=CARTESIAN_POINT('Ctrl Pts',(15.7805413014435,51.7935277336064,9.3821661014496));
#27028=CARTESIAN_POINT('Ctrl Pts',(15.8276282594351,41.6582954965891,0.));
#27029=CARTESIAN_POINT('Ctrl Pts',(15.622022622232,41.7186667587694,1.72780310113342));
#27030=CARTESIAN_POINT('Ctrl Pts',(15.6276222110082,42.4983369638543,3.28449990511991));
#27031=CARTESIAN_POINT('Ctrl Pts',(15.6332217997845,43.2780071689392,4.84119670910638));
#27032=CARTESIAN_POINT('Ctrl Pts',(15.8081948292727,44.6345103396637,5.91846432228297));
#27033=CARTESIAN_POINT('Ctrl Pts',(15.983167858761,45.9910135103883,6.99573193545955));
#27034=CARTESIAN_POINT('Ctrl Pts',(16.252136056532,47.6676348262506,7.38020429521638));
#27035=CARTESIAN_POINT('Ctrl Pts',(16.521104254303,49.344256142113,7.76467665497321));
#27036=CARTESIAN_POINT('Ctrl Pts',(16.790072452074,51.0208774579754,7.38020429521638));
#27037=CARTESIAN_POINT('',(11.7862169043639,35.9142171164878,1.57948960455104E-9));
#27038=CARTESIAN_POINT('Origin',(28.245428775984,28.6276304970123,0.));
#27039=CARTESIAN_POINT('Ctrl Pts',(11.7862169041098,35.9142171165574,3.13105403642851E-9));
#27040=CARTESIAN_POINT('Ctrl Pts',(11.7706940792791,35.9187750292273,0.24503815333559));
#27041=CARTESIAN_POINT('Ctrl Pts',(11.756819918478,35.9294543009582,0.490791160521951));
#27042=CARTESIAN_POINT('Ctrl Pts',(11.7446485667475,35.9463285033517,0.736766500725725));
#27043=CARTESIAN_POINT('Ctrl Pts',(11.7325171728812,35.9631473086865,0.981934317701356));
#27044=CARTESIAN_POINT('Ctrl Pts',(11.7220774809611,35.9861205266374,1.22732257376599));
#27045=CARTESIAN_POINT('Ctrl Pts',(11.7133702409769,36.0152719968249,1.47243294816374));
#27046=CARTESIAN_POINT('Ctrl Pts',(11.7046761143912,36.0443795639103,1.71717417803052));
#27047=CARTESIAN_POINT('Ctrl Pts',(11.6977092667638,36.079646826587,1.96163791541622));
#27048=CARTESIAN_POINT('Ctrl Pts',(11.6924966907343,36.1210475853283,2.20532408778562));
#27049=CARTESIAN_POINT('Ctrl Pts',(11.6872885852768,36.1624128366599,2.44880126242109));
#27050=CARTESIAN_POINT('Ctrl Pts',(11.6838317679614,36.2099010442177,2.69150175431097));
#27051=CARTESIAN_POINT('Ctrl Pts',(11.6821391062287,36.2634360706164,2.9329295186686));
#27052=CARTESIAN_POINT('Ctrl Pts',(11.6804467986042,36.3169598973807,3.17430677585645));
#27053=CARTESIAN_POINT('Ctrl Pts',(11.6805179152422,36.3765279276399,3.41441139318402));
#27054=CARTESIAN_POINT('Ctrl Pts',(11.6823510237343,36.4420148774081,3.65275710614698));
#27055=CARTESIAN_POINT('Ctrl Pts',(11.6841864598783,36.5075849814588,3.89140546668851));
#27056=CARTESIAN_POINT('Ctrl Pts',(11.6877883562711,36.579088906284,4.12829002081228));
#27057=CARTESIAN_POINT('Ctrl Pts',(11.6931409581037,36.6563532415796,4.36293874377873));
#27058=CARTESIAN_POINT('Ctrl Pts',(11.6984990217246,36.7336964173083,4.59782690201504));
#27059=CARTESIAN_POINT('Ctrl Pts',(11.7056113365131,36.8168115609901,4.83047425895006));
#27060=CARTESIAN_POINT('Ctrl Pts',(11.7144480496049,36.9054796074171,5.0604297595947));
#27061=CARTESIAN_POINT('Ctrl Pts',(11.7233105977818,36.994406884455,5.29105755998342));
#27062=CARTESIAN_POINT('Ctrl Pts',(11.7339075987038,37.0889193314433,5.51897736305724));
#27063=CARTESIAN_POINT('Ctrl Pts',(11.7461953488411,37.1887539873582,5.74376259354366));
#27064=CARTESIAN_POINT('Ctrl Pts',(11.7540303837178,37.2524115326578,5.88709234072642));
#27065=CARTESIAN_POINT('Ctrl Pts',(11.7625525566677,37.3182321008169,6.02914825314204));
#27066=CARTESIAN_POINT('Ctrl Pts',(11.7717478113122,37.3861394252393,6.16982677023484));
#27067=CARTESIAN_POINT('Ctrl Pts',(11.7861662410927,37.4926201075706,6.39041482339101));
#27068=CARTESIAN_POINT('Ctrl Pts',(11.8021412942477,37.6049078439222,6.60890054011826));
#27069=CARTESIAN_POINT('Ctrl Pts',(11.819664541394,37.7228633758097,6.82480412008072));
#27070=CARTESIAN_POINT('Ctrl Pts',(11.8371482288264,37.8405526164633,7.04022028559315));
#27071=CARTESIAN_POINT('Ctrl Pts',(11.8561731288311,37.9638839981998,7.25306552029652));
#27072=CARTESIAN_POINT('Ctrl Pts',(11.8767181155649,38.0926705666683,7.46287566269426));
#27073=CARTESIAN_POINT('Ctrl Pts',(11.8972300575422,38.221249993568,7.67234834441908));
#27074=CARTESIAN_POINT('Ctrl Pts',(11.9192571854562,38.3552669199728,7.87879526533072));
#27075=CARTESIAN_POINT('Ctrl Pts',(11.9427658506832,38.4944885898571,8.08177334612255));
#27076=CARTESIAN_POINT('Ctrl Pts',(11.9662519585,38.6335766715391,8.28455666214149));
#27077=CARTESIAN_POINT('Ctrl Pts',(11.9912167312945,38.7778593027061,8.48387739272872));
#27078=CARTESIAN_POINT('Ctrl Pts',(12.0176143452911,38.9270604659007,8.67931873611092));
#27079=CARTESIAN_POINT('Ctrl Pts',(12.0440132289432,39.0762688052766,8.8747694797048));
#27080=CARTESIAN_POINT('Ctrl Pts',(12.0718450467041,39.2303958882203,9.06634009532807));
#27081=CARTESIAN_POINT('Ctrl Pts',(12.1010522527169,39.3891252359326,9.25364450340952));
#27082=CARTESIAN_POINT('Ctrl Pts',(12.1302701731051,39.5479128119397,9.44101762226463));
#27083=CARTESIAN_POINT('Ctrl Pts',(12.1608644313196,39.7113057183257,9.62412107874999));
#27084=CARTESIAN_POINT('Ctrl Pts',(12.1927664798389,39.878950982619,9.8026043746609));
#27085=CARTESIAN_POINT('Ctrl Pts',(12.2247205672072,40.0468697110625,9.98137881379654));
#27086=CARTESIAN_POINT('Ctrl Pts',(12.2579866432891,40.2190543317699,10.1555177270923));
#27087=CARTESIAN_POINT('Ctrl Pts',(12.2924858372377,40.3951188515069,10.3247095747707));
#27088=CARTESIAN_POINT('Ctrl Pts',(12.302457272062,40.4460074573699,10.3736117457738));
#27089=CARTESIAN_POINT('Ctrl Pts',(12.3125316625314,40.4972200117264,10.4221009095723));
#27090=CARTESIAN_POINT('Ctrl Pts',(12.3227069631098,40.548746775169,10.4701702229062));
#27091=CARTESIAN_POINT('Ctrl Pts',(9.20712674149506,43.602250138795,0.));
#27092=CARTESIAN_POINT('Ctrl Pts',(9.00152110429196,43.6626214009754,1.72780310113343));
#27093=CARTESIAN_POINT('Ctrl Pts',(9.00712069306818,44.4422916060602,3.28449990511991));
#27094=CARTESIAN_POINT('Ctrl Pts',(9.01272028184443,45.2219618111451,4.84119670910638));
#27095=CARTESIAN_POINT('Ctrl Pts',(9.18769331133267,46.5784649818697,5.91846432228298));
#27096=CARTESIAN_POINT('Ctrl Pts',(9.36266634082093,47.9349681525942,6.99573193545957));
#27097=CARTESIAN_POINT('Ctrl Pts',(9.63163453859197,49.6115894684566,7.38020429521639));
#27098=CARTESIAN_POINT('Ctrl Pts',(9.90060273636299,51.2882107843189,7.76467665497321));
#27099=CARTESIAN_POINT('Ctrl Pts',(10.169570934134,52.9648321001813,7.38020429521639));
#27100=CARTESIAN_POINT('Ctrl Pts',(9.76686869112084,41.2977585211119,0.));
#27101=CARTESIAN_POINT('Ctrl Pts',(9.56126305391773,41.3581297832922,2.19648874705823));
#27102=CARTESIAN_POINT('Ctrl Pts',(9.62415438947685,42.3329177592892,4.17545672685568));
#27103=CARTESIAN_POINT('Ctrl Pts',(9.68704572503597,43.3077057352862,6.15442470665314));
#27104=CARTESIAN_POINT('Ctrl Pts',(9.96525491500249,45.0157989803435,7.5239130403414));
#27105=CARTESIAN_POINT('Ctrl Pts',(10.243464104969,46.7238922254008,8.89340137402968));
#27106=CARTESIAN_POINT('Ctrl Pts',(10.6411656892225,48.8389391928255,9.38216610144961));
#27107=CARTESIAN_POINT('Ctrl Pts',(11.038867273476,50.9539861602503,9.87093082886954));
#27108=CARTESIAN_POINT('Ctrl Pts',(11.4365688577295,53.0690331276751,9.3821661014496));
#27109=CARTESIAN_POINT('Ctrl Pts',(9.86626475512792,38.9283465500519,0.));
#27110=CARTESIAN_POINT('Ctrl Pts',(9.66065911792481,38.9887178122322,2.70899372698069));
#27111=CARTESIAN_POINT('Ctrl Pts',(9.78619863951222,40.1768659159253,5.14971273833323));
#27112=CARTESIAN_POINT('Ctrl Pts',(9.91173816109965,41.3650140196184,7.59043174968577));
#27113=CARTESIAN_POINT('Ctrl Pts',(10.3028354815503,43.4575689300874,9.27946171175752));
#27114=CARTESIAN_POINT('Ctrl Pts',(10.6939328020009,45.5501238405564,10.9684916738292));
#27115=CARTESIAN_POINT('Ctrl Pts',(11.2324035824698,48.1445866631609,11.5712994880388));
#27116=CARTESIAN_POINT('Ctrl Pts',(11.7708743629388,50.7390494857653,12.1741073022483));
#27117=CARTESIAN_POINT('Ctrl Pts',(12.3093451434078,53.3335123083698,11.5712994880388));
#27118=CARTESIAN_POINT('Ctrl Pts',(9.50149509066547,36.5850719698904,1.04083408558608E-14));
#27119=CARTESIAN_POINT('Ctrl Pts',(9.29588945346236,36.6454432320708,3.24562220582792));
#27120=CARTESIAN_POINT('Ctrl Pts',(9.48702599768942,38.0569942786768,6.16982677025167));
#27121=CARTESIAN_POINT('Ctrl Pts',(9.67816254191645,39.4685453252828,9.09403133467541));
#27122=CARTESIAN_POINT('Ctrl Pts',(10.1874616128179,41.9636584288765,11.1176436806954));
#27123=CARTESIAN_POINT('Ctrl Pts',(10.6967606837193,44.4587715324702,13.1412560267153));
#27124=CARTESIAN_POINT('Ctrl Pts',(11.3826266361241,47.5552162112105,13.8634749112255));
#27125=CARTESIAN_POINT('Ctrl Pts',(12.068492588529,50.6516608899507,14.5856937957357));
#27126=CARTESIAN_POINT('Ctrl Pts',(12.7543585409338,53.7481055686911,13.8634749112255));
#27127=CARTESIAN_POINT('',(9.50149509066547,36.5850719698904,1.04083408558608E-14));
#27128=CARTESIAN_POINT('Ctrl Pts',(9.50149509066547,36.5850719698904,1.04083408558608E-14));
#27129=CARTESIAN_POINT('Ctrl Pts',(9.29588945346237,36.6454432320708,3.24562220582792));
#27130=CARTESIAN_POINT('Ctrl Pts',(9.48702599768942,38.0569942786767,6.16982677025167));
#27131=CARTESIAN_POINT('Ctrl Pts',(9.64659405380729,39.2354107742189,8.61106394926976));
#27132=CARTESIAN_POINT('Ctrl Pts',(10.033497056841,41.196861549629,10.4489096280657));
#27133=CARTESIAN_POINT('Origin',(-8.28430119040596,39.3537269950292,0.));
#27134=CARTESIAN_POINT('Ctrl Pts',(9.50149509066549,36.5850719698904,1.04083408558608E-14));
#27135=CARTESIAN_POINT('Ctrl Pts',(9.29588945346237,36.6454432320708,3.24562220582792));
#27136=CARTESIAN_POINT('Ctrl Pts',(9.48702599768942,38.0569942786767,6.16982677025167));
#27137=CARTESIAN_POINT('Ctrl Pts',(9.67816254191646,39.4685453252828,9.09403133467541));
#27138=CARTESIAN_POINT('Ctrl Pts',(10.1874616128179,41.9636584288765,11.1176436806954));
#27139=CARTESIAN_POINT('Ctrl Pts',(10.6967606837193,44.4587715324702,13.1412560267153));
#27140=CARTESIAN_POINT('Ctrl Pts',(11.3826266361241,47.5552162112105,13.8634749112255));
#27141=CARTESIAN_POINT('Ctrl Pts',(12.068492588529,50.6516608899507,14.5856937957357));
#27142=CARTESIAN_POINT('Ctrl Pts',(12.7543585409338,53.748105568691,13.8634749112255));
#27143=CARTESIAN_POINT('Ctrl Pts',(10.0094201239378,35.7793349404724,0.));
#27144=CARTESIAN_POINT('Ctrl Pts',(9.80381448673468,35.8397062026528,3.38941559469374));
#27145=CARTESIAN_POINT('Ctrl Pts',(10.012528216215,37.3111196447713,6.44317352589574));
#27146=CARTESIAN_POINT('Ctrl Pts',(10.2212419456952,38.7825330868899,9.49693145709775));
#27147=CARTESIAN_POINT('Ctrl Pts',(10.7622140099937,41.3855144999133,11.6101975146502));
#27148=CARTESIAN_POINT('Ctrl Pts',(11.3031860742922,43.9884959129366,13.7234635722027));
#27149=CARTESIAN_POINT('Ctrl Pts',(12.0285476034518,47.2194501734233,14.4776794959001));
#27150=CARTESIAN_POINT('Ctrl Pts',(12.7539091326114,50.4504044339099,15.2318954195974));
#27151=CARTESIAN_POINT('Ctrl Pts',(13.479270661771,53.6813586943965,14.4776794959001));
#27152=CARTESIAN_POINT('Ctrl Pts',(10.923308849381,35.5109929990846,0.));
#27153=CARTESIAN_POINT('Ctrl Pts',(10.7177032121779,35.571364261265,3.38941559469374));
#27154=CARTESIAN_POINT('Ctrl Pts',(10.9264169416582,37.0427777033835,6.44317352589574));
#27155=CARTESIAN_POINT('Ctrl Pts',(11.1351306711385,38.5141911455021,9.49693145709775));
#27156=CARTESIAN_POINT('Ctrl Pts',(11.6761027354369,41.1171725585255,11.6101975146502));
#27157=CARTESIAN_POINT('Ctrl Pts',(12.2170747997354,43.7201539715489,13.7234635722027));
#27158=CARTESIAN_POINT('Ctrl Pts',(12.942436328895,46.9511082320355,14.4776794959001));
#27159=CARTESIAN_POINT('Ctrl Pts',(13.6677978580546,50.1820624925221,15.2318954195974));
#27160=CARTESIAN_POINT('Ctrl Pts',(14.3931593872142,53.4130167530087,14.4776794959001));
#27161=CARTESIAN_POINT('Ctrl Pts',(11.7862169042735,35.9142171164209,0.));
#27162=CARTESIAN_POINT('Ctrl Pts',(11.5806112670704,35.9745883786013,3.24562220582793));
#27163=CARTESIAN_POINT('Ctrl Pts',(11.7717478112975,37.3861394252072,6.16982677025168));
#27164=CARTESIAN_POINT('Ctrl Pts',(11.9628843555245,38.7976904718133,9.09403133467541));
#27165=CARTESIAN_POINT('Ctrl Pts',(12.472183426426,41.292803575407,11.1176436806954));
#27166=CARTESIAN_POINT('Ctrl Pts',(12.9814824973274,43.7879166790007,13.1412560267153));
#27167=CARTESIAN_POINT('Ctrl Pts',(13.6673484497322,46.884361357741,13.8634749112255));
#27168=CARTESIAN_POINT('Ctrl Pts',(14.353214402137,49.9808060364812,14.5856937957357));
#27169=CARTESIAN_POINT('Ctrl Pts',(15.0390803545419,53.0772507152215,13.8634749112255));
#27170=CARTESIAN_POINT('',(10.5170811194392,35.8178713036897,-1.00239475043615E-29));
#27171=CARTESIAN_POINT('Origin',(11.0241949492054,37.5449600575352,0.));
#27172=CARTESIAN_POINT('Origin',(11.0241949492054,37.5449600575352,0.));
#27173=CARTESIAN_POINT('Ctrl Pts',(16.7773762111445,33.8713086176151,0.));
#27174=CARTESIAN_POINT('Ctrl Pts',(16.5824550692829,33.9603261204012,3.24562220582793));
#27175=CARTESIAN_POINT('Ctrl Pts',(16.972530777998,35.3303080462615,6.16982677025168));
#27176=CARTESIAN_POINT('Ctrl Pts',(17.3626064867132,36.7002899721219,9.09403133467542));
#27177=CARTESIAN_POINT('Ctrl Pts',(18.221813245233,39.0975256070689,11.1176436806954));
#27178=CARTESIAN_POINT('Ctrl Pts',(19.0810200037527,41.4947612420159,13.1412560267153));
#27179=CARTESIAN_POINT('Ctrl Pts',(20.2005748533762,44.4620796765375,13.8634749112255));
#27180=CARTESIAN_POINT('Ctrl Pts',(21.3201297029997,47.4293981110592,14.5856937957357));
#27181=CARTESIAN_POINT('Ctrl Pts',(22.4396845526232,50.3967165455808,13.8634749112255));
#27182=CARTESIAN_POINT('Ctrl Pts',(18.0362202038896,35.8811107143581,0.));
#27183=CARTESIAN_POINT('Ctrl Pts',(17.8412990620279,35.9701282171442,2.7089937269807));
#27184=CARTESIAN_POINT('Ctrl Pts',(18.1346518775204,37.1283165495981,5.14971273833323));
#27185=CARTESIAN_POINT('Ctrl Pts',(18.4280046930129,38.2865048820522,7.59043174968578));
#27186=CARTESIAN_POINT('Ctrl Pts',(19.1129228203184,40.3021016488385,9.27946171175752));
#27187=CARTESIAN_POINT('Ctrl Pts',(19.797840947624,42.317698415625,10.9684916738293));
#27188=CARTESIAN_POINT('Ctrl Pts',(20.7000614289636,44.8091209655645,11.5712994880388));
#27189=CARTESIAN_POINT('Ctrl Pts',(21.6022819103031,47.300543515504,12.1741073022483));
#27190=CARTESIAN_POINT('Ctrl Pts',(22.5045023916426,49.7919660654434,11.5712994880388));
#27191=CARTESIAN_POINT('Ctrl Pts',(19.6629735993426,37.6067022235296,0.));
#27192=CARTESIAN_POINT('Ctrl Pts',(19.4680524574809,37.6957197263157,2.19648874705824));
#27193=CARTESIAN_POINT('Ctrl Pts',(19.6690304430806,38.6516353959964,4.17545672685568));
#27194=CARTESIAN_POINT('Ctrl Pts',(19.8700084286803,39.607551065677,6.15442470665314));
#27195=CARTESIAN_POINT('Ctrl Pts',(20.3884728641635,41.2586650884904,7.5239130403414));
#27196=CARTESIAN_POINT('Ctrl Pts',(20.9069372996467,42.9097791113039,8.89340137402967));
#27197=CARTESIAN_POINT('Ctrl Pts',(21.6015934223203,44.9466991136021,9.3821661014496));
#27198=CARTESIAN_POINT('Ctrl Pts',(22.2962495449939,46.9836191159003,9.87093082886954));
#27199=CARTESIAN_POINT('Ctrl Pts',(22.9909056676675,49.0205391181986,9.3821661014496));
#27200=CARTESIAN_POINT('Ctrl Pts',(21.5951194116472,38.9817677587446,0.));
#27201=CARTESIAN_POINT('Ctrl Pts',(21.4001982697855,39.0707852615307,1.72780310113343));
#27202=CARTESIAN_POINT('Ctrl Pts',(21.5166995019651,39.8417226435484,3.28449990511991));
#27203=CARTESIAN_POINT('Ctrl Pts',(21.6332007341447,40.612660025566,4.84119670910638));
#27204=CARTESIAN_POINT('Ctrl Pts',(21.9994433198419,41.9304546915348,5.91846432228298));
#27205=CARTESIAN_POINT('Ctrl Pts',(22.3656859055391,43.2482493575036,6.99573193545955));
#27206=CARTESIAN_POINT('Ctrl Pts',(22.8705244862895,44.8695269202924,7.38020429521639));
#27207=CARTESIAN_POINT('Ctrl Pts',(23.3753630670398,46.4908044830812,7.76467665497321));
#27208=CARTESIAN_POINT('Ctrl Pts',(23.8802016477901,48.1120820458699,7.38020429521639));
#27209=CARTESIAN_POINT('',(16.7773762109261,33.8713086175738,-1.21941606378243E-9));
#27210=CARTESIAN_POINT('Origin',(32.0320676419193,24.3164988679735,0.));
#27211=CARTESIAN_POINT('Ctrl Pts',(16.7773762111445,33.8713086176151,0.));
#27212=CARTESIAN_POINT('Ctrl Pts',(16.5824550692829,33.9603261204012,3.24562220582793));
#27213=CARTESIAN_POINT('Ctrl Pts',(16.972530777998,35.3303080462615,6.16982677025168));
#27214=CARTESIAN_POINT('Ctrl Pts',(17.3001355482566,36.4808862649313,8.62571762198521));
#27215=CARTESIAN_POINT('Ctrl Pts',(17.9679679135941,38.3823149509185,10.4701702229062));
#27216=CARTESIAN_POINT('Ctrl Pts',(15.3186586437011,41.8481313484577,1.04083408558608E-14));
#27217=CARTESIAN_POINT('Ctrl Pts',(15.1237375018394,41.9371488512438,1.72780310113343));
#27218=CARTESIAN_POINT('Ctrl Pts',(15.240238734019,42.7080862332614,3.28449990511991));
#27219=CARTESIAN_POINT('Ctrl Pts',(15.3567399661986,43.4790236152791,4.84119670910639));
#27220=CARTESIAN_POINT('Ctrl Pts',(15.7229825518958,44.7968182812479,5.91846432228298));
#27221=CARTESIAN_POINT('Ctrl Pts',(16.089225137593,46.1146129472167,6.99573193545957));
#27222=CARTESIAN_POINT('Ctrl Pts',(16.5940637183433,47.7358905100055,7.38020429521639));
#27223=CARTESIAN_POINT('Ctrl Pts',(17.0989022990936,49.3571680727943,7.76467665497322));
#27224=CARTESIAN_POINT('Ctrl Pts',(17.603740879844,50.978445635583,7.38020429521639));
#27225=CARTESIAN_POINT('Ctrl Pts',(15.5447398754882,39.4874365476043,0.));
#27226=CARTESIAN_POINT('Ctrl Pts',(15.3498187336265,39.5764540503904,2.19648874705824));
#27227=CARTESIAN_POINT('Ctrl Pts',(15.5507967192262,40.5323697200711,4.17545672685568));
#27228=CARTESIAN_POINT('Ctrl Pts',(15.7517747048259,41.4882853897517,6.15442470665314));
#27229=CARTESIAN_POINT('Ctrl Pts',(16.2702391403091,43.1393994125652,7.52391304034141));
#27230=CARTESIAN_POINT('Ctrl Pts',(16.7887035757923,44.7905134353786,8.89340137402968));
#27231=CARTESIAN_POINT('Ctrl Pts',(17.4833596984659,46.8274334376768,9.38216610144961));
#27232=CARTESIAN_POINT('Ctrl Pts',(18.1780158211395,48.864353439975,9.87093082886954));
#27233=CARTESIAN_POINT('Ctrl Pts',(18.8726719438131,50.9012734422733,9.38216610144961));
#27234=CARTESIAN_POINT('Ctrl Pts',(15.3059217494168,37.1279962392255,0.));
#27235=CARTESIAN_POINT('Ctrl Pts',(15.1110006075551,37.2170137420116,2.70899372698069));
#27236=CARTESIAN_POINT('Ctrl Pts',(15.4043534230476,38.3752020744656,5.14971273833323));
#27237=CARTESIAN_POINT('Ctrl Pts',(15.6977062385401,39.5333904069196,7.59043174968579));
#27238=CARTESIAN_POINT('Ctrl Pts',(16.3826243658456,41.548987173706,9.27946171175752));
#27239=CARTESIAN_POINT('Ctrl Pts',(17.0675424931512,43.5645839404925,10.9684916738293));
#27240=CARTESIAN_POINT('Ctrl Pts',(17.9697629744908,46.0560064904319,11.5712994880388));
#27241=CARTESIAN_POINT('Ctrl Pts',(18.8719834558303,48.5474290403714,12.1741073022483));
#27242=CARTESIAN_POINT('Ctrl Pts',(19.7742039371699,51.0388515903109,11.5712994880388));
#27243=CARTESIAN_POINT('Ctrl Pts',(14.6113821712786,34.8604849513722,0.));
#27244=CARTESIAN_POINT('Ctrl Pts',(14.4164610294169,34.9495024541583,3.24562220582793));
#27245=CARTESIAN_POINT('Ctrl Pts',(14.8065367381321,36.3194843800186,6.16982677025168));
#27246=CARTESIAN_POINT('Ctrl Pts',(15.1966124468473,37.689466305879,9.09403133467542));
#27247=CARTESIAN_POINT('Ctrl Pts',(16.055819205367,40.086701940826,11.1176436806954));
#27248=CARTESIAN_POINT('Ctrl Pts',(16.9150259638868,42.4839375757731,13.1412560267153));
#27249=CARTESIAN_POINT('Ctrl Pts',(18.0345808135103,45.4512560102947,13.8634749112255));
#27250=CARTESIAN_POINT('Ctrl Pts',(19.1541356631338,48.4185744448163,14.5856937957357));
#27251=CARTESIAN_POINT('Ctrl Pts',(20.2736905127572,51.3858928793379,13.8634749112255));
#27252=CARTESIAN_POINT('',(14.6113821712786,34.8604849513722,0.));
#27253=CARTESIAN_POINT('Ctrl Pts',(14.6113821712786,34.8604849513722,0.));
#27254=CARTESIAN_POINT('Ctrl Pts',(14.4164610294169,34.9495024541583,3.24562220582793));
#27255=CARTESIAN_POINT('Ctrl Pts',(14.8065367381321,36.3194843800186,6.16982677025167));
#27256=CARTESIAN_POINT('Ctrl Pts',(15.1321867744985,37.4631973926724,8.61106394926976));
#27257=CARTESIAN_POINT('Ctrl Pts',(15.7942952127128,39.3496213890631,10.4489096280657));
#27258=CARTESIAN_POINT('Origin',(-2.59935965651494,40.1321417817282,0.));
#27259=CARTESIAN_POINT('Ctrl Pts',(14.6113821712786,34.8604849513722,0.));
#27260=CARTESIAN_POINT('Ctrl Pts',(14.4164610294169,34.9495024541583,3.24562220582793));
#27261=CARTESIAN_POINT('Ctrl Pts',(14.8065367381321,36.3194843800186,6.16982677025167));
#27262=CARTESIAN_POINT('Ctrl Pts',(15.1966124468473,37.689466305879,9.09403133467541));
#27263=CARTESIAN_POINT('Ctrl Pts',(16.055819205367,40.086701940826,11.1176436806954));
#27264=CARTESIAN_POINT('Ctrl Pts',(16.9150259638868,42.483937575773,13.1412560267153));
#27265=CARTESIAN_POINT('Ctrl Pts',(18.0345808135103,45.4512560102947,13.8634749112255));
#27266=CARTESIAN_POINT('Ctrl Pts',(19.1541356631338,48.4185744448163,14.5856937957357));
#27267=CARTESIAN_POINT('Ctrl Pts',(20.2736905127572,51.3858928793379,13.8634749112255));
#27268=CARTESIAN_POINT('Ctrl Pts',(14.9994689250472,33.9906638941717,6.24500451351651E-15));
#27269=CARTESIAN_POINT('Ctrl Pts',(14.8045477831855,34.0796813969578,3.38941559469372));
#27270=CARTESIAN_POINT('Ctrl Pts',(15.2205410738882,35.5064149111822,6.44317352589573));
#27271=CARTESIAN_POINT('Ctrl Pts',(15.636534364591,36.9331484254066,9.49693145709774));
#27272=CARTESIAN_POINT('Ctrl Pts',(16.542442992115,39.4326468889937,11.6101975146502));
#27273=CARTESIAN_POINT('Ctrl Pts',(17.448351619639,41.9321453525807,13.7234635722027));
#27274=CARTESIAN_POINT('Ctrl Pts',(18.6261427473663,45.0269834486349,14.4776794959001));
#27275=CARTESIAN_POINT('Ctrl Pts',(19.8039338750935,48.1218215446891,15.2318954195974));
#27276=CARTESIAN_POINT('Ctrl Pts',(20.9817250028208,51.2166596407433,14.4776794959001));
#27277=CARTESIAN_POINT('Ctrl Pts',(15.8658665409936,33.5949933606688,0.));
#27278=CARTESIAN_POINT('Ctrl Pts',(15.6709453991319,33.684010863455,3.38941559469373));
#27279=CARTESIAN_POINT('Ctrl Pts',(16.0869386898346,35.1107443776793,6.44317352589574));
#27280=CARTESIAN_POINT('Ctrl Pts',(16.5029319805374,36.5374778919037,9.49693145709774));
#27281=CARTESIAN_POINT('Ctrl Pts',(17.4088406080614,39.0369763554908,11.6101975146502));
#27282=CARTESIAN_POINT('Ctrl Pts',(18.3147492355854,41.5364748190779,13.7234635722027));
#27283=CARTESIAN_POINT('Ctrl Pts',(19.4925403633127,44.631312915132,14.4776794959001));
#27284=CARTESIAN_POINT('Ctrl Pts',(20.6703314910399,47.7261510111863,15.2318954195974));
#27285=CARTESIAN_POINT('Ctrl Pts',(21.8481226187672,50.8209891072404,14.4776794959001));
#27286=CARTESIAN_POINT('Ctrl Pts',(16.7773762111446,33.8713086176151,0.));
#27287=CARTESIAN_POINT('Ctrl Pts',(16.5824550692829,33.9603261204012,3.24562220582793));
#27288=CARTESIAN_POINT('Ctrl Pts',(16.972530777998,35.3303080462615,6.16982677025167));
#27289=CARTESIAN_POINT('Ctrl Pts',(17.3626064867132,36.7002899721219,9.09403133467541));
#27290=CARTESIAN_POINT('Ctrl Pts',(18.221813245233,39.0975256070689,11.1176436806954));
#27291=CARTESIAN_POINT('Ctrl Pts',(19.0810200037527,41.4947612420159,13.1412560267153));
#27292=CARTESIAN_POINT('Ctrl Pts',(20.2005748533762,44.4620796765375,13.8634749112255));
#27293=CARTESIAN_POINT('Ctrl Pts',(21.3201297029997,47.4293981110591,14.5856937957357));
#27294=CARTESIAN_POINT('Ctrl Pts',(22.4396845526232,50.3967165455808,13.8634749112255));
#27295=CARTESIAN_POINT('',(15.5074469598942,33.9565603203064,-7.60754902620015E-30));
#27296=CARTESIAN_POINT('Origin',(16.2551894587641,35.5938999782222,0.));
#27297=CARTESIAN_POINT('Origin',(16.2551894587641,35.5938999782222,0.));
#27298=CARTESIAN_POINT('Ctrl Pts',(21.4269965203144,31.1388779521427,1.04083408558608E-14));
#27299=CARTESIAN_POINT('Ctrl Pts',(21.2467279061363,31.2547295558832,3.24562220582793));
#27300=CARTESIAN_POINT('Ctrl Pts',(21.8278019627956,32.5552534796889,6.16982677025168));
#27301=CARTESIAN_POINT('Ctrl Pts',(22.4088760194549,33.8557774034947,9.0940313346754));
#27302=CARTESIAN_POINT('Ctrl Pts',(23.6004994937372,36.1063347653243,11.1176436806954));
#27303=CARTESIAN_POINT('Ctrl Pts',(24.7921229680195,38.3568921271539,13.1412560267153));
#27304=CARTESIAN_POINT('Ctrl Pts',(26.322575806653,41.1346782711697,13.8634749112255));
#27305=CARTESIAN_POINT('Ctrl Pts',(27.8530286452863,43.9124644151855,14.5856937957357));
#27306=CARTESIAN_POINT('Ctrl Pts',(29.3834814839197,46.6902505592013,13.8634749112255));
#27307=CARTESIAN_POINT('Ctrl Pts',(22.9590519566757,32.9490709821973,0.));
#27308=CARTESIAN_POINT('Ctrl Pts',(22.7787833424976,33.0649225859378,2.70899372698069));
#27309=CARTESIAN_POINT('Ctrl Pts',(23.2339776345314,34.1695737726433,5.14971273833323));
#27310=CARTESIAN_POINT('Ctrl Pts',(23.6891719265652,35.2742249593487,7.59043174968578));
#27311=CARTESIAN_POINT('Ctrl Pts',(24.6539679027946,37.1718318447819,9.27946171175752));
#27312=CARTESIAN_POINT('Ctrl Pts',(25.6187638790239,39.069438730215,10.9684916738293));
#27313=CARTESIAN_POINT('Ctrl Pts',(26.866367454023,41.4071028290421,11.5712994880388));
#27314=CARTESIAN_POINT('Ctrl Pts',(28.1139710290221,43.7447669278692,12.1741073022483));
#27315=CARTESIAN_POINT('Ctrl Pts',(29.3615746040211,46.0824310266963,11.5712994880388));
#27316=CARTESIAN_POINT('Ctrl Pts',(24.8148246247012,34.4255873115186,0.));
#27317=CARTESIAN_POINT('Ctrl Pts',(24.6345560105231,34.5414389152591,2.19648874705822));
#27318=CARTESIAN_POINT('Ctrl Pts',(24.9695293139492,35.4590225922219,4.17545672685568));
#27319=CARTESIAN_POINT('Ctrl Pts',(25.3045026173754,36.3766062691846,6.15442470665313));
#27320=CARTESIAN_POINT('Ctrl Pts',(26.0526678575967,37.9371291496694,7.5239130403414));
#27321=CARTESIAN_POINT('Ctrl Pts',(26.8008330978182,39.4976520301542,8.89340137402967));
#27322=CARTESIAN_POINT('Ctrl Pts',(27.7783025634771,41.4149792500713,9.3821661014496));
#27323=CARTESIAN_POINT('Ctrl Pts',(28.755772029136,43.3323064699884,9.87093082886953));
#27324=CARTESIAN_POINT('Ctrl Pts',(29.7332414947948,45.2496336899055,9.3821661014496));
#27325=CARTESIAN_POINT('Ctrl Pts',(26.9229962078201,35.5116836434674,1.04083408558608E-14));
#27326=CARTESIAN_POINT('Ctrl Pts',(26.742727593642,35.6275352472079,1.72780310113343));
#27327=CARTESIAN_POINT('Ctrl Pts',(26.9677588400996,36.3740457442602,3.28449990511991));
#27328=CARTESIAN_POINT('Ctrl Pts',(27.1927900865572,37.1205562413125,4.84119670910639));
#27329=CARTESIAN_POINT('Ctrl Pts',(27.7428465855749,38.3728159033325,5.91846432228298));
#27330=CARTESIAN_POINT('Ctrl Pts',(28.2929030845927,39.6250755653525,6.99573193545956));
#27331=CARTESIAN_POINT('Ctrl Pts',(29.0233349906525,41.1580048392676,7.38020429521639));
#27332=CARTESIAN_POINT('Ctrl Pts',(29.7537668967123,42.6909341131828,7.76467665497322));
#27333=CARTESIAN_POINT('Ctrl Pts',(30.4841988027721,44.223863387098,7.38020429521639));
#27334=CARTESIAN_POINT('',(21.426996519931,31.1388779521943,-2.44187858986325E-9));
#27335=CARTESIAN_POINT('Origin',(35.1666259835204,19.5103534449749,0.));
#27336=CARTESIAN_POINT('Ctrl Pts',(21.4269965203144,31.1388779521427,1.04083408558608E-14));
#27337=CARTESIAN_POINT('Ctrl Pts',(21.2467279061363,31.2547295558832,3.24562220582793));
#27338=CARTESIAN_POINT('Ctrl Pts',(21.8278019627956,32.5552534796889,6.16982677025168));
#27339=CARTESIAN_POINT('Ctrl Pts',(22.3158165419708,33.6474974511925,8.62571762198519));
#27340=CARTESIAN_POINT('Ctrl Pts',(23.2474528526983,35.4345298797235,10.4701702229062));
#27341=CARTESIAN_POINT('Ctrl Pts',(21.118346831285,39.2421052839111,0.));
#27342=CARTESIAN_POINT('Ctrl Pts',(20.9380782171068,39.3579568876516,1.72780310113343));
#27343=CARTESIAN_POINT('Ctrl Pts',(21.1631094635644,40.1044673847039,3.28449990511991));
#27344=CARTESIAN_POINT('Ctrl Pts',(21.388140710022,40.8509778817562,4.84119670910638));
#27345=CARTESIAN_POINT('Ctrl Pts',(21.9381972090398,42.1032375437762,5.91846432228297));
#27346=CARTESIAN_POINT('Ctrl Pts',(22.4882537080575,43.3554972057961,6.99573193545955));
#27347=CARTESIAN_POINT('Ctrl Pts',(23.2186856141173,44.8884264797113,7.38020429521639));
#27348=CARTESIAN_POINT('Ctrl Pts',(23.9491175201772,46.4213557536265,7.76467665497322));
#27349=CARTESIAN_POINT('Ctrl Pts',(24.679549426237,47.9542850275417,7.38020429521639));
#27350=CARTESIAN_POINT('Ctrl Pts',(21.0061649833187,36.8732642383511,0.));
#27351=CARTESIAN_POINT('Ctrl Pts',(20.8258963691406,36.9891158420916,2.19648874705823));
#27352=CARTESIAN_POINT('Ctrl Pts',(21.1608696725667,37.9066995190544,4.17545672685568));
#27353=CARTESIAN_POINT('Ctrl Pts',(21.4958429759929,38.8242831960171,6.15442470665314));
#27354=CARTESIAN_POINT('Ctrl Pts',(22.2440082162142,40.3848060765019,7.5239130403414));
#27355=CARTESIAN_POINT('Ctrl Pts',(22.9921734564357,41.9453289569867,8.89340137402967));
#27356=CARTESIAN_POINT('Ctrl Pts',(23.9696429220946,43.8626561769038,9.38216610144961));
#27357=CARTESIAN_POINT('Ctrl Pts',(24.9471123877534,45.7799833968209,9.87093082886954));
#27358=CARTESIAN_POINT('Ctrl Pts',(25.9245818534123,47.697310616738,9.38216610144961));
#27359=CARTESIAN_POINT('Ctrl Pts',(20.433994315521,34.5718269932683,0.));
#27360=CARTESIAN_POINT('Ctrl Pts',(20.2537257013429,34.6876785970088,2.7089937269807));
#27361=CARTESIAN_POINT('Ctrl Pts',(20.7089199933767,35.7923297837142,5.14971273833323));
#27362=CARTESIAN_POINT('Ctrl Pts',(21.1641142854105,36.8969809704196,7.59043174968577));
#27363=CARTESIAN_POINT('Ctrl Pts',(22.1289102616398,38.7945878558528,9.27946171175751));
#27364=CARTESIAN_POINT('Ctrl Pts',(23.0937062378692,40.6921947412859,10.9684916738293));
#27365=CARTESIAN_POINT('Ctrl Pts',(24.3413098128683,43.029858840113,11.5712994880388));
#27366=CARTESIAN_POINT('Ctrl Pts',(25.5889133878673,45.3675229389401,12.1741073022483));
#27367=CARTESIAN_POINT('Ctrl Pts',(26.8365169628664,47.7051870377672,11.5712994880388));
#27368=CARTESIAN_POINT('Ctrl Pts',(19.4238236466312,32.4262389885811,0.));
#27369=CARTESIAN_POINT('Ctrl Pts',(19.243555032453,32.5420905923216,3.24562220582792));
#27370=CARTESIAN_POINT('Ctrl Pts',(19.8246290891124,33.8426145161273,6.16982677025167));
#27371=CARTESIAN_POINT('Ctrl Pts',(20.4057031457717,35.1431384399331,9.09403133467541));
#27372=CARTESIAN_POINT('Ctrl Pts',(21.597326620054,37.3936958017627,11.1176436806954));
#27373=CARTESIAN_POINT('Ctrl Pts',(22.7889500943363,39.6442531635923,13.1412560267153));
#27374=CARTESIAN_POINT('Ctrl Pts',(24.3194029329697,42.4220393076081,13.8634749112255));
#27375=CARTESIAN_POINT('Ctrl Pts',(25.8498557716031,45.1998254516239,14.5856937957357));
#27376=CARTESIAN_POINT('Ctrl Pts',(27.3803086102365,47.9776115956397,13.8634749112255));
#27377=CARTESIAN_POINT('',(19.4238236466312,32.4262389885811,0.));
#27378=CARTESIAN_POINT('Ctrl Pts',(19.4238236466312,32.4262389885811,0.));
#27379=CARTESIAN_POINT('Ctrl Pts',(19.243555032453,32.5420905923216,3.24562220582792));
#27380=CARTESIAN_POINT('Ctrl Pts',(19.8246290891124,33.8426145161273,6.16982677025167));
#27381=CARTESIAN_POINT('Ctrl Pts',(20.309731810084,34.9283413471511,8.61106394926976));
#27382=CARTESIAN_POINT('Ctrl Pts',(21.2335670650401,36.7013364119535,10.4489096280657));
#27383=CARTESIAN_POINT('Origin',(3.13849734404846,40.0935818932913,0.));
#27384=CARTESIAN_POINT('Ctrl Pts',(19.4238236466311,32.4262389885811,0.));
#27385=CARTESIAN_POINT('Ctrl Pts',(19.243555032453,32.5420905923216,3.24562220582792));
#27386=CARTESIAN_POINT('Ctrl Pts',(19.8246290891124,33.8426145161273,6.16982677025167));
#27387=CARTESIAN_POINT('Ctrl Pts',(20.4057031457717,35.1431384399331,9.09403133467541));
#27388=CARTESIAN_POINT('Ctrl Pts',(21.597326620054,37.3936958017627,11.1176436806954));
#27389=CARTESIAN_POINT('Ctrl Pts',(22.7889500943363,39.6442531635923,13.1412560267153));
#27390=CARTESIAN_POINT('Ctrl Pts',(24.3194029329697,42.4220393076081,13.8634749112255));
#27391=CARTESIAN_POINT('Ctrl Pts',(25.8498557716031,45.1998254516238,14.5856937957357));
#27392=CARTESIAN_POINT('Ctrl Pts',(27.3803086102365,47.9776115956397,13.8634749112255));
#27393=CARTESIAN_POINT('Ctrl Pts',(19.6841717937391,31.5100409519659,0.));
#27394=CARTESIAN_POINT('Ctrl Pts',(19.503903179561,31.6258925557065,3.38941559469373));
#27395=CARTESIAN_POINT('Ctrl Pts',(20.1187076077131,32.9789019620467,6.44317352589574));
#27396=CARTESIAN_POINT('Ctrl Pts',(20.7335120358652,34.331911368387,9.49693145709774));
#27397=CARTESIAN_POINT('Ctrl Pts',(21.9859155393831,36.6770443017775,11.6101975146502));
#27398=CARTESIAN_POINT('Ctrl Pts',(23.238319042901,39.022177235168,13.7234635722027));
#27399=CARTESIAN_POINT('Ctrl Pts',(24.8445633383045,41.9178971879301,14.4776794959001));
#27400=CARTESIAN_POINT('Ctrl Pts',(26.450807633708,44.8136171406923,15.2318954195974));
#27401=CARTESIAN_POINT('Ctrl Pts',(28.0570519291115,47.7093370934545,14.4776794959001));
#27402=CARTESIAN_POINT('Ctrl Pts',(20.4854409432124,30.9950965373906,0.));
#27403=CARTESIAN_POINT('Ctrl Pts',(20.3051723290343,31.1109481411311,3.38941559469372));
#27404=CARTESIAN_POINT('Ctrl Pts',(20.9199767571864,32.4639575474714,6.44317352589573));
#27405=CARTESIAN_POINT('Ctrl Pts',(21.5347811853385,33.8169669538117,9.49693145709774));
#27406=CARTESIAN_POINT('Ctrl Pts',(22.7871846888564,36.1620998872021,11.6101975146502));
#27407=CARTESIAN_POINT('Ctrl Pts',(24.0395881923743,38.5072328205926,13.7234635722027));
#27408=CARTESIAN_POINT('Ctrl Pts',(25.6458324877778,41.4029527733548,14.4776794959001));
#27409=CARTESIAN_POINT('Ctrl Pts',(27.2520767831814,44.298672726117,15.2318954195974));
#27410=CARTESIAN_POINT('Ctrl Pts',(28.8583210785848,47.1943926788791,14.4776794959001));
#27411=CARTESIAN_POINT('Ctrl Pts',(21.4269965203144,31.1388779521427,1.04083408558608E-14));
#27412=CARTESIAN_POINT('Ctrl Pts',(21.2467279061363,31.2547295558832,3.24562220582793));
#27413=CARTESIAN_POINT('Ctrl Pts',(21.8278019627956,32.555253479689,6.16982677025167));
#27414=CARTESIAN_POINT('Ctrl Pts',(22.4088760194549,33.8557774034947,9.0940313346754));
#27415=CARTESIAN_POINT('Ctrl Pts',(23.6004994937372,36.1063347653243,11.1176436806954));
#27416=CARTESIAN_POINT('Ctrl Pts',(24.7921229680195,38.3568921271539,13.1412560267153));
#27417=CARTESIAN_POINT('Ctrl Pts',(26.3225758066529,41.1346782711697,13.8634749112255));
#27418=CARTESIAN_POINT('Ctrl Pts',(27.8530286452863,43.9124644151855,14.5856937957357));
#27419=CARTESIAN_POINT('Ctrl Pts',(29.3834814839197,46.6902505592013,13.8634749112255));
#27420=CARTESIAN_POINT('',(20.182125900029,31.4039916914382,-5.03628278819837E-30));
#27421=CARTESIAN_POINT('Origin',(21.1552751870378,32.918250739684,0.));
#27422=CARTESIAN_POINT('Origin',(21.1552751870378,32.918250739684,0.));
#27423=CARTESIAN_POINT('Ctrl Pts',(25.6404249706861,27.7725495286735,0.));
#27424=CARTESIAN_POINT('Ctrl Pts',(25.4784786333245,27.9128768288047,3.24562220582793));
#27425=CARTESIAN_POINT('Ctrl Pts',(26.2387220458135,29.1174678338684,6.16982677025168));
#27426=CARTESIAN_POINT('Ctrl Pts',(26.9989654583026,30.3220588389322,9.09403133467542));
#27427=CARTESIAN_POINT('Ctrl Pts',(28.4987476307694,32.3801230698289,11.1176436806954));
#27428=CARTESIAN_POINT('Ctrl Pts',(29.9985298032362,34.4381873007258,13.1412560267153));
#27429=CARTESIAN_POINT('Ctrl Pts',(31.9087250245465,36.9698934388173,13.8634749112255));
#27430=CARTESIAN_POINT('Ctrl Pts',(33.8189202458568,39.5015995769089,14.5856937957357));
#27431=CARTESIAN_POINT('Ctrl Pts',(35.729115467167,42.0333057150005,13.8634749112255));
#27432=CARTESIAN_POINT('Ctrl Pts',(27.4145036200624,29.3462831821135,0.));
#27433=CARTESIAN_POINT('Ctrl Pts',(27.2525572827008,29.4866104822447,2.7089937269807));
#27434=CARTESIAN_POINT('Ctrl Pts',(27.860326608162,30.5152370105912,5.14971273833323));
#27435=CARTESIAN_POINT('Ctrl Pts',(28.4680959336233,31.5438635389378,7.59043174968578));
#27436=CARTESIAN_POINT('Ctrl Pts',(29.6931292949422,33.2848507390766,9.27946171175751));
#27437=CARTESIAN_POINT('Ctrl Pts',(30.9181626562612,35.0258379392154,10.9684916738292));
#27438=CARTESIAN_POINT('Ctrl Pts',(32.4857517139244,37.1621554871446,11.5712994880388));
#27439=CARTESIAN_POINT('Ctrl Pts',(34.0533407715877,39.2984730350737,12.1741073022483));
#27440=CARTESIAN_POINT('Ctrl Pts',(35.6209298292509,41.4347905830029,11.5712994880388));
#27441=CARTESIAN_POINT('Ctrl Pts',(29.4615173807458,30.543666717041,-1.05434036998093E-14));
#27442=CARTESIAN_POINT('Ctrl Pts',(29.2995710433842,30.6839940171721,2.19648874705823));
#27443=CARTESIAN_POINT('Ctrl Pts',(29.7617205741622,31.5445663438469,4.17545672685568));
#27444=CARTESIAN_POINT('Ctrl Pts',(30.2238701049403,32.4051386705216,6.15442470665314));
#27445=CARTESIAN_POINT('Ctrl Pts',(31.1865056631394,33.8433026630074,7.52391304034139));
#27446=CARTESIAN_POINT('Ctrl Pts',(32.1491412213385,35.2814666554933,8.89340137402967));
#27447=CARTESIAN_POINT('Ctrl Pts',(33.389525570451,37.0401698399469,9.3821661014496));
#27448=CARTESIAN_POINT('Ctrl Pts',(34.6299099195636,38.7988730244004,9.87093082886954));
#27449=CARTESIAN_POINT('Ctrl Pts',(35.8702942686761,40.557576208854,9.3821661014496));
#27450=CARTESIAN_POINT('Ctrl Pts',(31.7027984407115,31.3186840564482,0.));
#27451=CARTESIAN_POINT('Ctrl Pts',(31.5408521033499,31.4590113565794,1.72780310113342));
#27452=CARTESIAN_POINT('Ctrl Pts',(31.8698323768441,32.1658981677049,3.28449990511991));
#27453=CARTESIAN_POINT('Ctrl Pts',(32.1988126503383,32.8727849788304,4.84119670910639));
#27454=CARTESIAN_POINT('Ctrl Pts',(32.9214854985886,34.0340172414015,5.91846432228298));
#27455=CARTESIAN_POINT('Ctrl Pts',(33.6441583468389,35.1952495039725,6.99573193545956));
#27456=CARTESIAN_POINT('Ctrl Pts',(34.5853140909925,36.6086244696002,7.38020429521639));
#27457=CARTESIAN_POINT('Ctrl Pts',(35.526469835146,38.0219994352279,7.76467665497321));
#27458=CARTESIAN_POINT('Ctrl Pts',(36.4676255792996,39.4353744008555,7.38020429521639));
#27459=CARTESIAN_POINT('',(25.640424970796,27.7725495286968,1.57949969353625E-9));
#27460=CARTESIAN_POINT('Origin',(37.5852932322718,14.3070334890498,0.));
#27461=CARTESIAN_POINT('Ctrl Pts',(25.6404249705938,27.7725495288656,3.13107516801643E-9));
#27462=CARTESIAN_POINT('Ctrl Pts',(25.6281983378206,27.7831439665411,0.245038153335291));
#27463=CARTESIAN_POINT('Ctrl Pts',(25.6200142870521,27.7986217084842,0.490791160521329));
#27464=CARTESIAN_POINT('Ctrl Pts',(25.6159526330981,27.8190271851147,0.736766500724782));
#27465=CARTESIAN_POINT('Ctrl Pts',(25.6119043133259,27.8393656717115,0.98193431770045));
#27466=CARTESIAN_POINT('Ctrl Pts',(25.6119514551675,27.8645996505507,1.22732257376512));
#27467=CARTESIAN_POINT('Ctrl Pts',(25.6161410294536,27.8947338787561,1.47243294816291));
#27468=CARTESIAN_POINT('Ctrl Pts',(25.6203242940988,27.9248227237925,1.71717417802967));
#27469=CARTESIAN_POINT('Ctrl Pts',(25.6286375769735,27.9597970874095,1.96163791541537));
#27470=CARTESIAN_POINT('Ctrl Pts',(25.6410945477697,27.9996219245316,2.20532408778476));
#27471=CARTESIAN_POINT('Ctrl Pts',(25.6535408348301,28.039412605835,2.44880126242025));
#27472=CARTESIAN_POINT('Ctrl Pts',(25.670123717558,28.0840454126417,2.69150175431017));
#27473=CARTESIAN_POINT('Ctrl Pts',(25.690823271976,28.1334457426218,2.93292951866782));
#27474=CARTESIAN_POINT('Ctrl Pts',(25.711518496006,28.1828357379543,3.17430677585562));
#27475=CARTESIAN_POINT('Ctrl Pts',(25.7363286400399,28.2369911812591,3.41441139318315));
#27476=CARTESIAN_POINT('Ctrl Pts',(25.7652003562647,28.2957987052583,3.65275710614606));
#27477=CARTESIAN_POINT('Ctrl Pts',(25.7941087333335,28.3546809021119,3.89140546668757));
#27478=CARTESIAN_POINT('Ctrl Pts',(25.8270889373972,28.4182268780895,4.12829002081133));
#27479=CARTESIAN_POINT('Ctrl Pts',(25.8640546001339,28.4862854384143,4.36293874377776));
#27480=CARTESIAN_POINT('Ctrl Pts',(25.9010579825876,28.5544134456108,4.59782690201416));
#27481=CARTESIAN_POINT('Ctrl Pts',(25.9420548501735,28.6270630772619,4.83047425894926));
#27482=CARTESIAN_POINT('Ctrl Pts',(25.9869270447948,28.7040474659735,5.06042975959398));
#27483=CARTESIAN_POINT('Ctrl Pts',(26.0319304281239,28.7812569268608,5.29105755998273));
#27484=CARTESIAN_POINT('Ctrl Pts',(26.0808316886118,28.8628263193248,5.51897736305657));
#27485=CARTESIAN_POINT('Ctrl Pts',(26.1334818341726,28.9485346007072,5.74376259354302));
#27486=CARTESIAN_POINT('Ctrl Pts',(26.1670531325894,29.0031847495424,5.887092340726));
#27487=CARTESIAN_POINT('Ctrl Pts',(26.2021480259523,29.0595170057056,6.02914825314183));
#27488=CARTESIAN_POINT('Ctrl Pts',(26.2387220458403,29.1174678338915,6.16982677023483));
#27489=CARTESIAN_POINT('Ctrl Pts',(26.2960711849264,29.2083364372324,6.39041482339095));
#27490=CARTESIAN_POINT('Ctrl Pts',(26.3572486158602,29.3038406779897,6.60890054011815));
#27491=CARTESIAN_POINT('Ctrl Pts',(26.4221888209397,29.4038573838824,6.82480412008056));
#27492=CARTESIAN_POINT('Ctrl Pts',(26.4869824198613,29.5036482964479,7.04022028559305));
#27493=CARTESIAN_POINT('Ctrl Pts',(26.5555217851616,29.6079312382239,7.25306552029648));
#27494=CARTESIAN_POINT('Ctrl Pts',(26.6277100364536,29.7165449255437,7.46287566269426));
#27495=CARTESIAN_POINT('Ctrl Pts',(26.6997821794603,29.8249839175527,7.67234834441895));
#27496=CARTESIAN_POINT('Ctrl Pts',(26.7754914030015,29.9377396021008,7.87879526533046));
#27497=CARTESIAN_POINT('Ctrl Pts',(26.8547104088652,30.0546142350032,8.08177334612217));
#27498=CARTESIAN_POINT('Ctrl Pts',(26.9338534012421,30.1713767224897,8.28455666214139));
#27499=CARTESIAN_POINT('Ctrl Pts',(27.016499328435,30.2922500787582,8.48387739272888));
#27500=CARTESIAN_POINT('Ctrl Pts',(27.1024918458758,30.4170022653827,8.67931873611135));
#27501=CARTESIAN_POINT('Ctrl Pts',(27.1884884993292,30.5417604522572,8.87476947970517));
#27502=CARTESIAN_POINT('Ctrl Pts',(27.2778319154184,30.6703976233164,9.06634009532839));
#27503=CARTESIAN_POINT('Ctrl Pts',(27.3703382785463,30.8026498047317,9.25364450340979));
#27504=CARTESIAN_POINT('Ctrl Pts',(27.4628785767206,30.9349505015546,9.44101762226489));
#27505=CARTESIAN_POINT('Ctrl Pts',(27.5585839591973,31.0708686028433,9.62412107875024));
#27506=CARTESIAN_POINT('Ctrl Pts',(27.657245442894,31.2101115092137,9.80260437466114));
#27507=CARTESIAN_POINT('Ctrl Pts',(27.7560678639063,31.3495815496057,9.98137881379688));
#27508=CARTESIAN_POINT('Ctrl Pts',(27.8578558275202,31.4923869622811,10.1555177270927));
#27509=CARTESIAN_POINT('Ctrl Pts',(27.9623772429055,31.638209399578,10.3247095747713));
#27510=CARTESIAN_POINT('Ctrl Pts',(27.9925874699275,31.6803570199426,10.3736117457742));
#27511=CARTESIAN_POINT('Ctrl Pts',(28.0230259217659,31.7227565449012,10.4221009095725));
#27512=CARTESIAN_POINT('Ctrl Pts',(28.0536866918396,31.7653999649233,10.4701702229062));
#27513=CARTESIAN_POINT('Ctrl Pts',(26.4881263776672,35.8372231206707,0.));
#27514=CARTESIAN_POINT('Ctrl Pts',(26.3261800403055,35.9775504208019,1.72780310113343));
#27515=CARTESIAN_POINT('Ctrl Pts',(26.6551603137998,36.6844372319274,3.28449990511992));
#27516=CARTESIAN_POINT('Ctrl Pts',(26.984140587294,37.3913240430529,4.84119670910639));
#27517=CARTESIAN_POINT('Ctrl Pts',(27.7068134355443,38.552556305624,5.91846432228299));
#27518=CARTESIAN_POINT('Ctrl Pts',(28.4294862837945,39.7137885681951,6.99573193545956));
#27519=CARTESIAN_POINT('Ctrl Pts',(29.3706420279481,41.1271635338227,7.3802042952164));
#27520=CARTESIAN_POINT('Ctrl Pts',(30.3117977721017,42.5405384994504,7.76467665497322));
#27521=CARTESIAN_POINT('Ctrl Pts',(31.2529535162552,43.953913465078,7.38020429521639));
#27522=CARTESIAN_POINT('Ctrl Pts',(26.0399651488663,33.5084586029184,0.));
#27523=CARTESIAN_POINT('Ctrl Pts',(25.8780188115047,33.6487859030495,2.19648874705823));
#27524=CARTESIAN_POINT('Ctrl Pts',(26.3401683422827,34.5093582297243,4.17545672685568));
#27525=CARTESIAN_POINT('Ctrl Pts',(26.8023178730608,35.369930556399,6.15442470665314));
#27526=CARTESIAN_POINT('Ctrl Pts',(27.7649534312599,36.8080945488848,7.5239130403414));
#27527=CARTESIAN_POINT('Ctrl Pts',(28.727588989459,38.2462585413707,8.89340137402969));
#27528=CARTESIAN_POINT('Ctrl Pts',(29.9679733385715,40.0049617258242,9.38216610144961));
#27529=CARTESIAN_POINT('Ctrl Pts',(31.208357687684,41.7636649102778,9.87093082886954));
#27530=CARTESIAN_POINT('Ctrl Pts',(32.4487420367966,43.5223680947314,9.3821661014496));
#27531=CARTESIAN_POINT('Ctrl Pts',(25.1460896841347,31.3118750466443,0.));
#27532=CARTESIAN_POINT('Ctrl Pts',(24.9841433467731,31.4522023467755,2.70899372698069));
#27533=CARTESIAN_POINT('Ctrl Pts',(25.5919126722344,32.480828875122,5.14971273833323));
#27534=CARTESIAN_POINT('Ctrl Pts',(26.1996819976956,33.5094554034686,7.59043174968577));
#27535=CARTESIAN_POINT('Ctrl Pts',(27.4247153590146,35.2504426036074,9.27946171175751));
#27536=CARTESIAN_POINT('Ctrl Pts',(28.6497487203335,36.9914298037462,10.9684916738293));
#27537=CARTESIAN_POINT('Ctrl Pts',(30.2173377779967,39.1277473516754,11.5712994880388));
#27538=CARTESIAN_POINT('Ctrl Pts',(31.78492683566,41.2640648996045,12.1741073022483));
#27539=CARTESIAN_POINT('Ctrl Pts',(33.3525158933232,43.4003824475337,11.5712994880388));
#27540=CARTESIAN_POINT('Ctrl Pts',(23.8408520862202,29.3318883095339,0.));
#27541=CARTESIAN_POINT('Ctrl Pts',(23.6789057488586,29.4722156096651,3.24562220582793));
#27542=CARTESIAN_POINT('Ctrl Pts',(24.4391491613477,30.6768066147289,6.16982677025167));
#27543=CARTESIAN_POINT('Ctrl Pts',(25.1993925738368,31.8813976197927,9.09403133467541));
#27544=CARTESIAN_POINT('Ctrl Pts',(26.6991747463036,33.9394618506894,11.1176436806954));
#27545=CARTESIAN_POINT('Ctrl Pts',(28.1989569187704,35.9975260815862,13.1412560267153));
#27546=CARTESIAN_POINT('Ctrl Pts',(30.1091521400807,38.5292322196778,13.8634749112255));
#27547=CARTESIAN_POINT('Ctrl Pts',(32.0193473613909,41.0609383577694,14.5856937957357));
#27548=CARTESIAN_POINT('Ctrl Pts',(33.9295425827012,43.592644495861,13.8634749112255));
#27549=CARTESIAN_POINT('',(23.8408520862202,29.3318883095339,0.));
#27550=CARTESIAN_POINT('Ctrl Pts',(23.8408520862202,29.3318883095339,0.));
#27551=CARTESIAN_POINT('Ctrl Pts',(23.6789057488586,29.4722156096651,3.24562220582793));
#27552=CARTESIAN_POINT('Ctrl Pts',(24.4391491613477,30.6768066147289,6.16982677025167));
#27553=CARTESIAN_POINT('Ctrl Pts',(25.0738292744463,31.6824449968206,8.61106394926976));
#27554=CARTESIAN_POINT('Ctrl Pts',(26.240584724474,33.3059180634109,10.4489096280657));
#27555=CARTESIAN_POINT('Origin',(8.81246358936599,39.2388322978494,0.));
#27556=CARTESIAN_POINT('Ctrl Pts',(23.8408520862202,29.3318883095339,0.));
#27557=CARTESIAN_POINT('Ctrl Pts',(23.6789057488586,29.4722156096651,3.24562220582793));
#27558=CARTESIAN_POINT('Ctrl Pts',(24.4391491613477,30.6768066147289,6.16982677025167));
#27559=CARTESIAN_POINT('Ctrl Pts',(25.1993925738368,31.8813976197927,9.09403133467541));
#27560=CARTESIAN_POINT('Ctrl Pts',(26.6991747463036,33.9394618506894,11.1176436806954));
#27561=CARTESIAN_POINT('Ctrl Pts',(28.1989569187704,35.9975260815862,13.1412560267153));
#27562=CARTESIAN_POINT('Ctrl Pts',(30.1091521400807,38.5292322196778,13.8634749112255));
#27563=CARTESIAN_POINT('Ctrl Pts',(32.0193473613909,41.0609383577694,14.5856937957357));
#27564=CARTESIAN_POINT('Ctrl Pts',(33.9295425827012,43.592644495861,13.8634749112255));
#27565=CARTESIAN_POINT('Ctrl Pts',(23.9681616891744,28.3879644434326,0.));
#27566=CARTESIAN_POINT('Ctrl Pts',(23.8062153518128,28.5282917435638,3.38941559469372));
#27567=CARTESIAN_POINT('Ctrl Pts',(24.6073152722067,29.7800336722638,6.44317352589573));
#27568=CARTESIAN_POINT('Ctrl Pts',(25.4084151926006,31.0317756009639,9.49693145709774));
#27569=CARTESIAN_POINT('Ctrl Pts',(26.9818182484142,33.1748028604388,11.6101975146502));
#27570=CARTESIAN_POINT('Ctrl Pts',(28.5552213042278,35.3178301199138,13.7234635722027));
#27571=CARTESIAN_POINT('Ctrl Pts',(30.5572202654792,37.9554834217125,14.4776794959001));
#27572=CARTESIAN_POINT('Ctrl Pts',(32.5592192267306,40.5931367235112,15.2318954195974));
#27573=CARTESIAN_POINT('Ctrl Pts',(34.5612181879821,43.2307900253099,14.4776794959001));
#27574=CARTESIAN_POINT('Ctrl Pts',(24.6879908429608,27.7642289310884,0.));
#27575=CARTESIAN_POINT('Ctrl Pts',(24.5260445055992,27.9045562312196,3.38941559469372));
#27576=CARTESIAN_POINT('Ctrl Pts',(25.327144425993,29.1562981599196,6.44317352589574));
#27577=CARTESIAN_POINT('Ctrl Pts',(26.1282443463869,30.4080400886197,9.49693145709774));
#27578=CARTESIAN_POINT('Ctrl Pts',(27.7016474022005,32.5510673480946,11.6101975146502));
#27579=CARTESIAN_POINT('Ctrl Pts',(29.2750504580142,34.6940946075696,13.7234635722027));
#27580=CARTESIAN_POINT('Ctrl Pts',(31.2770494192656,37.3317479093683,14.4776794959001));
#27581=CARTESIAN_POINT('Ctrl Pts',(33.279048380517,39.969401211167,15.2318954195974));
#27582=CARTESIAN_POINT('Ctrl Pts',(35.2810473417684,42.6070545129657,14.4776794959001));
#27583=CARTESIAN_POINT('Ctrl Pts',(25.6404249706861,27.7725495286735,0.));
#27584=CARTESIAN_POINT('Ctrl Pts',(25.4784786333245,27.9128768288047,3.24562220582793));
#27585=CARTESIAN_POINT('Ctrl Pts',(26.2387220458135,29.1174678338684,6.16982677025167));
#27586=CARTESIAN_POINT('Ctrl Pts',(26.9989654583026,30.3220588389322,9.09403133467541));
#27587=CARTESIAN_POINT('Ctrl Pts',(28.4987476307694,32.380123069829,11.1176436806954));
#27588=CARTESIAN_POINT('Ctrl Pts',(29.9985298032362,34.4381873007258,13.1412560267153));
#27589=CARTESIAN_POINT('Ctrl Pts',(31.9087250245465,36.9698934388173,13.8634749112255));
#27590=CARTESIAN_POINT('Ctrl Pts',(33.8189202458568,39.5015995769089,14.5856937957357));
#27591=CARTESIAN_POINT('Ctrl Pts',(35.729115467167,42.0333057150005,13.8634749112255));
#27592=CARTESIAN_POINT('',(24.4459549573234,28.2121283533352,-2.36249235658883E-30));
#27593=CARTESIAN_POINT('Origin',(25.6247005192793,29.572480844482,0.));
#27594=CARTESIAN_POINT('Origin',(25.6247005192793,29.572480844482,0.));
#27595=CARTESIAN_POINT('Ctrl Pts',(29.3318883095343,23.8408520862197,0.));
#27596=CARTESIAN_POINT('Ctrl Pts',(29.1915610094032,24.0027984235813,3.24562220582793));
#27597=CARTESIAN_POINT('Ctrl Pts',(30.1154974142047,25.0869345107937,6.16982677025167));
#27598=CARTESIAN_POINT('Ctrl Pts',(31.0394338190063,26.171070598006,9.09403133467541));
#27599=CARTESIAN_POINT('Ctrl Pts',(32.8168434496408,27.994745445196,11.1176436806954));
#27600=CARTESIAN_POINT('Ctrl Pts',(34.5942530802753,29.8184202923861,13.1412560267153));
#27601=CARTESIAN_POINT('Ctrl Pts',(36.8453046181047,32.0525081884195,13.8634749112255));
#27602=CARTESIAN_POINT('Ctrl Pts',(39.0963561559341,34.286596084453,14.5856937957357));
#27603=CARTESIAN_POINT('Ctrl Pts',(41.3474076937634,36.5206839804864,13.8634749112255));
#27604=CARTESIAN_POINT('Ctrl Pts',(31.3118750466448,25.1460896841342,0.));
#27605=CARTESIAN_POINT('Ctrl Pts',(31.1715477465136,25.3080360214958,2.7089937269807));
#27606=CARTESIAN_POINT('Ctrl Pts',(31.9195196745979,26.2396980216803,5.14971273833323));
#27607=CARTESIAN_POINT('Ctrl Pts',(32.6674916026822,27.1713600218648,7.59043174968577));
#27608=CARTESIAN_POINT('Ctrl Pts',(34.1278242025588,28.720286057907,9.27946171175751));
#27609=CARTESIAN_POINT('Ctrl Pts',(35.5881568024354,30.2692120939491,10.9684916738293));
#27610=CARTESIAN_POINT('Ctrl Pts',(37.4438197501023,32.1606938263356,11.5712994880388));
#27611=CARTESIAN_POINT('Ctrl Pts',(39.2994826977692,34.052175558722,12.1741073022483));
#27612=CARTESIAN_POINT('Ctrl Pts',(41.1551456454362,35.9436572911085,11.5712994880388));
#27613=CARTESIAN_POINT('Ctrl Pts',(33.5084586029188,26.0399651488657,-1.05434036998093E-14));
#27614=CARTESIAN_POINT('Ctrl Pts',(33.3681313027877,26.2019114862273,2.19648874705823));
#27615=CARTESIAN_POINT('Ctrl Pts',(33.9480490292002,26.9879536917286,4.17545672685568));
#27616=CARTESIAN_POINT('Ctrl Pts',(34.5279667556127,27.7739958972299,6.15442470665314));
#27617=CARTESIAN_POINT('Ctrl Pts',(35.6854761478363,29.0605241301522,7.5239130403414));
#27618=CARTESIAN_POINT('Ctrl Pts',(36.8429855400598,30.3470523630746,8.89340137402968));
#27619=CARTESIAN_POINT('Ctrl Pts',(38.3210341242512,31.9113293869104,9.38216610144961));
#27620=CARTESIAN_POINT('Ctrl Pts',(39.7990827084425,33.4756064107461,9.87093082886955));
#27621=CARTESIAN_POINT('Ctrl Pts',(41.2771312926339,35.0398834345819,9.38216610144961));
#27622=CARTESIAN_POINT('Ctrl Pts',(35.8372231206712,26.4881263776665,0.));
#27623=CARTESIAN_POINT('Ctrl Pts',(35.6968958205401,26.6500727150282,1.72780310113343));
#27624=CARTESIAN_POINT('Ctrl Pts',(36.1231280314034,27.3029456632456,3.28449990511992));
#27625=CARTESIAN_POINT('Ctrl Pts',(36.5493602422666,27.9558186114631,4.84119670910638));
#27626=CARTESIAN_POINT('Ctrl Pts',(37.4299379045754,29.0023841344366,5.91846432228298));
#27627=CARTESIAN_POINT('Ctrl Pts',(38.3105155668842,30.0489496574101,6.99573193545956));
#27628=CARTESIAN_POINT('Ctrl Pts',(39.4432359322497,31.3139980762869,7.38020429521639));
#27629=CARTESIAN_POINT('Ctrl Pts',(40.5759562976151,32.5790464951637,7.76467665497322));
#27630=CARTESIAN_POINT('Ctrl Pts',(41.7086766629805,33.8440949140405,7.38020429521639));
#27631=CARTESIAN_POINT('',(29.3318883095548,23.8408520862335,1.57950172528022E-9));
#27632=CARTESIAN_POINT('Origin',(39.2388322978496,8.81246358936532,0.));
#27633=CARTESIAN_POINT('Ctrl Pts',(29.3318883094704,23.840852086423,3.1310780077989E-9));
#27634=CARTESIAN_POINT('Ctrl Pts',(29.3212938718738,23.8530787192646,0.245038153335593));
#27635=CARTESIAN_POINT('Ctrl Pts',(29.3153958352832,23.8695636319733,0.490791160521933));
#27636=CARTESIAN_POINT('Ctrl Pts',(29.3142795252166,23.8903394438997,0.736766500725686));
#27637=CARTESIAN_POINT('Ctrl Pts',(29.3131668799332,23.9110470500023,0.981934317701342));
#27638=CARTESIAN_POINT('Ctrl Pts',(29.3168047115563,23.9360174743377,1.227322573766));
#27639=CARTESIAN_POINT('Ctrl Pts',(29.3252401898306,23.965248740963,1.47243294816377));
#27640=CARTESIAN_POINT('Ctrl Pts',(29.3336629639887,23.9944359843101,1.71717417803053));
#27641=CARTESIAN_POINT('Ctrl Pts',(29.3468690005324,24.0278712558265,1.96163791541622));
#27642=CARTESIAN_POINT('Ctrl Pts',(29.3648668425816,24.0655179217451,2.2053240877856));
#27643=CARTESIAN_POINT('Ctrl Pts',(29.3828492487603,24.1031322999562,2.44880126242104));
#27644=CARTESIAN_POINT('Ctrl Pts',(29.4056152523349,24.1449508188713,2.6915017543109));
#27645=CARTESIAN_POINT('Ctrl Pts',(29.4331345151071,24.1909024709822,2.9329295186685));
#27646=CARTESIAN_POINT('Ctrl Pts',(29.4606480207945,24.2368445099158,3.17430677585634));
#27647=CARTESIAN_POINT('Ctrl Pts',(29.492912756491,24.2869178772579,3.41441139318391));
#27648=CARTESIAN_POINT('Ctrl Pts',(29.5298597835414,24.341017951831,3.65275710614686));
#27649=CARTESIAN_POINT('Ctrl Pts',(29.5668537253365,24.3951867218145,3.89140546668843));
#27650=CARTESIAN_POINT('Ctrl Pts',(29.6085417737706,24.4533923189748,4.12829002081224));
#27651=CARTESIAN_POINT('Ctrl Pts',(29.6548169223665,24.5154973789738,4.36293874377873));
#27652=CARTESIAN_POINT('Ctrl Pts',(29.7011392900673,24.5776658109,4.59782690201513));
#27653=CARTESIAN_POINT('Ctrl Pts',(29.7520579892329,24.6437415114729,4.83047425895023));
#27654=CARTESIAN_POINT('Ctrl Pts',(29.8074294704424,24.7135563309893,5.06042975959494));
#27655=CARTESIAN_POINT('Ctrl Pts',(29.862962836158,24.7835752616714,5.29105755998378));
#27656=CARTESIAN_POINT('Ctrl Pts',(29.9229748872206,24.8573550203558,5.51897736305772));
#27657=CARTESIAN_POINT('Ctrl Pts',(29.9872866904184,24.9346980180644,5.74376259354425));
#27658=CARTESIAN_POINT('Ctrl Pts',(30.0282938085162,24.9840142132784,5.88709234072681));
#27659=CARTESIAN_POINT('Ctrl Pts',(30.0710484023926,25.034778564225,6.02914825314223));
#27660=CARTESIAN_POINT('Ctrl Pts',(30.1154974142345,25.0869345108127,6.16982677023484));
#27661=CARTESIAN_POINT('Ctrl Pts',(30.185194772364,25.1687165693392,6.39041482339089));
#27662=CARTESIAN_POINT('Ctrl Pts',(30.2593411758391,25.2545422584419,6.60890054011803));
#27663=CARTESIAN_POINT('Ctrl Pts',(30.3378542445907,25.3442989836975,6.82480412008038));
#27664=CARTESIAN_POINT('Ctrl Pts',(30.4161900656828,25.433853078108,7.04022028559285));
#27665=CARTESIAN_POINT('Ctrl Pts',(30.4988728090635,25.5273204012122,7.25306552029626));
#27666=CARTESIAN_POINT('Ctrl Pts',(30.5857836273893,25.6245550984952,7.46287566269403));
#27667=CARTESIAN_POINT('Ctrl Pts',(30.6725546575099,25.7216334025456,7.67234834441864));
#27668=CARTESIAN_POINT('Ctrl Pts',(30.76354007733,25.8224668509012,7.87879526533008));
#27669=CARTESIAN_POINT('Ctrl Pts',(30.858585742418,25.9268778285522,8.08177334612172));
#27670=CARTESIAN_POINT('Ctrl Pts',(30.9535402077704,26.0311886201132,8.28455666214105));
#27671=CARTESIAN_POINT('Ctrl Pts',(31.052546990739,26.1390699181376,8.48387739272866));
#27672=CARTESIAN_POINT('Ctrl Pts',(31.1554183156071,26.2503142961678,8.67931873611123));
#27673=CARTESIAN_POINT('Ctrl Pts',(31.2582945883135,26.3615640247581,8.87476947970508));
#27674=CARTESIAN_POINT('Ctrl Pts',(31.3650355954447,26.4761769610839,9.06634009532832));
#27675=CARTESIAN_POINT('Ctrl Pts',(31.4754218249885,26.5939179778765,9.25364450340974));
#27676=CARTESIAN_POINT('Ctrl Pts',(31.5858485486312,26.711702186799,9.44101762226468));
#27677=CARTESIAN_POINT('Ctrl Pts',(31.6999229509133,26.8326165417651,9.62412107874988));
#27678=CARTESIAN_POINT('Ctrl Pts',(31.8173965346648,26.9564011630242,9.80260437466064));
#27679=CARTESIAN_POINT('Ctrl Pts',(31.9350617421636,27.08038770264,9.98137881379626));
#27680=CARTESIAN_POINT('Ctrl Pts',(32.0561369802834,27.2072536245427,10.155517727092));
#27681=CARTESIAN_POINT('Ctrl Pts',(32.1803472149479,27.3367168513598,10.3247095747704));
#27682=CARTESIAN_POINT('Ctrl Pts',(32.2162481771956,27.3741361061496,10.3736117457753));
#27683=CARTESIAN_POINT('Ctrl Pts',(32.2524108910217,27.41177222173,10.4221009095756));
#27684=CARTESIAN_POINT('Ctrl Pts',(32.2888283700906,27.4496181106902,10.4701702229111));
#27685=CARTESIAN_POINT('Ctrl Pts',(31.3186840564488,31.702798440711,0.));
#27686=CARTESIAN_POINT('Ctrl Pts',(31.1783567563176,31.8647447780726,1.72780310113343));
#27687=CARTESIAN_POINT('Ctrl Pts',(31.6045889671809,32.51761772629,3.28449990511991));
#27688=CARTESIAN_POINT('Ctrl Pts',(32.0308211780442,33.1704906745075,4.84119670910638));
#27689=CARTESIAN_POINT('Ctrl Pts',(32.911398840353,34.217056197481,5.91846432228298));
#27690=CARTESIAN_POINT('Ctrl Pts',(33.7919765026618,35.2636217204545,6.99573193545956));
#27691=CARTESIAN_POINT('Ctrl Pts',(34.9246968680272,36.5286701393313,7.38020429521639));
#27692=CARTESIAN_POINT('Ctrl Pts',(36.0574172333927,37.7937185582081,7.76467665497322));
#27693=CARTESIAN_POINT('Ctrl Pts',(37.1901375987581,39.0587669770849,7.38020429521639));
#27694=CARTESIAN_POINT('Ctrl Pts',(30.5436667170415,29.4615173807453,0.));
#27695=CARTESIAN_POINT('Ctrl Pts',(30.4033394169104,29.6234637181069,2.19648874705824));
#27696=CARTESIAN_POINT('Ctrl Pts',(30.9832571433228,30.4095059236082,4.17545672685568));
#27697=CARTESIAN_POINT('Ctrl Pts',(31.5631748697354,31.1955481291095,6.15442470665314));
#27698=CARTESIAN_POINT('Ctrl Pts',(32.7206842619589,32.4820763620318,7.5239130403414));
#27699=CARTESIAN_POINT('Ctrl Pts',(33.8781936541825,33.7686045949542,8.89340137402967));
#27700=CARTESIAN_POINT('Ctrl Pts',(35.3562422383739,35.3328816187899,9.3821661014496));
#27701=CARTESIAN_POINT('Ctrl Pts',(36.8342908225652,36.8971586426257,9.87093082886954));
#27702=CARTESIAN_POINT('Ctrl Pts',(38.3123394067565,38.4614356664615,9.3821661014496));
#27703=CARTESIAN_POINT('Ctrl Pts',(29.346283182114,27.4145036200619,0.));
#27704=CARTESIAN_POINT('Ctrl Pts',(29.2059558819829,27.5764499574235,2.7089937269807));
#27705=CARTESIAN_POINT('Ctrl Pts',(29.9539278100672,28.508111957608,5.14971273833323));
#27706=CARTESIAN_POINT('Ctrl Pts',(30.7018997381515,29.4397739577925,7.59043174968578));
#27707=CARTESIAN_POINT('Ctrl Pts',(32.1622323380281,30.9886999938347,9.27946171175752));
#27708=CARTESIAN_POINT('Ctrl Pts',(33.6225649379047,32.5376260298769,10.9684916738293));
#27709=CARTESIAN_POINT('Ctrl Pts',(35.4782278855716,34.4291077622633,11.5712994880388));
#27710=CARTESIAN_POINT('Ctrl Pts',(37.3338908332385,36.3205894946498,12.1741073022483));
#27711=CARTESIAN_POINT('Ctrl Pts',(39.1895537809054,38.2120712270362,11.5712994880388));
#27712=CARTESIAN_POINT('Ctrl Pts',(27.7725495286739,25.6404249706856,0.));
#27713=CARTESIAN_POINT('Ctrl Pts',(27.6322222285428,25.8023713080472,3.24562220582792));
#27714=CARTESIAN_POINT('Ctrl Pts',(28.5561586333444,26.8865073952596,6.16982677025168));
#27715=CARTESIAN_POINT('Ctrl Pts',(29.4800950381459,27.9706434824719,9.09403133467541));
#27716=CARTESIAN_POINT('Ctrl Pts',(31.2575046687804,29.7943183296619,11.1176436806954));
#27717=CARTESIAN_POINT('Ctrl Pts',(33.0349142994149,31.6179931768519,13.1412560267153));
#27718=CARTESIAN_POINT('Ctrl Pts',(35.2859658372443,33.8520810728854,13.8634749112255));
#27719=CARTESIAN_POINT('Ctrl Pts',(37.5370173750737,36.0861689689189,14.5856937957357));
#27720=CARTESIAN_POINT('Ctrl Pts',(39.7880689129031,38.3202568649523,13.8634749112255));
#27721=CARTESIAN_POINT('',(27.7725495286739,25.6404249706856,0.));
#27722=CARTESIAN_POINT('Ctrl Pts',(27.7725495286739,25.6404249706856,0.));
#27723=CARTESIAN_POINT('Ctrl Pts',(27.6322222285428,25.8023713080473,3.24562220582792));
#27724=CARTESIAN_POINT('Ctrl Pts',(28.5561586333444,26.8865073952596,6.16982677025168));
#27725=CARTESIAN_POINT('Ctrl Pts',(29.3274958817336,27.7915854309815,8.61106394926976));
#27726=CARTESIAN_POINT('Ctrl Pts',(30.7134197505153,29.2324872694336,10.4489096280657));
#27727=CARTESIAN_POINT('Origin',(14.3070334890505,37.5852932322716,0.));
#27728=CARTESIAN_POINT('Ctrl Pts',(27.7725495286739,25.6404249706856,0.));
#27729=CARTESIAN_POINT('Ctrl Pts',(27.6322222285428,25.8023713080473,3.24562220582792));
#27730=CARTESIAN_POINT('Ctrl Pts',(28.5561586333444,26.8865073952596,6.16982677025168));
#27731=CARTESIAN_POINT('Ctrl Pts',(29.4800950381459,27.9706434824719,9.09403133467541));
#27732=CARTESIAN_POINT('Ctrl Pts',(31.2575046687804,29.7943183296619,11.1176436806954));
#27733=CARTESIAN_POINT('Ctrl Pts',(33.0349142994149,31.6179931768519,13.1412560267153));
#27734=CARTESIAN_POINT('Ctrl Pts',(35.2859658372443,33.8520810728854,13.8634749112255));
#27735=CARTESIAN_POINT('Ctrl Pts',(37.5370173750737,36.0861689689189,14.5856937957357));
#27736=CARTESIAN_POINT('Ctrl Pts',(39.7880689129031,38.3202568649523,13.8634749112255));
#27737=CARTESIAN_POINT('Ctrl Pts',(27.7642289310889,24.6879908429603,0.));
#27738=CARTESIAN_POINT('Ctrl Pts',(27.6239016309577,24.8499371803219,3.38941559469372));
#27739=CARTESIAN_POINT('Ctrl Pts',(28.5949889593955,25.974929775439,6.44317352589573));
#27740=CARTESIAN_POINT('Ctrl Pts',(29.5660762878334,27.0999223705561,9.49693145709776));
#27741=CARTESIAN_POINT('Ctrl Pts',(31.4284489470461,28.997218101093,11.6101975146502));
#27742=CARTESIAN_POINT('Ctrl Pts',(33.2908216062588,30.8945138316298,13.7234635722027));
#27743=CARTESIAN_POINT('Ctrl Pts',(35.6478203077953,33.2204054676045,14.4776794959001));
#27744=CARTESIAN_POINT('Ctrl Pts',(38.0048190093318,35.5462971035791,15.2318954195974));
#27745=CARTESIAN_POINT('Ctrl Pts',(40.3618177108683,37.8721887395537,14.4776794959001));
#27746=CARTESIAN_POINT('Ctrl Pts',(28.387964443433,23.9681616891739,0.));
#27747=CARTESIAN_POINT('Ctrl Pts',(28.2476371433019,24.1301080265356,3.38941559469372));
#27748=CARTESIAN_POINT('Ctrl Pts',(29.2187244717397,25.2551006216527,6.44317352589573));
#27749=CARTESIAN_POINT('Ctrl Pts',(30.1898118001775,26.3800932167698,9.49693145709775));
#27750=CARTESIAN_POINT('Ctrl Pts',(32.0521844593903,28.2773889473066,11.6101975146502));
#27751=CARTESIAN_POINT('Ctrl Pts',(33.914557118603,30.1746846778435,13.7234635722027));
#27752=CARTESIAN_POINT('Ctrl Pts',(36.2715558201394,32.5005763138181,14.4776794959001));
#27753=CARTESIAN_POINT('Ctrl Pts',(38.6285545216759,34.8264679497928,15.2318954195974));
#27754=CARTESIAN_POINT('Ctrl Pts',(40.9855532232124,37.1523595857673,14.4776794959001));
#27755=CARTESIAN_POINT('Ctrl Pts',(29.3318883095343,23.8408520862197,0.));
#27756=CARTESIAN_POINT('Ctrl Pts',(29.1915610094032,24.0027984235813,3.24562220582793));
#27757=CARTESIAN_POINT('Ctrl Pts',(30.1154974142047,25.0869345107937,6.16982677025167));
#27758=CARTESIAN_POINT('Ctrl Pts',(31.0394338190063,26.171070598006,9.09403133467541));
#27759=CARTESIAN_POINT('Ctrl Pts',(32.8168434496408,27.994745445196,11.1176436806954));
#27760=CARTESIAN_POINT('Ctrl Pts',(34.5942530802753,29.8184202923861,13.1412560267153));
#27761=CARTESIAN_POINT('Ctrl Pts',(36.8453046181047,32.0525081884195,13.8634749112255));
#27762=CARTESIAN_POINT('Ctrl Pts',(39.0963561559341,34.286596084453,14.5856937957357));
#27763=CARTESIAN_POINT('Ctrl Pts',(41.3474076937634,36.5206839804864,13.8634749112255));
#27764=CARTESIAN_POINT('',(28.2121348679648,24.44594743904,3.59391606952161E-31));
#27765=CARTESIAN_POINT('Origin',(29.5724808444824,25.6247005192788,0.));
#27766=CARTESIAN_POINT('Origin',(29.5724808444824,25.6247005192788,0.));
#27767=CARTESIAN_POINT('Ctrl Pts',(32.4262389885814,19.4238236466306,1.04083408558608E-14));
#27768=CARTESIAN_POINT('Ctrl Pts',(32.310387384841,19.6040922608087,3.24562220582793));
#27769=CARTESIAN_POINT('Ctrl Pts',(33.3792081011658,20.5457035458242,6.16982677025168));
#27770=CARTESIAN_POINT('Ctrl Pts',(34.4480288174906,21.4873148308397,9.09403133467541));
#27771=CARTESIAN_POINT('Ctrl Pts',(36.4668829718392,23.0394755334782,11.1176436806954));
#27772=CARTESIAN_POINT('Ctrl Pts',(38.4857371261878,24.5916362361167,13.1412560267153));
#27773=CARTESIAN_POINT('Ctrl Pts',(41.0318200627227,26.4826263031063,13.8634749112255));
#27774=CARTESIAN_POINT('Ctrl Pts',(43.5779029992576,28.3736163700958,14.5856937957357));
#27775=CARTESIAN_POINT('Ctrl Pts',(46.1239859357924,30.2646064370854,13.8634749112255));
#27776=CARTESIAN_POINT('Ctrl Pts',(34.5718269932686,20.4339943155204,0.));
#27777=CARTESIAN_POINT('Ctrl Pts',(34.4559753895281,20.6142629296985,2.70899372698069));
#27778=CARTESIAN_POINT('Ctrl Pts',(35.3289233687526,21.4299944500885,5.14971273833323));
#27779=CARTESIAN_POINT('Ctrl Pts',(36.2018713479771,22.2457259704785,7.59043174968577));
#27780=CARTESIAN_POINT('Ctrl Pts',(37.8677750259293,23.571059175064,9.27946171175751));
#27781=CARTESIAN_POINT('Ctrl Pts',(39.5336787038815,24.8963923796496,10.9684916738292));
#27782=CARTESIAN_POINT('Ctrl Pts',(41.6396395952276,26.5045331830048,11.5712994880388));
#27783=CARTESIAN_POINT('Ctrl Pts',(43.7456004865738,28.1126739863601,12.1741073022483));
#27784=CARTESIAN_POINT('Ctrl Pts',(45.8515613779199,29.7208147897153,11.5712994880388));
#27785=CARTESIAN_POINT('Ctrl Pts',(36.8732642383515,21.006164983318,0.));
#27786=CARTESIAN_POINT('Ctrl Pts',(36.757412634611,21.1864335974961,2.19648874705823));
#27787=CARTESIAN_POINT('Ctrl Pts',(37.4432931040928,21.8819441292785,4.17545672685567));
#27788=CARTESIAN_POINT('Ctrl Pts',(38.1291735735746,22.5774546610608,6.15442470665314));
#27789=CARTESIAN_POINT('Ctrl Pts',(39.4579932465785,23.6861571296384,7.5239130403414));
#27790=CARTESIAN_POINT('Ctrl Pts',(40.7868129195823,24.794859598216,8.89340137402967));
#27791=CARTESIAN_POINT('Ctrl Pts',(42.4724369320184,26.1328662922311,9.3821661014496));
#27792=CARTESIAN_POINT('Ctrl Pts',(44.1580609444546,27.4708729862462,9.87093082886954));
#27793=CARTESIAN_POINT('Ctrl Pts',(45.8436849568907,28.8088796802613,9.3821661014496));
#27794=CARTESIAN_POINT('Ctrl Pts',(39.2421052839114,21.1183468312843,0.));
#27795=CARTESIAN_POINT('Ctrl Pts',(39.126253680171,21.2986154454624,1.72780310113342));
#27796=CARTESIAN_POINT('Ctrl Pts',(39.6410609697423,21.8841839202762,3.28449990511992));
#27797=CARTESIAN_POINT('Ctrl Pts',(40.1558682593137,22.46975239509,4.84119670910638));
#27798=CARTESIAN_POINT('Ctrl Pts',(41.1764247138527,23.3803461224639,5.91846432228298));
#27799=CARTESIAN_POINT('Ctrl Pts',(42.1969811683917,24.2909398498379,6.99573193545956));
#27800=CARTESIAN_POINT('Ctrl Pts',(43.4982072348259,25.3819089842539,7.3802042952164));
#27801=CARTESIAN_POINT('Ctrl Pts',(44.7994333012602,26.4728781186699,7.76467665497322));
#27802=CARTESIAN_POINT('Ctrl Pts',(46.1006593676944,27.5638472530859,7.38020429521639));
#27803=CARTESIAN_POINT('',(32.4262389886935,19.4238236466219,1.57950316568597E-9));
#27804=CARTESIAN_POINT('Origin',(40.0935818932913,3.13849734404774,0.));
#27805=CARTESIAN_POINT('Ctrl Pts',(32.4262389885471,19.4238236468409,3.1310815762065E-9));
#27806=CARTESIAN_POINT('Ctrl Pts',(32.4174924183248,19.4374335758627,0.245038153335351));
#27807=CARTESIAN_POINT('Ctrl Pts',(32.4140004629285,19.4545900740528,0.490791160521444));
#27808=CARTESIAN_POINT('Ctrl Pts',(32.415852221603,19.4753132856566,0.736766500724951));
#27809=CARTESIAN_POINT('Ctrl Pts',(32.4176979010578,19.4959684641205,0.981934317700587));
#27810=CARTESIAN_POINT('Ctrl Pts',(32.4248523667013,19.5201670081214,1.22732257376522));
#27811=CARTESIAN_POINT('Ctrl Pts',(32.4373620269519,19.5479002488741,1.47243294816298));
#27812=CARTESIAN_POINT('Ctrl Pts',(32.4498528472303,19.5755917224263,1.71717417802969));
#27813=CARTESIAN_POINT('Ctrl Pts',(32.467682800622,19.6068072561334,1.96163791541534));
#27814=CARTESIAN_POINT('Ctrl Pts',(32.4908551297617,19.6415093732945,2.20532408778468));
#27815=CARTESIAN_POINT('Ctrl Pts',(32.5140075851258,19.6761817281437,2.4488012624201));
#27816=CARTESIAN_POINT('Ctrl Pts',(32.5424932593661,19.7143346547167,2.69150175430996));
#27817=CARTESIAN_POINT('Ctrl Pts',(32.5762720176612,19.7559021858351,2.93292951866755));
#27818=CARTESIAN_POINT('Ctrl Pts',(32.6100437093728,19.7974610209431,3.17430677585539));
#27819=CARTESIAN_POINT('Ctrl Pts',(32.6491062197569,19.8424329629628,3.41441139318295));
#27820=CARTESIAN_POINT('Ctrl Pts',(32.6933764227085,19.8907242666033,3.6527571061459));
#27821=CARTESIAN_POINT('Ctrl Pts',(32.7377028392566,19.9390768897696,3.89140546668738));
#27822=CARTESIAN_POINT('Ctrl Pts',(32.7872500836133,19.9907572100055,4.12829002081109));
#27823=CARTESIAN_POINT('Ctrl Pts',(32.8418926894894,20.0456444897533,4.36293874377749));
#27824=CARTESIAN_POINT('Ctrl Pts',(32.8965910526136,20.1005877764142,4.5978269020138));
#27825=CARTESIAN_POINT('Ctrl Pts',(32.9563950254811,20.1587444351916,4.83047425894881));
#27826=CARTESIAN_POINT('Ctrl Pts',(33.0211385895995,20.2199684571167,5.06042975959344));
#27827=CARTESIAN_POINT('Ctrl Pts',(33.0860714385207,20.2813714740828,5.29105755998216));
#27828=CARTESIAN_POINT('Ctrl Pts',(33.1559726078587,20.3458596558639,5.51897736305598));
#27829=CARTESIAN_POINT('Ctrl Pts',(33.2306368658403,20.413262889504,5.7437625935424));
#27830=CARTESIAN_POINT('Ctrl Pts',(33.2782450169496,20.4562411955789,5.88709234072559));
#27831=CARTESIAN_POINT('Ctrl Pts',(33.3277889511025,20.5004042255162,6.02914825314163));
#27832=CARTESIAN_POINT('Ctrl Pts',(33.3792081011979,20.5457035458388,6.16982677023484));
#27833=CARTESIAN_POINT('Ctrl Pts',(33.4598348411498,20.6167342126792,6.390414823391));
#27834=CARTESIAN_POINT('Ctrl Pts',(33.5454408102123,20.6911341865983,6.60890054011824));
#27835=CARTESIAN_POINT('Ctrl Pts',(33.6359284429692,20.7688037431276,6.82480412008069));
#27836=CARTESIAN_POINT('Ctrl Pts',(33.7262117948162,20.8462979562736,7.04022028559317));
#27837=CARTESIAN_POINT('Ctrl Pts',(33.8213547340594,20.9270469355452,7.25306552029659));
#27838=CARTESIAN_POINT('Ctrl Pts',(33.9212188657882,21.0109232247564,7.46287566269436));
#27839=CARTESIAN_POINT('Ctrl Pts',(34.0209223750764,21.0946646065286,7.6723483444191));
#27840=CARTESIAN_POINT('Ctrl Pts',(34.1253317904082,21.1815231404629,7.87879526533065));
#27841=CARTESIAN_POINT('Ctrl Pts',(34.2342692590686,21.2713449564541,8.08177334612241));
#27842=CARTESIAN_POINT('Ctrl Pts',(34.3431021983079,21.3610805851808,8.28455666214176));
#27843=CARTESIAN_POINT('Ctrl Pts',(34.456454344463,21.4537736728372,8.48387739272939));
#27844=CARTESIAN_POINT('Ctrl Pts',(34.5741103132403,21.5492456275386,8.67931873611198));
#27845=CARTESIAN_POINT('Ctrl Pts',(34.6917719409582,21.6447221741883,8.87476947970573));
#27846=CARTESIAN_POINT('Ctrl Pts',(34.8137376000418,21.7429776869135,9.06634009532888));
#27847=CARTESIAN_POINT('Ctrl Pts',(34.9397565506955,21.8438106715185,9.25364450341021));
#27848=CARTESIAN_POINT('Ctrl Pts',(35.0658217301578,21.9446806457088,9.44101762226526));
#27849=CARTESIAN_POINT('Ctrl Pts',(35.1959429263784,22.0481297867737,9.62412107875057));
#27850=CARTESIAN_POINT('Ctrl Pts',(35.3298371867854,22.1539362249981,9.80260437466142));
#27851=CARTESIAN_POINT('Ctrl Pts',(35.4639498564645,22.2599152554387,9.98137881379685));
#27852=CARTESIAN_POINT('Ctrl Pts',(35.6018476263942,22.3682590622501,10.1555177270924));
#27853=CARTESIAN_POINT('Ctrl Pts',(35.7432181181529,22.4787275806304,10.3247095747707));
#27854=CARTESIAN_POINT('Ctrl Pts',(35.7840789755634,22.5106567217244,10.3736117457754));
#27855=CARTESIAN_POINT('Ctrl Pts',(35.8252297828071,22.5427632651452,10.4221009095756));
#27856=CARTESIAN_POINT('Ctrl Pts',(35.8666626160154,22.575041189881,10.4701702229111));
#27857=CARTESIAN_POINT('Ctrl Pts',(35.5116836434679,26.9229962078195,0.));
#27858=CARTESIAN_POINT('Ctrl Pts',(35.3958320397274,27.1032648219976,1.72780310113343));
#27859=CARTESIAN_POINT('Ctrl Pts',(35.9106393292987,27.6888332968114,3.28449990511991));
#27860=CARTESIAN_POINT('Ctrl Pts',(36.4254466188701,28.2744017716252,4.84119670910639));
#27861=CARTESIAN_POINT('Ctrl Pts',(37.4460030734091,29.1849954989991,5.91846432228298));
#27862=CARTESIAN_POINT('Ctrl Pts',(38.4665595279481,30.0955892263731,6.99573193545956));
#27863=CARTESIAN_POINT('Ctrl Pts',(39.7677855943823,31.1865583607891,7.38020429521639));
#27864=CARTESIAN_POINT('Ctrl Pts',(41.0690116608166,32.2775274952051,7.76467665497322));
#27865=CARTESIAN_POINT('Ctrl Pts',(42.3702377272508,33.368496629621,7.38020429521639));
#27866=CARTESIAN_POINT('Ctrl Pts',(34.425587311519,24.8148246247006,0.));
#27867=CARTESIAN_POINT('Ctrl Pts',(34.3097357077786,24.9950932388787,2.19648874705823));
#27868=CARTESIAN_POINT('Ctrl Pts',(34.9956161772604,25.690603770661,4.17545672685568));
#27869=CARTESIAN_POINT('Ctrl Pts',(35.6814966467422,26.3861143024433,6.15442470665313));
#27870=CARTESIAN_POINT('Ctrl Pts',(37.010316319746,27.494816771021,7.5239130403414));
#27871=CARTESIAN_POINT('Ctrl Pts',(38.3391359927498,28.6035192395986,8.89340137402967));
#27872=CARTESIAN_POINT('Ctrl Pts',(40.024760005186,29.9415259336137,9.38216610144961));
#27873=CARTESIAN_POINT('Ctrl Pts',(41.7103840176221,31.2795326276287,9.87093082886953));
#27874=CARTESIAN_POINT('Ctrl Pts',(43.3960080300583,32.6175393216438,9.3821661014496));
#27875=CARTESIAN_POINT('Ctrl Pts',(32.9490709821978,22.9590519566751,0.));
#27876=CARTESIAN_POINT('Ctrl Pts',(32.8332193784573,23.1393205708532,2.7089937269807));
#27877=CARTESIAN_POINT('Ctrl Pts',(33.7061673576818,23.9550520912432,5.14971273833323));
#27878=CARTESIAN_POINT('Ctrl Pts',(34.5791153369063,24.7707836116333,7.59043174968577));
#27879=CARTESIAN_POINT('Ctrl Pts',(36.2450190148585,26.0961168162188,9.27946171175751));
#27880=CARTESIAN_POINT('Ctrl Pts',(37.9109226928106,27.4214500208043,10.9684916738292));
#27881=CARTESIAN_POINT('Ctrl Pts',(40.0168835841568,29.0295908241596,11.5712994880388));
#27882=CARTESIAN_POINT('Ctrl Pts',(42.1228444755029,30.6377316275148,12.1741073022483));
#27883=CARTESIAN_POINT('Ctrl Pts',(44.2288053668491,32.2458724308701,11.5712994880388));
#27884=CARTESIAN_POINT('Ctrl Pts',(31.1388779521431,21.4269965203138,0.));
#27885=CARTESIAN_POINT('Ctrl Pts',(31.0230263484026,21.607265134492,3.24562220582793));
#27886=CARTESIAN_POINT('Ctrl Pts',(32.0918470647274,22.5488764195075,6.16982677025167));
#27887=CARTESIAN_POINT('Ctrl Pts',(33.1606677810522,23.490487704523,9.09403133467541));
#27888=CARTESIAN_POINT('Ctrl Pts',(35.1795219354008,25.0426484071615,11.1176436806954));
#27889=CARTESIAN_POINT('Ctrl Pts',(37.1983760897495,26.5948091098,13.1412560267153));
#27890=CARTESIAN_POINT('Ctrl Pts',(39.7444590262843,28.4857991767895,13.8634749112255));
#27891=CARTESIAN_POINT('Ctrl Pts',(42.2905419628192,30.3767892437791,14.5856937957357));
#27892=CARTESIAN_POINT('Ctrl Pts',(44.8366248993541,32.2677793107686,13.8634749112255));
#27893=CARTESIAN_POINT('',(31.1388779521431,21.4269965203138,0.));
#27894=CARTESIAN_POINT('Ctrl Pts',(31.1388779521431,21.4269965203138,0.));
#27895=CARTESIAN_POINT('Ctrl Pts',(31.0230263484026,21.607265134492,3.24562220582793));
#27896=CARTESIAN_POINT('Ctrl Pts',(32.0918470647274,22.5488764195074,6.16982677025168));
#27897=CARTESIAN_POINT('Ctrl Pts',(32.984139246383,23.3349693300819,8.61106394926976));
#27898=CARTESIAN_POINT('Ctrl Pts',(34.5610181206247,24.5639673341826,10.4489096280657));
#27899=CARTESIAN_POINT('Origin',(19.5103534449755,35.16662598352,0.));
#27900=CARTESIAN_POINT('Ctrl Pts',(31.1388779521431,21.4269965203138,0.));
#27901=CARTESIAN_POINT('Ctrl Pts',(31.0230263484026,21.607265134492,3.24562220582793));
#27902=CARTESIAN_POINT('Ctrl Pts',(32.0918470647274,22.5488764195075,6.16982677025167));
#27903=CARTESIAN_POINT('Ctrl Pts',(33.1606677810522,23.490487704523,9.09403133467541));
#27904=CARTESIAN_POINT('Ctrl Pts',(35.1795219354008,25.0426484071615,11.1176436806954));
#27905=CARTESIAN_POINT('Ctrl Pts',(37.1983760897495,26.5948091098,13.1412560267153));
#27906=CARTESIAN_POINT('Ctrl Pts',(39.7444590262843,28.4857991767895,13.8634749112255));
#27907=CARTESIAN_POINT('Ctrl Pts',(42.2905419628192,30.3767892437791,14.5856937957357));
#27908=CARTESIAN_POINT('Ctrl Pts',(44.8366248993541,32.2677793107686,13.8634749112255));
#27909=CARTESIAN_POINT('Ctrl Pts',(30.9950965373909,20.4854409432118,6.24500451351651E-15));
#27910=CARTESIAN_POINT('Ctrl Pts',(30.8792449336505,20.6657095573899,3.38941559469373));
#27911=CARTESIAN_POINT('Ctrl Pts',(32.0005511325098,21.6410512138983,6.44317352589574));
#27912=CARTESIAN_POINT('Ctrl Pts',(33.1218573313691,22.6163928704066,9.49693145709774));
#27913=CARTESIAN_POINT('Ctrl Pts',(35.2352870572787,24.2293336022806,11.6101975146502));
#27914=CARTESIAN_POINT('Ctrl Pts',(37.3487167831882,25.8422743341547,13.7234635722027));
#27915=CARTESIAN_POINT('Ctrl Pts',(40.0127335284694,27.8090558579144,14.4776794959001));
#27916=CARTESIAN_POINT('Ctrl Pts',(42.6767502737507,29.7758373816741,15.2318954195974));
#27917=CARTESIAN_POINT('Ctrl Pts',(45.3407670190319,31.7426189054338,14.4776794959001));
#27918=CARTESIAN_POINT('Ctrl Pts',(31.5100409519663,19.6841717937385,0.));
#27919=CARTESIAN_POINT('Ctrl Pts',(31.3941893482258,19.8644404079166,3.38941559469373));
#27920=CARTESIAN_POINT('Ctrl Pts',(32.5154955470851,20.839782064425,6.44317352589574));
#27921=CARTESIAN_POINT('Ctrl Pts',(33.6368017459444,21.8151237209333,9.49693145709774));
#27922=CARTESIAN_POINT('Ctrl Pts',(35.750231471854,23.4280644528074,11.6101975146502));
#27923=CARTESIAN_POINT('Ctrl Pts',(37.8636611977636,25.0410051846814,13.7234635722027));
#27924=CARTESIAN_POINT('Ctrl Pts',(40.5276779430448,27.0077867084411,14.4776794959001));
#27925=CARTESIAN_POINT('Ctrl Pts',(43.191694688326,28.9745682322008,15.2318954195974));
#27926=CARTESIAN_POINT('Ctrl Pts',(45.8557114336072,30.9413497559605,14.4776794959001));
#27927=CARTESIAN_POINT('Ctrl Pts',(32.4262389885814,19.4238236466306,1.04083408558608E-14));
#27928=CARTESIAN_POINT('Ctrl Pts',(32.310387384841,19.6040922608087,3.24562220582793));
#27929=CARTESIAN_POINT('Ctrl Pts',(33.3792081011658,20.5457035458242,6.16982677025168));
#27930=CARTESIAN_POINT('Ctrl Pts',(34.4480288174906,21.4873148308398,9.09403133467541));
#27931=CARTESIAN_POINT('Ctrl Pts',(36.4668829718392,23.0394755334782,11.1176436806954));
#27932=CARTESIAN_POINT('Ctrl Pts',(38.4857371261878,24.5916362361167,13.1412560267153));
#27933=CARTESIAN_POINT('Ctrl Pts',(41.0318200627227,26.4826263031063,13.8634749112255));
#27934=CARTESIAN_POINT('Ctrl Pts',(43.5779029992576,28.3736163700958,14.5856937957357));
#27935=CARTESIAN_POINT('Ctrl Pts',(46.1239859357924,30.2646064370854,13.8634749112255));
#27936=CARTESIAN_POINT('',(31.4039970697498,20.1821175312128,3.07395939422514E-30));
#27937=CARTESIAN_POINT('Origin',(32.9182507396844,21.1552751870372,0.));
#27938=CARTESIAN_POINT('Origin',(32.9182507396844,21.1552751870372,0.));
#27939=CARTESIAN_POINT('Ctrl Pts',(34.8604849513725,14.611382171278,0.));
#27940=CARTESIAN_POINT('Ctrl Pts',(34.7714674485863,14.8063033131397,3.24562220582793));
#27941=CARTESIAN_POINT('Ctrl Pts',(35.9634143688744,15.5862213055782,6.16982677025167));
#27942=CARTESIAN_POINT('Ctrl Pts',(37.1553612891626,16.3661392980167,9.09403133467541));
#27943=CARTESIAN_POINT('Ctrl Pts',(39.3745619185374,17.6151883402598,11.1176436806954));
#27944=CARTESIAN_POINT('Ctrl Pts',(41.5937625479122,18.8642373825028,13.1412560267153));
#27945=CARTESIAN_POINT('Ctrl Pts',(44.3830459768616,20.3736345158496,13.8634749112255));
#27946=CARTESIAN_POINT('Ctrl Pts',(47.1723294058109,21.8830316491965,14.5856937957357));
#27947=CARTESIAN_POINT('Ctrl Pts',(49.9616128347603,23.3924287825432,13.8634749112255));
#27948=CARTESIAN_POINT('Ctrl Pts',(37.1279962392258,15.3059217494161,0.));
#27949=CARTESIAN_POINT('Ctrl Pts',(37.0389787364397,15.5008428912778,2.70899372698068));
#27950=CARTESIAN_POINT('Ctrl Pts',(38.0191320633214,16.1840379904937,5.14971273833323));
#27951=CARTESIAN_POINT('Ctrl Pts',(38.9992853902032,16.8672330897095,7.59043174968577));
#27952=CARTESIAN_POINT('Ctrl Pts',(40.8368471514174,17.9419935007384,9.2794617117575));
#27953=CARTESIAN_POINT('Ctrl Pts',(42.6744089126316,19.0167539117673,10.9684916738292));
#27954=CARTESIAN_POINT('Ctrl Pts',(44.9877964569989,20.3088166768302,11.5712994880388));
#27955=CARTESIAN_POINT('Ctrl Pts',(47.3011840013661,21.600879441893,12.1741073022483));
#27956=CARTESIAN_POINT('Ctrl Pts',(49.6145715457333,22.8929422069559,11.5712994880388));
#27957=CARTESIAN_POINT('Ctrl Pts',(39.4874365476046,15.5447398754875,-1.05434036998093E-14));
#27958=CARTESIAN_POINT('Ctrl Pts',(39.3984190448184,15.7396610173492,2.19648874705823));
#27959=CARTESIAN_POINT('Ctrl Pts',(40.1762997089269,16.3304812866722,4.17545672685568));
#27960=CARTESIAN_POINT('Ctrl Pts',(40.9541803730353,16.9213015559953,6.15442470665313));
#27961=CARTESIAN_POINT('Ctrl Pts',(42.4272593902765,17.8296082752018,7.5239130403414));
#27962=CARTESIAN_POINT('Ctrl Pts',(43.9003384075178,18.7379149944084,8.89340137402966));
#27963=CARTESIAN_POINT('Ctrl Pts',(45.7592234042437,19.8224134008053,9.3821661014496));
#27964=CARTESIAN_POINT('Ctrl Pts',(47.6181084009697,20.9069118072022,9.87093082886953));
#27965=CARTESIAN_POINT('Ctrl Pts',(49.4769933976957,21.9914102135992,9.38216610144959));
#27966=CARTESIAN_POINT('Ctrl Pts',(41.848131348458,15.3186586437003,1.04083408558608E-14));
#27967=CARTESIAN_POINT('Ctrl Pts',(41.7591138456719,15.513579785562,1.72780310113342));
#27968=CARTESIAN_POINT('Ctrl Pts',(42.3520162221172,16.019923301465,3.28449990511991));
#27969=CARTESIAN_POINT('Ctrl Pts',(42.9449185985626,16.5262668173679,4.84119670910638));
#27970=CARTESIAN_POINT('Ctrl Pts',(44.0846782589592,17.2823516867885,5.91846432228298));
#27971=CARTESIAN_POINT('Ctrl Pts',(45.2244379193558,18.038436556209,6.99573193545956));
#27972=CARTESIAN_POINT('Ctrl Pts',(46.6676804765724,18.9331174206827,7.38020429521639));
#27973=CARTESIAN_POINT('Ctrl Pts',(48.1109230337889,19.8277982851563,7.76467665497322));
#27974=CARTESIAN_POINT('Ctrl Pts',(49.5541655910054,20.72247914963,7.38020429521639));
#27975=CARTESIAN_POINT('',(34.8604849513959,14.6113821712854,1.57949473064594E-9));
#27976=CARTESIAN_POINT('Origin',(40.1321417817281,-2.59935965651565,0.));
#27977=CARTESIAN_POINT('Ctrl Pts',(34.8604849513684,14.6113821714911,3.131065100813E-9));
#27978=CARTESIAN_POINT('Ctrl Pts',(34.8537643034671,14.6260983377859,0.24503815333575));
#27979=CARTESIAN_POINT('Ctrl Pts',(34.852749515407,14.6435771646296,0.490791160522261));
#27980=CARTESIAN_POINT('Ctrl Pts',(34.8575316463562,14.6638259110834,0.736766500726186));
#27981=CARTESIAN_POINT('Ctrl Pts',(34.862298077838,14.6840081820398,0.981934317701831));
#27982=CARTESIAN_POINT('Ctrl Pts',(34.872823533213,14.7069422331332,1.22732257376648));
#27983=CARTESIAN_POINT('Ctrl Pts',(34.8891527148323,14.7326128792076,1.47243294816424));
#27984=CARTESIAN_POINT('Ctrl Pts',(34.9054573041507,14.7582448644191,1.71717417803102));
#27985=CARTESIAN_POINT('Ctrl Pts',(34.9275482079567,14.7866052020688,1.96163791541673));
#27986=CARTESIAN_POINT('Ctrl Pts',(34.955423302389,14.8176563354396,2.20532408778614));
#27987=CARTESIAN_POINT('Ctrl Pts',(34.9832744897135,14.8486808377691,2.44880126242163));
#27988=CARTESIAN_POINT('Ctrl Pts',(35.0168999484379,14.882391488439,2.69150175431155));
#27989=CARTESIAN_POINT('Ctrl Pts',(35.0562505641471,14.9187287035022,2.93292951866921));
#27990=CARTESIAN_POINT('Ctrl Pts',(35.0955929476291,14.9550583167476,3.1743067758571));
#27991=CARTESIAN_POINT('Ctrl Pts',(35.1406580326364,14.9940133343939,3.41441139318471));
#27992=CARTESIAN_POINT('Ctrl Pts',(35.191350197822,15.0355127954202,3.6527571061477));
#27993=CARTESIAN_POINT('Ctrl Pts',(35.2421067311091,15.0770649517992,3.89140546668922));
#27994=CARTESIAN_POINT('Ctrl Pts',(35.2985045323757,15.1211679328245,4.12829002081298));
#27995=CARTESIAN_POINT('Ctrl Pts',(35.3604022296527,15.1677200855873,4.36293874377942));
#27996=CARTESIAN_POINT('Ctrl Pts',(35.4223630872643,15.2143197401098,4.59782690201577));
#27997=CARTESIAN_POINT('Ctrl Pts',(35.4898348974067,15.2633734552292,4.83047425895083));
#27998=CARTESIAN_POINT('Ctrl Pts',(35.5626325521737,15.3147603350321,5.06042975959551));
#27999=CARTESIAN_POINT('Ctrl Pts',(35.6356430387473,15.3662974499285,5.2910575599842));
#28000=CARTESIAN_POINT('Ctrl Pts',(35.7140103401313,15.4201812613939,5.51897736305799));
#28001=CARTESIAN_POINT('Ctrl Pts',(35.7975071039183,15.4762725955035,5.74376259354438));
#28002=CARTESIAN_POINT('Ctrl Pts',(35.8507471233726,15.5120380980664,5.8870923407269));
#28003=CARTESIAN_POINT('Ctrl Pts',(35.9060718261753,15.5487007750603,6.02914825314227));
#28004=CARTESIAN_POINT('Ctrl Pts',(35.9634143689083,15.586221305588,6.16982677023484));
#28005=CARTESIAN_POINT('Ctrl Pts',(36.0533291627655,15.645054601201,6.39041482339096));
#28006=CARTESIAN_POINT('Ctrl Pts',(36.1486520067523,15.7065142910191,6.60890054011815));
#28007=CARTESIAN_POINT('Ctrl Pts',(36.2492721362563,15.7705155506317,6.82480412008057));
#28008=CARTESIAN_POINT('Ctrl Pts',(36.3496651101704,15.8343723238084,7.0402202855931));
#28009=CARTESIAN_POINT('Ctrl Pts',(36.4553314094028,15.9007591428902,7.25306552029658));
#28010=CARTESIAN_POINT('Ctrl Pts',(36.5661159087968,15.9695695446607,7.46287566269441));
#28011=CARTESIAN_POINT('Ctrl Pts',(36.6767222213247,16.0382692711118,7.67234834441893));
#28012=CARTESIAN_POINT('Ctrl Pts',(36.7924301575637,16.1093847013531,7.87879526533028));
#28013=CARTESIAN_POINT('Ctrl Pts',(36.9130417770841,16.1827888425355,8.08177334612183));
#28014=CARTESIAN_POINT('Ctrl Pts',(37.0335376654153,16.2561225498029,8.28455666214065));
#28015=CARTESIAN_POINT('Ctrl Pts',(37.1589276519414,16.3317404631312,8.48387739272776));
#28016=CARTESIAN_POINT('Ctrl Pts',(37.288973128395,16.4094964608243,8.67931873610986));
#28017=CARTESIAN_POINT('Ctrl Pts',(37.4190248596921,16.4872561983753,8.87476947970367));
#28018=CARTESIAN_POINT('Ctrl Pts',(37.5537323016291,16.5671540886063,9.06634009532686));
#28019=CARTESIAN_POINT('Ctrl Pts',(37.6928185909662,16.6490263722355,9.25364450340825));
#28020=CARTESIAN_POINT('Ctrl Pts',(37.8319559027359,16.730928689904,9.44101762226329));
#28021=CARTESIAN_POINT('Ctrl Pts',(37.9754750005784,16.814806690878,9.62412107874858));
#28022=CARTESIAN_POINT('Ctrl Pts',(38.1230642366182,16.900481032106,9.80260437465942));
#28023=CARTESIAN_POINT('Ctrl Pts',(38.270894221272,16.9862951259302,9.98137881379502));
#28024=CARTESIAN_POINT('Ctrl Pts',(38.4228073220804,17.0739112501813,10.1555177270907));
#28025=CARTESIAN_POINT('Ctrl Pts',(38.5784601754,17.1631362396558,10.3247095747691));
#28026=CARTESIAN_POINT('Ctrl Pts',(38.6234491187501,17.1889252818176,10.3736117457744));
#28027=CARTESIAN_POINT('Ctrl Pts',(38.6687503076455,17.2148486564428,10.4221009095751));
#28028=CARTESIAN_POINT('Ctrl Pts',(38.714355041992,17.2409015314888,10.4701702229111));
#28029=CARTESIAN_POINT('Ctrl Pts',(38.981767758745,21.5951194116466,0.));
#28030=CARTESIAN_POINT('Ctrl Pts',(38.8927502559589,21.7900405535082,1.72780310113343));
#28031=CARTESIAN_POINT('Ctrl Pts',(39.4856526324043,22.2963840694112,3.28449990511992));
#28032=CARTESIAN_POINT('Ctrl Pts',(40.0785550088497,22.8027275853141,4.84119670910638));
#28033=CARTESIAN_POINT('Ctrl Pts',(41.2183146692462,23.5588124547347,5.91846432228298));
#28034=CARTESIAN_POINT('Ctrl Pts',(42.3580743296429,24.3148973241552,6.99573193545956));
#28035=CARTESIAN_POINT('Ctrl Pts',(43.8013168868594,25.2095781886289,7.3802042952164));
#28036=CARTESIAN_POINT('Ctrl Pts',(45.2445594440759,26.1042590531026,7.76467665497323));
#28037=CARTESIAN_POINT('Ctrl Pts',(46.6878020012925,26.9989399175762,7.38020429521639));
#28038=CARTESIAN_POINT('Ctrl Pts',(37.6067022235299,19.6629735993419,0.));
#28039=CARTESIAN_POINT('Ctrl Pts',(37.5176847207438,19.8578947412036,2.19648874705823));
#28040=CARTESIAN_POINT('Ctrl Pts',(38.2955653848522,20.4487150105266,4.17545672685568));
#28041=CARTESIAN_POINT('Ctrl Pts',(39.0734460489607,21.0395352798497,6.15442470665314));
#28042=CARTESIAN_POINT('Ctrl Pts',(40.5465250662019,21.9478419990562,7.5239130403414));
#28043=CARTESIAN_POINT('Ctrl Pts',(42.0196040834431,22.8561487182628,8.89340137402969));
#28044=CARTESIAN_POINT('Ctrl Pts',(43.8784890801691,23.9406471246597,9.38216610144961));
#28045=CARTESIAN_POINT('Ctrl Pts',(45.7373740768951,25.0251455310566,9.87093082886954));
#28046=CARTESIAN_POINT('Ctrl Pts',(47.5962590736211,26.1096439374536,9.38216610144961));
#28047=CARTESIAN_POINT('Ctrl Pts',(35.8811107143584,18.036220203889,0.));
#28048=CARTESIAN_POINT('Ctrl Pts',(35.7920932115723,18.2311413457506,2.70899372698069));
#28049=CARTESIAN_POINT('Ctrl Pts',(36.772246538454,18.9143364449665,5.14971273833323));
#28050=CARTESIAN_POINT('Ctrl Pts',(37.7523998653357,19.5975315441823,7.59043174968578));
#28051=CARTESIAN_POINT('Ctrl Pts',(39.5899616265499,20.6722919552112,9.27946171175751));
#28052=CARTESIAN_POINT('Ctrl Pts',(41.4275233877641,21.7470523662401,10.9684916738292));
#28053=CARTESIAN_POINT('Ctrl Pts',(43.7409109321314,23.039115131303,11.5712994880388));
#28054=CARTESIAN_POINT('Ctrl Pts',(46.0542984764987,24.3311778963658,12.1741073022483));
#28055=CARTESIAN_POINT('Ctrl Pts',(48.367686020866,25.6232406614287,11.5712994880388));
#28056=CARTESIAN_POINT('Ctrl Pts',(33.8713086176154,16.777376211144,0.));
#28057=CARTESIAN_POINT('Ctrl Pts',(33.7822911148293,16.9722973530056,3.24562220582793));
#28058=CARTESIAN_POINT('Ctrl Pts',(34.9742380351174,17.7522153454442,6.16982677025167));
#28059=CARTESIAN_POINT('Ctrl Pts',(36.1661849554055,18.5321333378827,9.09403133467541));
#28060=CARTESIAN_POINT('Ctrl Pts',(38.3853855847803,19.7811823801258,11.1176436806954));
#28061=CARTESIAN_POINT('Ctrl Pts',(40.6045862141551,21.0302314223688,13.1412560267153));
#28062=CARTESIAN_POINT('Ctrl Pts',(43.3938696431045,22.5396285557156,13.8634749112255));
#28063=CARTESIAN_POINT('Ctrl Pts',(46.1831530720539,24.0490256890624,14.5856937957357));
#28064=CARTESIAN_POINT('Ctrl Pts',(48.9724365010033,25.5584228224092,13.8634749112255));
#28065=CARTESIAN_POINT('',(33.8713086176154,16.777376211144,0.));
#28066=CARTESIAN_POINT('Ctrl Pts',(33.8713086176154,16.777376211144,0.));
#28067=CARTESIAN_POINT('Ctrl Pts',(33.7822911148293,16.9722973530056,3.24562220582793));
#28068=CARTESIAN_POINT('Ctrl Pts',(34.9742380351174,17.7522153454441,6.16982677025168));
#28069=CARTESIAN_POINT('Ctrl Pts',(35.969320654379,18.4033205461165,8.61106394926976));
#28070=CARTESIAN_POINT('Ctrl Pts',(37.7050538275442,19.39539586064,10.4489096280657));
#28071=CARTESIAN_POINT('Origin',(24.316498867974,32.0320676419189,0.));
#28072=CARTESIAN_POINT('Ctrl Pts',(33.8713086176154,16.7773762111439,0.));
#28073=CARTESIAN_POINT('Ctrl Pts',(33.7822911148293,16.9722973530056,3.24562220582793));
#28074=CARTESIAN_POINT('Ctrl Pts',(34.9742380351174,17.7522153454441,6.16982677025168));
#28075=CARTESIAN_POINT('Ctrl Pts',(36.1661849554055,18.5321333378827,9.09403133467541));
#28076=CARTESIAN_POINT('Ctrl Pts',(38.3853855847803,19.7811823801258,11.1176436806954));
#28077=CARTESIAN_POINT('Ctrl Pts',(40.6045862141551,21.0302314223688,13.1412560267153));
#28078=CARTESIAN_POINT('Ctrl Pts',(43.3938696431045,22.5396285557156,13.8634749112255));
#28079=CARTESIAN_POINT('Ctrl Pts',(46.1831530720539,24.0490256890624,14.5856937957357));
#28080=CARTESIAN_POINT('Ctrl Pts',(48.9724365010033,25.5584228224092,13.8634749112255));
#28081=CARTESIAN_POINT('Ctrl Pts',(33.5949933606691,15.865866540993,0.));
#28082=CARTESIAN_POINT('Ctrl Pts',(33.505975857883,16.0607876828547,3.38941559469372));
#28083=CARTESIAN_POINT('Ctrl Pts',(34.7546743665352,16.8666232572808,6.44317352589574));
#28084=CARTESIAN_POINT('Ctrl Pts',(36.0033728751873,17.6724588317069,9.49693145709774));
#28085=CARTESIAN_POINT('Ctrl Pts',(38.3248363332022,18.9682097429542,11.6101975146502));
#28086=CARTESIAN_POINT('Ctrl Pts',(40.646299791217,20.2639606542015,13.7234635722027));
#28087=CARTESIAN_POINT('Ctrl Pts',(43.563102881699,21.8315940656521,14.4776794959001));
#28088=CARTESIAN_POINT('Ctrl Pts',(46.479905972181,23.3992274771026,15.2318954195974));
#28089=CARTESIAN_POINT('Ctrl Pts',(49.3967090626629,24.9668608885532,14.4776794959001));
#28090=CARTESIAN_POINT('Ctrl Pts',(33.990663894172,14.9994689250466,0.));
#28091=CARTESIAN_POINT('Ctrl Pts',(33.9016463913858,15.1943900669083,3.38941559469372));
#28092=CARTESIAN_POINT('Ctrl Pts',(35.150344900038,16.0002256413344,6.44317352589574));
#28093=CARTESIAN_POINT('Ctrl Pts',(36.3990434086901,16.8060612157605,9.49693145709774));
#28094=CARTESIAN_POINT('Ctrl Pts',(38.720506866705,18.1018121270078,11.6101975146502));
#28095=CARTESIAN_POINT('Ctrl Pts',(41.0419703247199,19.3975630382551,13.7234635722027));
#28096=CARTESIAN_POINT('Ctrl Pts',(43.9587734152018,20.9651964497057,14.4776794959001));
#28097=CARTESIAN_POINT('Ctrl Pts',(46.8755765056838,22.5328298611562,15.2318954195974));
#28098=CARTESIAN_POINT('Ctrl Pts',(49.7923795961658,24.1004632726068,14.4776794959001));
#28099=CARTESIAN_POINT('Ctrl Pts',(34.8604849513725,14.611382171278,0.));
#28100=CARTESIAN_POINT('Ctrl Pts',(34.7714674485863,14.8063033131397,3.24562220582793));
#28101=CARTESIAN_POINT('Ctrl Pts',(35.9634143688744,15.5862213055782,6.16982677025167));
#28102=CARTESIAN_POINT('Ctrl Pts',(37.1553612891626,16.3661392980167,9.09403133467541));
#28103=CARTESIAN_POINT('Ctrl Pts',(39.3745619185374,17.6151883402598,11.1176436806954));
#28104=CARTESIAN_POINT('Ctrl Pts',(41.5937625479122,18.8642373825028,13.1412560267153));
#28105=CARTESIAN_POINT('Ctrl Pts',(44.3830459768616,20.3736345158497,13.8634749112255));
#28106=CARTESIAN_POINT('Ctrl Pts',(47.1723294058109,21.8830316491965,14.5856937957357));
#28107=CARTESIAN_POINT('Ctrl Pts',(49.9616128347603,23.3924287825433,13.8634749112255));
#28108=CARTESIAN_POINT('',(33.9565644528671,15.5074379108486,5.72595023245623E-30));
#28109=CARTESIAN_POINT('Origin',(35.5938999782225,16.2551894587635,0.));
#28110=CARTESIAN_POINT('Origin',(35.5938999782225,16.2551894587635,0.));
#28111=CARTESIAN_POINT('Ctrl Pts',(36.5850719698906,9.50149509066482,0.));
#28112=CARTESIAN_POINT('Ctrl Pts',(36.5247007077103,9.70710072786793,3.24562220582793));
#28113=CARTESIAN_POINT('Ctrl Pts',(37.8155092299557,10.3094485465012,6.16982677025168));
#28114=CARTESIAN_POINT('Ctrl Pts',(39.1063177522012,10.9117963651344,9.09403133467541));
#28115=CARTESIAN_POINT('Ctrl Pts',(41.4806883314343,11.832306710442,11.1176436806954));
#28116=CARTESIAN_POINT('Ctrl Pts',(43.8550589106673,12.7528170557496,13.1412560267153));
#28117=CARTESIAN_POINT('Ctrl Pts',(46.830761065047,13.8498942825606,13.8634749112255));
#28118=CARTESIAN_POINT('Ctrl Pts',(49.8064632194267,14.9469715093716,14.5856937957357));
#28119=CARTESIAN_POINT('Ctrl Pts',(52.7821653738064,16.0440487361825,13.8634749112255));
#28120=CARTESIAN_POINT('Ctrl Pts',(38.928346550052,9.86626475512722,0.));
#28121=CARTESIAN_POINT('Ctrl Pts',(38.8679752878718,10.0718703923303,2.70899372698069));
#28122=CARTESIAN_POINT('Ctrl Pts',(39.9353808672042,10.6086211883239,5.14971273833323));
#28123=CARTESIAN_POINT('Ctrl Pts',(41.0027864465367,11.1453719843175,7.59043174968578));
#28124=CARTESIAN_POINT('Ctrl Pts',(42.9745988326451,11.9476805791743,9.27946171175751));
#28125=CARTESIAN_POINT('Ctrl Pts',(44.9464112187536,12.7499891740311,10.9684916738293));
#28126=CARTESIAN_POINT('Ctrl Pts',(47.4201315169974,13.6996712289063,11.5712994880388));
#28127=CARTESIAN_POINT('Ctrl Pts',(49.8938518152413,14.6493532837814,12.1741073022483));
#28128=CARTESIAN_POINT('Ctrl Pts',(52.3675721134852,15.5990353386566,11.5712994880388));
#28129=CARTESIAN_POINT('Ctrl Pts',(41.2977585211121,9.7668686911201,0.));
#28130=CARTESIAN_POINT('Ctrl Pts',(41.2373872589318,9.97247432832318,2.19648874705823));
#28131=CARTESIAN_POINT('Ctrl Pts',(42.0914327105682,10.4465769382885,4.17545672685568));
#28132=CARTESIAN_POINT('Ctrl Pts',(42.9454781622046,10.9206795482538,6.15442470665314));
#28133=CARTESIAN_POINT('Ctrl Pts',(44.5328288829012,11.6101000126265,7.52391304034141));
#28134=CARTESIAN_POINT('Ctrl Pts',(46.1201796035979,12.2995204769992,8.89340137402968));
#28135=CARTESIAN_POINT('Ctrl Pts',(48.1144840466621,13.1084333356589,9.38216610144961));
#28136=CARTESIAN_POINT('Ctrl Pts',(50.1087884897263,13.9173461943186,9.87093082886955));
#28137=CARTESIAN_POINT('Ctrl Pts',(52.1030929327904,14.7262590529783,9.38216610144962));
#28138=CARTESIAN_POINT('Ctrl Pts',(43.6022501387952,9.20712674149426,0.));
#28139=CARTESIAN_POINT('Ctrl Pts',(43.5418788766149,9.41273237869738,1.72780310113342));
#28140=CARTESIAN_POINT('Ctrl Pts',(44.2008065573392,9.82954324187981,3.28449990511991));
#28141=CARTESIAN_POINT('Ctrl Pts',(44.8597342380634,10.2463541050622,4.84119670910639));
#28142=CARTESIAN_POINT('Ctrl Pts',(46.0954948844274,10.8325384089567,5.91846432228298));
#28143=CARTESIAN_POINT('Ctrl Pts',(47.3312555307913,11.4187227128512,6.99573193545957));
#28144=CARTESIAN_POINT('Ctrl Pts',(48.8871343222931,12.0989021850284,7.3802042952164));
#28145=CARTESIAN_POINT('Ctrl Pts',(50.4430131137949,12.7790816572055,7.76467665497322));
#28146=CARTESIAN_POINT('Ctrl Pts',(51.9988919052966,13.4592611293828,7.38020429521639));
#28147=CARTESIAN_POINT('',(36.5850719699957,9.50149509062496,1.57949199304179E-9));
#28148=CARTESIAN_POINT('Origin',(39.3537269950291,-8.28430119040666,1.04083408558608E-14));
#28149=CARTESIAN_POINT('Ctrl Pts',(36.5850719699169,9.50149509087633,3.13105402820441E-9));
#28150=CARTESIAN_POINT('Ctrl Pts',(36.5805140573471,9.51701791573643,0.245038153335483));
#28151=CARTESIAN_POINT('Ctrl Pts',(36.5819970947817,9.53446325272387,0.490791160521737));
#28152=CARTESIAN_POINT('Ctrl Pts',(36.5896122476099,9.5538253279424,0.736766500725404));
#28153=CARTESIAN_POINT('Ctrl Pts',(36.597202400319,9.57312383855536,0.981934317701064));
#28154=CARTESIAN_POINT('Ctrl Pts',(36.6108845775071,9.59432652559737,1.22732257376573));
#28155=CARTESIAN_POINT('Ctrl Pts',(36.6307008654467,9.61741199666751,1.4724329481635));
#28156=CARTESIAN_POINT('Ctrl Pts',(36.650487309385,9.64046270023582,1.71717417803028));
#28157=CARTESIAN_POINT('Ctrl Pts',(36.6763894565088,9.66539050713801,1.96163791541599));
#28158=CARTESIAN_POINT('Ctrl Pts',(36.7083998596961,9.69215854518714,2.20532408778539));
#28159=CARTESIAN_POINT('Ctrl Pts',(36.7403828091233,9.71890362559676,2.44880126242082));
#28160=CARTESIAN_POINT('Ctrl Pts',(36.77846353496,9.74748574872929,2.69150175431068));
#28161=CARTESIAN_POINT('Ctrl Pts',(36.8225849430252,9.7778529268265,2.93292951866827));
#28162=CARTESIAN_POINT('Ctrl Pts',(36.8666971208038,9.8082137520495,3.17430677585629));
#28163=CARTESIAN_POINT('Ctrl Pts',(36.9168473852605,9.84035883350012,3.41441139318404));
#28164=CARTESIAN_POINT('Ctrl Pts',(36.972929566381,9.87422164256039,3.65275710614716));
#28165=CARTESIAN_POINT('Ctrl Pts',(37.0290829597591,9.90812745007459,3.8914054666886));
#28166=CARTESIAN_POINT('Ctrl Pts',(37.0911832213397,9.94375528237804,4.12829002081229));
#28167=CARTESIAN_POINT('Ctrl Pts',(37.1590759513992,9.98102464057091,4.36293874377867));
#28168=CARTESIAN_POINT('Ctrl Pts',(37.2270379591175,10.0183320283713,4.59782690201507));
#28169=CARTESIAN_POINT('Ctrl Pts',(37.3008040750528,10.0572842076519,4.83047425895017));
#28170=CARTESIAN_POINT('Ctrl Pts',(37.3801738701484,10.0977878566474,5.06042975959489));
#28171=CARTESIAN_POINT('Ctrl Pts',(37.4597757114127,10.1384099224355,5.29105755998366));
#28172=CARTESIAN_POINT('Ctrl Pts',(37.5450138125792,10.180592444572,5.51897736305752));
#28173=CARTESIAN_POINT('Ctrl Pts',(37.6356433288455,10.2242300213427,5.74376259354398));
#28174=CARTESIAN_POINT('Ctrl Pts',(37.6934314033807,10.2520546379008,5.88709234072663));
#28175=CARTESIAN_POINT('Ctrl Pts',(37.7534106234275,10.2804706155742,6.02914825314214));
#28176=CARTESIAN_POINT('Ctrl Pts',(37.8155092299907,10.3094485465061,6.16982677023484));
#28177=CARTESIAN_POINT('Ctrl Pts',(37.9128816718431,10.3548867946542,6.39041482339091));
#28178=CARTESIAN_POINT('Ctrl Pts',(38.0159808925391,10.4021550583218,6.60890054011806));
#28179=CARTESIAN_POINT('Ctrl Pts',(38.124685183118,10.4511851399362,6.82480412008043));
#28180=CARTESIAN_POINT('Ctrl Pts',(38.2331440676596,10.5001045333895,7.04022028559285));
#28181=CARTESIAN_POINT('Ctrl Pts',(38.347182665745,10.5507777480887,7.25306552029621));
#28182=CARTESIAN_POINT('Ctrl Pts',(38.4666322798727,10.6031214810711,7.46287566269393));
#28183=CARTESIAN_POINT('Ctrl Pts',(38.5858897700795,10.6553810238844,7.67234834441863));
#28184=CARTESIAN_POINT('Ctrl Pts',(38.7105407473183,10.7093056453531,7.87879526533015));
#28185=CARTESIAN_POINT('Ctrl Pts',(38.8403712129407,10.7647978150924,8.08177334612187));
#28186=CARTESIAN_POINT('Ctrl Pts',(38.9700771015594,10.820236738098,8.28455666214102));
#28187=CARTESIAN_POINT('Ctrl Pts',(39.1049523499261,10.8772401144471,8.48387739272847));
#28188=CARTESIAN_POINT('Ctrl Pts',(39.2447399831763,10.935697267249,8.67931873611088));
#28189=CARTESIAN_POINT('Ctrl Pts',(39.3845343398416,10.9941572316853,8.87476947970464));
#28190=CARTESIAN_POINT('Ctrl Pts',(39.5292413095784,11.0540710087835,9.06634009532779));
#28191=CARTESIAN_POINT('Ctrl Pts',(39.6785635418397,11.1153159078424,9.25364450340913));
#28192=CARTESIAN_POINT('Ctrl Pts',(39.8279405514883,11.1765832739882,9.44101762226425));
#28193=CARTESIAN_POINT('Ctrl Pts',(39.9819359159956,11.2391826206559,9.62412107874963));
#28194=CARTESIAN_POINT('Ctrl Pts',(40.1402156364348,11.3029807823645,9.80260437466055));
#28195=CARTESIAN_POINT('Ctrl Pts',(40.2987535438823,11.3668830120894,9.9813788137962));
#28196=CARTESIAN_POINT('Ctrl Pts',(40.461589462918,11.4319878421545,10.155517727092));
#28197=CARTESIAN_POINT('Ctrl Pts',(40.6283560345709,11.498152939241,10.3247095747704));
#28198=CARTESIAN_POINT('Ctrl Pts',(40.6765572187104,11.5172768919413,10.3736117457753));
#28199=CARTESIAN_POINT('Ctrl Pts',(40.7250865876886,11.5364893726198,10.4221009095756));
#28200=CARTESIAN_POINT('Ctrl Pts',(40.7739348422944,11.5557868365697,10.4701702229111));
#28201=CARTESIAN_POINT('Ctrl Pts',(41.6582954965894,15.8276282594343,0.));
#28202=CARTESIAN_POINT('Ctrl Pts',(41.5979242344091,16.0332338966374,1.72780310113343));
#28203=CARTESIAN_POINT('Ctrl Pts',(42.2568519151334,16.4500447598199,3.28449990511991));
#28204=CARTESIAN_POINT('Ctrl Pts',(42.9157795958577,16.8668556230023,4.84119670910639));
#28205=CARTESIAN_POINT('Ctrl Pts',(44.1515402422216,17.4530399268967,5.91846432228298));
#28206=CARTESIAN_POINT('Ctrl Pts',(45.3873008885855,18.0392242307912,6.99573193545956));
#28207=CARTESIAN_POINT('Ctrl Pts',(46.9431796800873,18.7194037029684,7.38020429521639));
#28208=CARTESIAN_POINT('Ctrl Pts',(48.4990584715891,19.3995831751456,7.76467665497322));
#28209=CARTESIAN_POINT('Ctrl Pts',(50.0549372630908,20.0797626473228,7.3802042952164));
#28210=CARTESIAN_POINT('Ctrl Pts',(40.0222531270435,14.110841134834,0.));
#28211=CARTESIAN_POINT('Ctrl Pts',(39.9618818648632,14.3164467720371,2.19648874705823));
#28212=CARTESIAN_POINT('Ctrl Pts',(40.8159273164996,14.7905493820025,4.17545672685568));
#28213=CARTESIAN_POINT('Ctrl Pts',(41.669972768136,15.2646519919678,6.15442470665315));
#28214=CARTESIAN_POINT('Ctrl Pts',(43.2573234888327,15.9540724563405,7.52391304034141));
#28215=CARTESIAN_POINT('Ctrl Pts',(44.8446742095293,16.6434929207132,8.89340137402968));
#28216=CARTESIAN_POINT('Ctrl Pts',(46.8389786525935,17.4524057793729,9.38216610144961));
#28217=CARTESIAN_POINT('Ctrl Pts',(48.8332830956577,18.2613186380326,9.87093082886955));
#28218=CARTESIAN_POINT('Ctrl Pts',(50.8275875387219,19.0702314966922,9.38216610144961));
#28219=CARTESIAN_POINT('Ctrl Pts',(38.0827145049534,12.7462230199156,0.));
#28220=CARTESIAN_POINT('Ctrl Pts',(38.0223432427731,12.9518286571187,2.7089937269807));
#28221=CARTESIAN_POINT('Ctrl Pts',(39.0897488221056,13.4885794531123,5.14971273833323));
#28222=CARTESIAN_POINT('Ctrl Pts',(40.1571544014381,14.0253302491059,7.59043174968579));
#28223=CARTESIAN_POINT('Ctrl Pts',(42.1289667875465,14.8276388439627,9.27946171175752));
#28224=CARTESIAN_POINT('Ctrl Pts',(44.1007791736549,15.6299474388195,10.9684916738293));
#28225=CARTESIAN_POINT('Ctrl Pts',(46.5744994718988,16.5796294936946,11.5712994880388));
#28226=CARTESIAN_POINT('Ctrl Pts',(49.0482197701427,17.5293115485698,12.1741073022483));
#28227=CARTESIAN_POINT('Ctrl Pts',(51.5219400683865,18.4789936034449,11.5712994880388));
#28228=CARTESIAN_POINT('Ctrl Pts',(35.9142171164211,11.7862169042729,0.));
#28229=CARTESIAN_POINT('Ctrl Pts',(35.8538458542409,11.991822541476,3.24562220582793));
#28230=CARTESIAN_POINT('Ctrl Pts',(37.1446543764862,12.5941703601092,6.16982677025168));
#28231=CARTESIAN_POINT('Ctrl Pts',(38.4354628987317,13.1965181787425,9.09403133467541));
#28232=CARTESIAN_POINT('Ctrl Pts',(40.8098334779648,14.1170285240501,11.1176436806954));
#28233=CARTESIAN_POINT('Ctrl Pts',(43.1842040571978,15.0375388693576,13.1412560267153));
#28234=CARTESIAN_POINT('Ctrl Pts',(46.1599062115776,16.1346160961686,13.8634749112255));
#28235=CARTESIAN_POINT('Ctrl Pts',(49.1356083659572,17.2316933229796,14.5856937957357));
#28236=CARTESIAN_POINT('Ctrl Pts',(52.1113105203369,18.3287705497906,13.8634749112255));
#28237=CARTESIAN_POINT('',(35.9142171164211,11.7862169042729,0.));
#28238=CARTESIAN_POINT('Ctrl Pts',(35.9142171164211,11.7862169042729,0.));
#28239=CARTESIAN_POINT('Ctrl Pts',(35.8538458542409,11.991822541476,3.24562220582793));
#28240=CARTESIAN_POINT('Ctrl Pts',(37.1446543764862,12.5941703601092,6.16982677025168));
#28241=CARTESIAN_POINT('Ctrl Pts',(38.222270420807,13.0970332266261,8.61106394926975));
#28242=CARTESIAN_POINT('Ctrl Pts',(40.0815233709314,13.8319900590777,10.4489096280657));
#28243=CARTESIAN_POINT('Origin',(28.6276304970128,28.2454287759835,0.));
#28244=CARTESIAN_POINT('Ctrl Pts',(35.9142171164211,11.7862169042729,0.));
#28245=CARTESIAN_POINT('Ctrl Pts',(35.8538458542409,11.991822541476,3.24562220582793));
#28246=CARTESIAN_POINT('Ctrl Pts',(37.1446543764862,12.5941703601092,6.16982677025167));
#28247=CARTESIAN_POINT('Ctrl Pts',(38.4354628987317,13.1965181787425,9.0940313346754));
#28248=CARTESIAN_POINT('Ctrl Pts',(40.8098334779648,14.11702852405,11.1176436806954));
#28249=CARTESIAN_POINT('Ctrl Pts',(43.1842040571979,15.0375388693576,13.1412560267153));
#28250=CARTESIAN_POINT('Ctrl Pts',(46.1599062115776,16.1346160961686,13.8634749112255));
#28251=CARTESIAN_POINT('Ctrl Pts',(49.1356083659572,17.2316933229796,14.5856937957357));
#28252=CARTESIAN_POINT('Ctrl Pts',(52.1113105203369,18.3287705497906,13.8634749112255));
#28253=CARTESIAN_POINT('Ctrl Pts',(35.5109929990849,10.9233088493804,6.24500451351651E-15));
#28254=CARTESIAN_POINT('Ctrl Pts',(35.4506217369045,11.1289144865835,3.38941559469373));
#28255=CARTESIAN_POINT('Ctrl Pts',(36.8012926546625,11.74883949047,6.44317352589573));
#28256=CARTESIAN_POINT('Ctrl Pts',(38.1519635724205,12.3687644943564,9.49693145709774));
#28257=CARTESIAN_POINT('Ctrl Pts',(40.6342024610833,13.3209478330611,11.6101975146502));
#28258=CARTESIAN_POINT('Ctrl Pts',(43.116441349746,14.2731311717657,13.7234635722027));
#28259=CARTESIAN_POINT('Ctrl Pts',(46.226653085872,15.4097039753314,14.4776794959001));
#28260=CARTESIAN_POINT('Ctrl Pts',(49.336864821998,16.5462767788972,15.2318954195974));
#28261=CARTESIAN_POINT('Ctrl Pts',(52.4470765581241,17.682849582463,14.4776794959001));
#28262=CARTESIAN_POINT('Ctrl Pts',(35.7793349404726,10.0094201239371,0.));
#28263=CARTESIAN_POINT('Ctrl Pts',(35.7189636782923,10.2150257611402,3.38941559469373));
#28264=CARTESIAN_POINT('Ctrl Pts',(37.0696345960503,10.8349507650267,6.44317352589573));
#28265=CARTESIAN_POINT('Ctrl Pts',(38.4203055138083,11.4548757689132,9.49693145709775));
#28266=CARTESIAN_POINT('Ctrl Pts',(40.902544402471,12.4070591076178,11.6101975146502));
#28267=CARTESIAN_POINT('Ctrl Pts',(43.3847832911339,13.3592424463224,13.7234635722027));
#28268=CARTESIAN_POINT('Ctrl Pts',(46.4949950272598,14.4958152498882,14.4776794959001));
#28269=CARTESIAN_POINT('Ctrl Pts',(49.6052067633858,15.632388053454,15.2318954195974));
#28270=CARTESIAN_POINT('Ctrl Pts',(52.7154184995118,16.7689608570197,14.4776794959001));
#28271=CARTESIAN_POINT('Ctrl Pts',(36.5850719698906,9.50149509066483,0.));
#28272=CARTESIAN_POINT('Ctrl Pts',(36.5247007077103,9.70710072786794,3.24562220582793));
#28273=CARTESIAN_POINT('Ctrl Pts',(37.8155092299557,10.3094485465012,6.16982677025168));
#28274=CARTESIAN_POINT('Ctrl Pts',(39.1063177522012,10.9117963651344,9.09403133467541));
#28275=CARTESIAN_POINT('Ctrl Pts',(41.4806883314343,11.832306710442,11.1176436806954));
#28276=CARTESIAN_POINT('Ctrl Pts',(43.8550589106673,12.7528170557496,13.1412560267153));
#28277=CARTESIAN_POINT('Ctrl Pts',(46.830761065047,13.8498942825606,13.8634749112255));
#28278=CARTESIAN_POINT('Ctrl Pts',(49.8064632194267,14.9469715093716,14.5856937957357));
#28279=CARTESIAN_POINT('Ctrl Pts',(52.7821653738064,16.0440487361826,13.8634749112255));
#28280=CARTESIAN_POINT('',(35.817874106391,10.5170715743152,8.26137723558795E-30));
#28281=CARTESIAN_POINT('Origin',(37.5449600575355,11.0241949492048,0.));
#28282=CARTESIAN_POINT('Origin',(37.5449600575355,11.0241949492048,0.));
#28283=CARTESIAN_POINT('Ctrl Pts',(37.5648924257372,4.19818497005498,0.));
#28284=CARTESIAN_POINT('Ctrl Pts',(37.5343963889644,4.41028956474376,3.24562220582792));
#28285=CARTESIAN_POINT('Ctrl Pts',(38.8977893740385,4.82280514501199,6.16982677025168));
#28286=CARTESIAN_POINT('Ctrl Pts',(40.2611823591128,5.23532072528026,9.09403133467541));
#28287=CARTESIAN_POINT('Ctrl Pts',(42.7423875503303,5.80855343755452,11.1176436806954));
#28288=CARTESIAN_POINT('Ctrl Pts',(45.2235927415478,6.38178614982881,13.1412560267153));
#28289=CARTESIAN_POINT('Ctrl Pts',(48.325136906711,7.04421014147558,13.8634749112255));
#28290=CARTESIAN_POINT('Ctrl Pts',(51.4266810718742,7.70663413312235,14.5856937957357));
#28291=CARTESIAN_POINT('Ctrl Pts',(54.5282252370374,8.36905812476912,13.8634749112255));
#28292=CARTESIAN_POINT('Ctrl Pts',(39.9362279852005,4.225759062382,0.));
#28293=CARTESIAN_POINT('Ctrl Pts',(39.9057319484277,4.43786365707078,2.7089937269807));
#28294=CARTESIAN_POINT('Ctrl Pts',(41.0386604807592,4.8172434514972,5.14971273833323));
#28295=CARTESIAN_POINT('Ctrl Pts',(42.1715890130907,5.19662324592361,7.59043174968578));
#28296=CARTESIAN_POINT('Ctrl Pts',(44.2375116101495,5.71014733528395,9.27946171175752));
#28297=CARTESIAN_POINT('Ctrl Pts',(46.3034342072083,6.22367142464428,10.9684916738293));
#28298=CARTESIAN_POINT('Ctrl Pts',(48.8871294476768,6.81163998135133,11.5712994880388));
#28299=CARTESIAN_POINT('Ctrl Pts',(51.4708246881453,7.39960853805837,12.1741073022483));
#28300=CARTESIAN_POINT('Ctrl Pts',(54.0545199286137,7.98757709476541,11.5712994880388));
#28301=CARTESIAN_POINT('Ctrl Pts',(42.2673772240309,3.79017222552498,0.));
#28302=CARTESIAN_POINT('Ctrl Pts',(42.236881187258,4.00227682021375,2.19648874705823));
#28303=CARTESIAN_POINT('Ctrl Pts',(43.1497055238908,4.35001040888147,4.17545672685568));
#28304=CARTESIAN_POINT('Ctrl Pts',(44.0625298605235,4.69774399754918,6.15442470665315));
#28305=CARTESIAN_POINT('Ctrl Pts',(45.7318384015437,5.15424359455786,7.52391304034141));
#28306=CARTESIAN_POINT('Ctrl Pts',(47.401146942564,5.61074319156655,8.89340137402969));
#28307=CARTESIAN_POINT('Ctrl Pts',(49.4902725446046,6.12760336939874,9.38216610144961));
#28308=CARTESIAN_POINT('Ctrl Pts',(51.5793981466453,6.64446354723092,9.87093082886955));
#28309=CARTESIAN_POINT('Ctrl Pts',(53.668523748686,7.16132372506311,9.38216610144961));
#28310=CARTESIAN_POINT('Ctrl Pts',(44.4687528548128,2.90816428999238,0.));
#28311=CARTESIAN_POINT('Ctrl Pts',(44.4382568180399,3.12026888468116,1.72780310113342));
#28312=CARTESIAN_POINT('Ctrl Pts',(45.149795935654,3.43906202795197,3.28449990511992));
#28313=CARTESIAN_POINT('Ctrl Pts',(45.8613350532681,3.7578551712228,4.84119670910639));
#28314=CARTESIAN_POINT('Ctrl Pts',(47.1679401624789,4.16220588757978,5.91846432228298));
#28315=CARTESIAN_POINT('Ctrl Pts',(48.4745452716896,4.56655660393679,6.99573193545957));
#28316=CARTESIAN_POINT('Ctrl Pts',(50.1113870920656,5.01838819123964,7.3802042952164));
#28317=CARTESIAN_POINT('Ctrl Pts',(51.7482289124415,5.47021977854247,7.76467665497322));
#28318=CARTESIAN_POINT('Ctrl Pts',(53.3850707328175,5.92205136584531,7.38020429521639));
#28319=CARTESIAN_POINT('',(37.5648924257523,4.19818497006209,1.57948606811744E-9));
#28320=CARTESIAN_POINT('Origin',(37.7741838134883,-13.8005982420128,0.));
#28321=CARTESIAN_POINT('Ctrl Pts',(37.5648924257933,4.19818497026059,3.13104703599162E-9));
#28322=CARTESIAN_POINT('Ctrl Pts',(37.562590034511,4.21419845373592,0.24503815333554));
#28323=CARTESIAN_POINT('Ctrl Pts',(37.5665407070749,4.23125516411427,0.490791160521858));
#28324=CARTESIAN_POINT('Ctrl Pts',(37.5768338592308,4.24933641208172,0.736766500725589));
#28325=CARTESIAN_POINT('Ctrl Pts',(37.5870932195462,4.26735830032753,0.981934317701222));
#28326=CARTESIAN_POINT('Ctrl Pts',(37.6036535888759,4.28639799775346,1.22732257376586));
#28327=CARTESIAN_POINT('Ctrl Pts',(37.6265535806588,4.3064283402013,1.47243294816361));
#28328=CARTESIAN_POINT('Ctrl Pts',(37.649419084278,4.32642851627456,1.71717417803036));
#28329=CARTESIAN_POINT('Ctrl Pts',(37.6786051816996,4.34741633416657,1.96163791541604));
#28330=CARTESIAN_POINT('Ctrl Pts',(37.7140992541436,4.369356356832,2.20532408778542));
#28331=CARTESIAN_POINT('Ctrl Pts',(37.7495628850543,4.39127756261105,2.44880126242083));
#28332=CARTESIAN_POINT('Ctrl Pts',(37.7913236642409,4.41414930860333,2.69150175431066));
#28333=CARTESIAN_POINT('Ctrl Pts',(37.8393176800295,4.43792826156017,2.93292951866823));
#28334=CARTESIAN_POINT('Ctrl Pts',(37.8873016553744,4.46170223991264,3.17430677585613));
#28335=CARTESIAN_POINT('Ctrl Pts',(37.9415161845175,4.48638300400794,3.41441139318375));
#28336=CARTESIAN_POINT('Ctrl Pts',(38.0018467100928,4.51191981196192,3.65275710614676));
#28337=CARTESIAN_POINT('Ctrl Pts',(38.0622538424058,4.53748904614668,3.89140546668832));
#28338=CARTESIAN_POINT('Ctrl Pts',(38.128792382057,4.5639164498048,4.12829002081211));
#28339=CARTESIAN_POINT('Ctrl Pts',(38.2012980447015,4.5911443167709,4.36293874377859));
#28340=CARTESIAN_POINT('Ctrl Pts',(38.2738776920355,4.61839996701916,4.59782690201494));
#28341=CARTESIAN_POINT('Ctrl Pts',(38.3524364483673,4.6464576564197,4.83047425894999));
#28342=CARTESIAN_POINT('Ctrl Pts',(38.4367626436468,4.675253537117,5.06042975959466));
#28343=CARTESIAN_POINT('Ctrl Pts',(38.5213353756664,4.70413360568181,5.29105755998335));
#28344=CARTESIAN_POINT('Ctrl Pts',(38.6117090746819,4.73375612398284,5.51897736305714));
#28345=CARTESIAN_POINT('Ctrl Pts',(38.7076263878304,4.76405160819197,5.74376259354354));
#28346=CARTESIAN_POINT('Ctrl Pts',(38.7687861188958,4.78336890979173,5.88709234072634));
#28347=CARTESIAN_POINT('Ctrl Pts',(38.8321988522325,4.80295972078415,6.029148253142));
#28348=CARTESIAN_POINT('Ctrl Pts',(38.8977893740739,4.8228051450119,6.16982677023485));
#28349=CARTESIAN_POINT('Ctrl Pts',(39.0006372418043,4.85392335399592,6.39041482339099));
#28350=CARTESIAN_POINT('Ctrl Pts',(39.1094140363897,4.88603794597511,6.60890054011821));
#28351=CARTESIAN_POINT('Ctrl Pts',(39.2239895821647,4.91909873852093,6.82480412008064));
#28352=CARTESIAN_POINT('Ctrl Pts',(39.3383064672143,4.95208489447194,7.04022028559313));
#28353=CARTESIAN_POINT('Ctrl Pts',(39.458395867156,4.98601294426688,7.25306552029656));
#28354=CARTESIAN_POINT('Ctrl Pts',(39.584078946338,5.02082444100455,7.46287566269435));
#28355=CARTESIAN_POINT('Ctrl Pts',(39.7095598756334,5.05557994659237,7.67234834441894));
#28356=CARTESIAN_POINT('Ctrl Pts',(39.8406163594389,5.091216009501,7.87879526533036));
#28357=CARTESIAN_POINT('Ctrl Pts',(39.9770226972832,5.12766654724745,8.08177334612198));
#28358=CARTESIAN_POINT('Ctrl Pts',(40.1132981483379,5.16408210939131,8.28455666214124));
#28359=CARTESIAN_POINT('Ctrl Pts',(40.2549129874365,5.20131052440296,8.48387739272877));
#28360=CARTESIAN_POINT('Ctrl Pts',(40.4015971043843,5.23927881325903,8.67931873611127));
#28361=CARTESIAN_POINT('Ctrl Pts',(40.5482882764499,5.27724892828933,8.87476947970516));
#28362=CARTESIAN_POINT('Ctrl Pts',(40.7000489573831,5.31595892053015,9.06634009532842));
#28363=CARTESIAN_POINT('Ctrl Pts',(40.8565673625296,5.35532966548965,9.25364450340988));
#28364=CARTESIAN_POINT('Ctrl Pts',(41.0131431849084,5.3947148532184,9.44101762226502));
#28365=CARTESIAN_POINT('Ctrl Pts',(41.1744799145451,5.43476120340312,9.62412107875041));
#28366=CARTESIAN_POINT('Ctrl Pts',(41.3402280007164,5.47538443899869,9.80260437466134));
#28367=CARTESIAN_POINT('Ctrl Pts',(41.5062464563474,5.51607393950573,9.98137881379686));
#28368=CARTESIAN_POINT('Ctrl Pts',(41.6766903238787,5.55734212879157,10.1555177270925));
#28369=CARTESIAN_POINT('Ctrl Pts',(41.8511757273808,5.59910040291772,10.3247095747708));
#28370=CARTESIAN_POINT('Ctrl Pts',(41.9016079152,5.61116995762813,10.3736117457739));
#28371=CARTESIAN_POINT('Ctrl Pts',(41.9523775462543,5.62328043365736,10.4221009095724));
#28372=CARTESIAN_POINT('Ctrl Pts',(42.0034749115207,5.63542964579433,10.4701702229062));
#28373=CARTESIAN_POINT('Ctrl Pts',(43.4867804707272,9.73793223897082,1.04083408558608E-14));
#28374=CARTESIAN_POINT('Ctrl Pts',(43.4562844339543,9.9500368336596,1.72780310113343));
#28375=CARTESIAN_POINT('Ctrl Pts',(44.1678235515684,10.2688299769304,3.28449990511991));
#28376=CARTESIAN_POINT('Ctrl Pts',(44.8793626691825,10.5876231202012,4.84119670910638));
#28377=CARTESIAN_POINT('Ctrl Pts',(46.1859677783933,10.9919738365582,5.91846432228298));
#28378=CARTESIAN_POINT('Ctrl Pts',(47.492572887604,11.3963245529152,6.99573193545956));
#28379=CARTESIAN_POINT('Ctrl Pts',(49.12941470798,11.8481561402181,7.3802042952164));
#28380=CARTESIAN_POINT('Ctrl Pts',(50.7662565283559,12.2999877275209,7.76467665497321));
#28381=CARTESIAN_POINT('Ctrl Pts',(52.4030983487318,12.7518193148238,7.3802042952164));
#28382=CARTESIAN_POINT('Ctrl Pts',(41.6230663715378,8.27145263712653,0.));
#28383=CARTESIAN_POINT('Ctrl Pts',(41.5925703347649,8.48355723181529,2.19648874705823));
#28384=CARTESIAN_POINT('Ctrl Pts',(42.5053946713977,8.83129082048301,4.17545672685568));
#28385=CARTESIAN_POINT('Ctrl Pts',(43.4182190080304,9.17902440915073,6.15442470665315));
#28386=CARTESIAN_POINT('Ctrl Pts',(45.0875275490506,9.63552400615941,7.52391304034141));
#28387=CARTESIAN_POINT('Ctrl Pts',(46.7568360900709,10.0920236031681,8.89340137402968));
#28388=CARTESIAN_POINT('Ctrl Pts',(48.8459616921115,10.6088837810003,9.38216610144961));
#28389=CARTESIAN_POINT('Ctrl Pts',(50.9350872941522,11.1257439588325,9.87093082886954));
#28390=CARTESIAN_POINT('Ctrl Pts',(53.0242128961929,11.6426041366647,9.38216610144961));
#28391=CARTESIAN_POINT('Ctrl Pts',(39.5090640497074,7.19674949232866,0.));
#28392=CARTESIAN_POINT('Ctrl Pts',(39.4785680129346,7.40885408701741,2.70899372698069));
#28393=CARTESIAN_POINT('Ctrl Pts',(40.6114965452661,7.78823388144385,5.14971273833323));
#28394=CARTESIAN_POINT('Ctrl Pts',(41.7444250775976,8.16761367587025,7.59043174968578));
#28395=CARTESIAN_POINT('Ctrl Pts',(43.8103476746564,8.6811377652306,9.27946171175751));
#28396=CARTESIAN_POINT('Ctrl Pts',(45.8762702717153,9.19466185459093,10.9684916738292));
#28397=CARTESIAN_POINT('Ctrl Pts',(48.4599655121837,9.78263041129798,11.5712994880388));
#28398=CARTESIAN_POINT('Ctrl Pts',(51.0436607526522,10.370598968005,12.1741073022483));
#28399=CARTESIAN_POINT('Ctrl Pts',(53.6273559931206,10.9585675247121,11.5712994880388));
#28400=CARTESIAN_POINT('Ctrl Pts',(37.2260157227863,6.55512420987368,0.));
#28401=CARTESIAN_POINT('Ctrl Pts',(37.1955196860134,6.76722880456246,3.24562220582792));
#28402=CARTESIAN_POINT('Ctrl Pts',(38.5589126710877,7.17974438483072,6.16982677025168));
#28403=CARTESIAN_POINT('Ctrl Pts',(39.9223056561619,7.59225996509896,9.0940313346754));
#28404=CARTESIAN_POINT('Ctrl Pts',(42.4035108473794,8.16549267737322,11.1176436806954));
#28405=CARTESIAN_POINT('Ctrl Pts',(44.8847160385968,8.7387253896475,13.1412560267153));
#28406=CARTESIAN_POINT('Ctrl Pts',(47.9862602037601,9.40114938129427,13.8634749112255));
#28407=CARTESIAN_POINT('Ctrl Pts',(51.0878043689233,10.0635733729411,14.5856937957357));
#28408=CARTESIAN_POINT('Ctrl Pts',(54.1893485340865,10.7259973645878,13.8634749112255));
#28409=CARTESIAN_POINT('',(37.2260157227863,6.55512420987368,0.));
#28410=CARTESIAN_POINT('Ctrl Pts',(37.2260157227863,6.55512420987368,0.));
#28411=CARTESIAN_POINT('Ctrl Pts',(37.1955196860134,6.76722880456246,3.24562220582792));
#28412=CARTESIAN_POINT('Ctrl Pts',(38.5589126710877,7.17974438483072,6.16982677025168));
#28413=CARTESIAN_POINT('Ctrl Pts',(39.6971249853933,7.52412807936664,8.61106394926976));
#28414=CARTESIAN_POINT('Ctrl Pts',(41.6420486840549,7.98700482807798,10.4489096280657));
#28415=CARTESIAN_POINT('Origin',(32.3559861244014,23.8837944332594,0.));
#28416=CARTESIAN_POINT('Ctrl Pts',(37.2260157227863,6.55512420987368,0.));
#28417=CARTESIAN_POINT('Ctrl Pts',(37.1955196860134,6.76722880456246,3.24562220582792));
#28418=CARTESIAN_POINT('Ctrl Pts',(38.5589126710877,7.17974438483072,6.16982677025168));
#28419=CARTESIAN_POINT('Ctrl Pts',(39.9223056561619,7.59225996509896,9.0940313346754));
#28420=CARTESIAN_POINT('Ctrl Pts',(42.4035108473794,8.16549267737322,11.1176436806954));
#28421=CARTESIAN_POINT('Ctrl Pts',(44.8847160385968,8.7387253896475,13.1412560267153));
#28422=CARTESIAN_POINT('Ctrl Pts',(47.9862602037601,9.40114938129427,13.8634749112255));
#28423=CARTESIAN_POINT('Ctrl Pts',(51.0878043689233,10.0635733729411,14.5856937957357));
#28424=CARTESIAN_POINT('Ctrl Pts',(54.1893485340865,10.7259973645878,13.8634749112255));
#28425=CARTESIAN_POINT('Ctrl Pts',(36.7040912252866,5.75838408981591,0.));
#28426=CARTESIAN_POINT('Ctrl Pts',(36.6735951885137,5.97048868450468,3.38941559469373));
#28427=CARTESIAN_POINT('Ctrl Pts',(38.0987427505052,6.39188323248848,6.44317352589574));
#28428=CARTESIAN_POINT('Ctrl Pts',(39.5238903124967,6.81327778047227,9.49693145709775));
#28429=CARTESIAN_POINT('Ctrl Pts',(42.1163734062201,7.40250983972819,11.6101975146502));
#28430=CARTESIAN_POINT('Ctrl Pts',(44.7088564999435,7.99174189898409,13.7234635722027));
#28431=CARTESIAN_POINT('Ctrl Pts',(47.949161939876,8.67411674998977,14.4776794959001));
#28432=CARTESIAN_POINT('Ctrl Pts',(51.1894673798085,9.35649160099544,15.2318954195974));
#28433=CARTESIAN_POINT('Ctrl Pts',(54.4297728197411,10.0388664520011,14.4776794959001));
#28434=CARTESIAN_POINT('Ctrl Pts',(36.8396419064669,4.81560839388842,6.24500451351652E-15));
#28435=CARTESIAN_POINT('Ctrl Pts',(36.8091458696941,5.0277129885772,3.38941559469373));
#28436=CARTESIAN_POINT('Ctrl Pts',(38.2342934316856,5.44910753656099,6.44317352589574));
#28437=CARTESIAN_POINT('Ctrl Pts',(39.6594409936771,5.87050208454479,9.49693145709774));
#28438=CARTESIAN_POINT('Ctrl Pts',(42.2519240874005,6.45973414380071,11.6101975146502));
#28439=CARTESIAN_POINT('Ctrl Pts',(44.8444071811239,7.04896620305661,13.7234635722027));
#28440=CARTESIAN_POINT('Ctrl Pts',(48.0847126210564,7.73134105406228,14.4776794959001));
#28441=CARTESIAN_POINT('Ctrl Pts',(51.3250180609889,8.41371590506795,15.2318954195974));
#28442=CARTESIAN_POINT('Ctrl Pts',(54.5653235009214,9.09609075607363,14.4776794959001));
#28443=CARTESIAN_POINT('Ctrl Pts',(37.5648924257372,4.19818497005498,0.));
#28444=CARTESIAN_POINT('Ctrl Pts',(37.5343963889644,4.41028956474376,3.24562220582792));
#28445=CARTESIAN_POINT('Ctrl Pts',(38.8977893740386,4.822805145012,6.16982677025168));
#28446=CARTESIAN_POINT('Ctrl Pts',(40.2611823591128,5.23532072528026,9.09403133467541));
#28447=CARTESIAN_POINT('Ctrl Pts',(42.7423875503303,5.80855343755452,11.1176436806954));
#28448=CARTESIAN_POINT('Ctrl Pts',(45.2235927415478,6.38178614982881,13.1412560267153));
#28449=CARTESIAN_POINT('Ctrl Pts',(48.325136906711,7.04421014147557,13.8634749112255));
#28450=CARTESIAN_POINT('Ctrl Pts',(51.4266810718742,7.70663413312235,14.5856937957357));
#28451=CARTESIAN_POINT('Ctrl Pts',(54.5282252370374,8.36905812476912,13.8634749112255));
#28452=CARTESIAN_POINT('',(36.9500351333054,5.31260798930611,1.06286264225831E-29));
#28453=CARTESIAN_POINT('Origin',(38.731713020801,5.56877962163325,0.));
#28454=CARTESIAN_POINT('Origin',(38.731713020801,5.56877962163325,0.));
#28455=CARTESIAN_POINT('Ctrl Pts',(37.78,-1.19058808997946,0.));
#28456=CARTESIAN_POINT('Ctrl Pts',(37.78,-0.976302375693734,3.24562220582793));
#28457=CARTESIAN_POINT('Ctrl Pts',(39.1882226984276,-0.762016661408056,
6.16982677025167));
#28458=CARTESIAN_POINT('Ctrl Pts',(40.5964453968552,-0.547730947122339,
9.09403133467541));
#28459=CARTESIAN_POINT('Ctrl Pts',(43.1339750175689,-0.33344523283667,11.1176436806954));
#28460=CARTESIAN_POINT('Ctrl Pts',(45.6715046382825,-0.119159518550966,
13.1412560267153));
#28461=CARTESIAN_POINT('Ctrl Pts',(48.8357523191413,0.0951261957347176,
13.8634749112255));
#28462=CARTESIAN_POINT('Ctrl Pts',(52.0000000000001,0.309411910020398,14.5856937957357));
#28463=CARTESIAN_POINT('Ctrl Pts',(55.1642476808588,0.523697624306074,13.8634749112255));
#28464=CARTESIAN_POINT('Ctrl Pts',(40.1311229851415,-1.50077089879047,0.));
#28465=CARTESIAN_POINT('Ctrl Pts',(40.1311229851416,-1.28648518450476,2.70899372698069));
#28466=CARTESIAN_POINT('Ctrl Pts',(41.30651131265,-1.07219947021906,5.14971273833323));
#28467=CARTESIAN_POINT('Ctrl Pts',(42.4818996401583,-0.857913755933361,
7.59043174968578));
#28468=CARTESIAN_POINT('Ctrl Pts',(44.5998762217203,-0.643628041647661,
9.27946171175752));
#28469=CARTESIAN_POINT('Ctrl Pts',(46.7178528032822,-0.429342327361976,
10.9684916738293));
#28470=CARTESIAN_POINT('Ctrl Pts',(49.3589264016411,-0.21505661307629,11.5712994880388));
#28471=CARTESIAN_POINT('Ctrl Pts',(52.0000000000001,-0.000770898790611535,
12.1741073022483));
#28472=CARTESIAN_POINT('Ctrl Pts',(54.641073598359,0.213514815495078,11.5712994880388));
#28473=CARTESIAN_POINT('Ctrl Pts',(42.376554015719,-2.2636812166277,0.));
#28474=CARTESIAN_POINT('Ctrl Pts',(42.3765540157191,-2.04939550234198,2.19648874705824));
#28475=CARTESIAN_POINT('Ctrl Pts',(43.3295747662223,-1.83510978805626,4.17545672685568));
#28476=CARTESIAN_POINT('Ctrl Pts',(44.2825955167256,-1.62082407377057,6.15442470665314));
#28477=CARTESIAN_POINT('Ctrl Pts',(45.9998795700625,-1.40653835948487,7.5239130403414));
#28478=CARTESIAN_POINT('Ctrl Pts',(47.7171636233994,-1.19225264519917,8.89340137402968));
#28479=CARTESIAN_POINT('Ctrl Pts',(49.8585818116997,-0.977966930913482,
9.38216610144961));
#28480=CARTESIAN_POINT('Ctrl Pts',(52.0000000000001,-0.763681216627804,
9.87093082886955));
#28481=CARTESIAN_POINT('Ctrl Pts',(54.1414181883005,-0.549395502342091,
9.38216610144961));
#28482=CARTESIAN_POINT('Ctrl Pts',(44.43,-3.45000000000046,0.));
#28483=CARTESIAN_POINT('Ctrl Pts',(44.43,-3.23571428571475,1.72780310113343));
#28484=CARTESIAN_POINT('Ctrl Pts',(45.1796656699787,-3.02142857142903,3.28449990511992));
#28485=CARTESIAN_POINT('Ctrl Pts',(45.9293313399574,-2.80714285714333,4.84119670910639));
#28486=CARTESIAN_POINT('Ctrl Pts',(47.2801821999294,-2.59285714285764,5.91846432228298));
#28487=CARTESIAN_POINT('Ctrl Pts',(48.6310330599014,-2.37857142857193,6.99573193545956));
#28488=CARTESIAN_POINT('Ctrl Pts',(50.3155165299507,-2.16428571428624,7.38020429521639));
#28489=CARTESIAN_POINT('Ctrl Pts',(52.,-1.95000000000054,7.76467665497322));
#28490=CARTESIAN_POINT('Ctrl Pts',(53.6844834700493,-1.73571428571485,7.38020429521639));
#28491=CARTESIAN_POINT('',(37.7799999998362,-1.19058808962906,-2.44188901215463E-9));
#28492=CARTESIAN_POINT('Origin',(35.4256671812558,-19.0359549110505,1.04083408558608E-14));
#28493=CARTESIAN_POINT('Ctrl Pts',(37.78,-1.19058808997946,0.));
#28494=CARTESIAN_POINT('Ctrl Pts',(37.78,-0.976302375693734,3.24562220582793));
#28495=CARTESIAN_POINT('Ctrl Pts',(39.1882226984276,-0.762016661408056,
6.16982677025167));
#28496=CARTESIAN_POINT('Ctrl Pts',(40.3709173991841,-0.582048976597612,
8.62571762198518));
#28497=CARTESIAN_POINT('Ctrl Pts',(42.3779453595727,-0.399648641330362,
10.4701702229062));
#28498=CARTESIAN_POINT('Ctrl Pts',(44.4300000000001,3.44999999999955,0.));
#28499=CARTESIAN_POINT('Ctrl Pts',(44.43,3.66428571428526,1.72780310113343));
#28500=CARTESIAN_POINT('Ctrl Pts',(45.1796656699788,3.87857142857096,3.28449990511991));
#28501=CARTESIAN_POINT('Ctrl Pts',(45.9293313399575,4.09285714285668,4.84119670910639));
#28502=CARTESIAN_POINT('Ctrl Pts',(47.2801821999295,4.30714285714236,5.91846432228298));
#28503=CARTESIAN_POINT('Ctrl Pts',(48.6310330599015,4.52142857142807,6.99573193545957));
#28504=CARTESIAN_POINT('Ctrl Pts',(50.3155165299508,4.73571428571376,7.38020429521639));
#28505=CARTESIAN_POINT('Ctrl Pts',(52.0000000000001,4.94999999999945,7.76467665497322));
#28506=CARTESIAN_POINT('Ctrl Pts',(53.6844834700494,5.16428571428516,7.38020429521639));
#28507=CARTESIAN_POINT('Ctrl Pts',(42.3765540157191,2.26368121662681,0.));
#28508=CARTESIAN_POINT('Ctrl Pts',(42.3765540157191,2.47796693091252,2.19648874705823));
#28509=CARTESIAN_POINT('Ctrl Pts',(43.3295747662223,2.69225264519823,4.17545672685568));
#28510=CARTESIAN_POINT('Ctrl Pts',(44.2825955167256,2.90653835948393,6.15442470665313));
#28511=CARTESIAN_POINT('Ctrl Pts',(45.9998795700625,3.12082407376963,7.5239130403414));
#28512=CARTESIAN_POINT('Ctrl Pts',(47.7171636233994,3.33510978805533,8.89340137402968));
#28513=CARTESIAN_POINT('Ctrl Pts',(49.8585818116998,3.54939550234102,9.3821661014496));
#28514=CARTESIAN_POINT('Ctrl Pts',(52.0000000000001,3.7636812166267,9.87093082886954));
#28515=CARTESIAN_POINT('Ctrl Pts',(54.1414181883005,3.97796693091241,9.3821661014496));
#28516=CARTESIAN_POINT('Ctrl Pts',(40.1311229851416,1.50077089878964,-1.05434036998093E-14));
#28517=CARTESIAN_POINT('Ctrl Pts',(40.1311229851416,1.71505661307536,2.70899372698069));
#28518=CARTESIAN_POINT('Ctrl Pts',(41.30651131265,1.92934232736107,5.14971273833323));
#28519=CARTESIAN_POINT('Ctrl Pts',(42.4818996401584,2.14362804164676,7.59043174968578));
#28520=CARTESIAN_POINT('Ctrl Pts',(44.5998762217203,2.35791375593245,9.2794617117575));
#28521=CARTESIAN_POINT('Ctrl Pts',(46.7178528032822,2.57219947021815,10.9684916738292));
#28522=CARTESIAN_POINT('Ctrl Pts',(49.3589264016411,2.78648518450383,11.5712994880388));
#28523=CARTESIAN_POINT('Ctrl Pts',(52.0000000000001,3.00077089878951,12.1741073022483));
#28524=CARTESIAN_POINT('Ctrl Pts',(54.641073598359,3.2150566130752,11.5712994880388));
#28525=CARTESIAN_POINT('Ctrl Pts',(37.78,1.19058808997868,0.));
#28526=CARTESIAN_POINT('Ctrl Pts',(37.7800000000001,1.4048738042644,3.24562220582793));
#28527=CARTESIAN_POINT('Ctrl Pts',(39.1882226984277,1.6191595185501,6.16982677025167));
#28528=CARTESIAN_POINT('Ctrl Pts',(40.5964453968553,1.8334452328358,9.09403133467541));
#28529=CARTESIAN_POINT('Ctrl Pts',(43.1339750175689,2.04773094712147,11.1176436806954));
#28530=CARTESIAN_POINT('Ctrl Pts',(45.6715046382825,2.26201666140717,13.1412560267153));
#28531=CARTESIAN_POINT('Ctrl Pts',(48.8357523191413,2.47630237569286,13.8634749112255));
#28532=CARTESIAN_POINT('Ctrl Pts',(52.0000000000001,2.69058808997853,14.5856937957357));
#28533=CARTESIAN_POINT('Ctrl Pts',(55.1642476808589,2.90487380426421,13.8634749112255));
#28534=CARTESIAN_POINT('',(37.78,1.19058808997869,0.));
#28535=CARTESIAN_POINT('Ctrl Pts',(37.78,1.19058808997869,0.));
#28536=CARTESIAN_POINT('Ctrl Pts',(37.7800000000001,1.4048738042644,3.24562220582793));
#28537=CARTESIAN_POINT('Ctrl Pts',(39.1882226984277,1.6191595185501,6.16982677025167));
#28538=CARTESIAN_POINT('Ctrl Pts',(40.3638605623321,1.79805338220488,8.61106394926975));
#28539=CARTESIAN_POINT('Ctrl Pts',(42.3548619717231,1.97942721139859,10.4489096280657));
#28540=CARTESIAN_POINT('Origin',(35.4256671812562,19.0359549110498,0.));
#28541=CARTESIAN_POINT('Ctrl Pts',(37.78,1.19058808997868,0.));
#28542=CARTESIAN_POINT('Ctrl Pts',(37.7800000000001,1.4048738042644,3.24562220582793));
#28543=CARTESIAN_POINT('Ctrl Pts',(39.1882226984277,1.6191595185501,6.16982677025167));
#28544=CARTESIAN_POINT('Ctrl Pts',(40.5964453968553,1.8334452328358,9.09403133467541));
#28545=CARTESIAN_POINT('Ctrl Pts',(43.1339750175689,2.04773094712147,11.1176436806954));
#28546=CARTESIAN_POINT('Ctrl Pts',(45.6715046382825,2.26201666140717,13.1412560267153));
#28547=CARTESIAN_POINT('Ctrl Pts',(48.8357523191413,2.47630237569286,13.8634749112255));
#28548=CARTESIAN_POINT('Ctrl Pts',(52.0000000000001,2.69058808997853,14.5856937957357));
#28549=CARTESIAN_POINT('Ctrl Pts',(55.1642476808589,2.90487380426421,13.8634749112255));
#28550=CARTESIAN_POINT('Ctrl Pts',(37.15,0.476235235991243,0.));
#28551=CARTESIAN_POINT('Ctrl Pts',(37.1500000000001,0.69052095027696,3.38941559469373));
#28552=CARTESIAN_POINT('Ctrl Pts',(38.6206123116491,0.904806664562659,6.44317352589573));
#28553=CARTESIAN_POINT('Ctrl Pts',(40.0912246232982,1.11909237884837,9.49693145709774));
#28554=CARTESIAN_POINT('Ctrl Pts',(42.7411764423978,1.33337809313404,11.6101975146502));
#28555=CARTESIAN_POINT('Ctrl Pts',(45.3911282614975,1.54766380741972,13.7234635722027));
#28556=CARTESIAN_POINT('Ctrl Pts',(48.6955641307488,1.76194952170541,14.4776794959001));
#28557=CARTESIAN_POINT('Ctrl Pts',(52.,1.97623523599108,15.2318954195974));
#28558=CARTESIAN_POINT('Ctrl Pts',(55.3044358692513,2.19052095027676,14.4776794959001));
#28559=CARTESIAN_POINT('Ctrl Pts',(37.15,-0.476235235992009,0.));
#28560=CARTESIAN_POINT('Ctrl Pts',(37.15,-0.261949521706298,3.38941559469373));
#28561=CARTESIAN_POINT('Ctrl Pts',(38.6206123116491,-0.0476638074206039,
6.44317352589573));
#28562=CARTESIAN_POINT('Ctrl Pts',(40.0912246232982,0.166621906865105,9.49693145709774));
#28563=CARTESIAN_POINT('Ctrl Pts',(42.7411764423978,0.380907621150789,11.6101975146502));
#28564=CARTESIAN_POINT('Ctrl Pts',(45.3911282614975,0.595193335436467,13.7234635722027));
#28565=CARTESIAN_POINT('Ctrl Pts',(48.6955641307488,0.80947904972215,14.4776794959001));
#28566=CARTESIAN_POINT('Ctrl Pts',(52.,1.02376476400783,15.2318954195974));
#28567=CARTESIAN_POINT('Ctrl Pts',(55.3044358692513,1.23805047829351,14.4776794959001));
#28568=CARTESIAN_POINT('Ctrl Pts',(37.7800000000001,-1.19058808997946,0.));
#28569=CARTESIAN_POINT('Ctrl Pts',(37.7800000000001,-0.976302375693737,
3.24562220582793));
#28570=CARTESIAN_POINT('Ctrl Pts',(39.1882226984276,-0.762016661408056,
6.16982677025167));
#28571=CARTESIAN_POINT('Ctrl Pts',(40.5964453968553,-0.547730947122335,
9.09403133467541));
#28572=CARTESIAN_POINT('Ctrl Pts',(43.1339750175689,-0.333445232836653,
11.1176436806954));
#28573=CARTESIAN_POINT('Ctrl Pts',(45.6715046382825,-0.11915951855097,13.1412560267153));
#28574=CARTESIAN_POINT('Ctrl Pts',(48.8357523191413,0.095126195734721,13.8634749112255));
#28575=CARTESIAN_POINT('Ctrl Pts',(52.0000000000001,0.309411910020398,14.5856937957357));
#28576=CARTESIAN_POINT('Ctrl Pts',(55.1642476808589,0.523697624306077,13.8634749112255));
#28577=CARTESIAN_POINT('',(37.3300000000069,-4.97400852990502E-6,1.27795074265261E-29));
#28578=CARTESIAN_POINT('Origin',(39.13,-4.02455846426619E-13,0.));
#28579=CARTESIAN_POINT('Origin',(39.13,-4.02455846426619E-13,0.));
#28580=CARTESIAN_POINT('Ctrl Pts',(37.2260157227862,-6.55512420987448,0.));
#28581=CARTESIAN_POINT('Ctrl Pts',(37.256511759559,-6.34301961518571,3.24562220582792));
#28582=CARTESIAN_POINT('Ctrl Pts',(38.6808968181789,-6.33132600607645,6.16982677025168));
#28583=CARTESIAN_POINT('Ctrl Pts',(40.1052818767988,-6.31963239696717,9.09403133467541));
#28584=CARTESIAN_POINT('Ctrl Pts',(42.647479141562,-6.46865591986398,11.1176436806954));
#28585=CARTESIAN_POINT('Ctrl Pts',(45.1896764063252,-6.61767944276075,13.1412560267153));
#28586=CARTESIAN_POINT('Ctrl Pts',(48.3522126450341,-6.85589424503005,13.8634749112255));
#28587=CARTESIAN_POINT('Ctrl Pts',(51.5147488837429,-7.09410904729936,14.5856937957357));
#28588=CARTESIAN_POINT('Ctrl Pts',(54.6772851224518,-7.33232384956867,13.8634749112255));
#28589=CARTESIAN_POINT('Ctrl Pts',(39.5090640497072,-7.1967494923295,-1.05434036998093E-14));
#28590=CARTESIAN_POINT('Ctrl Pts',(39.5395600864801,-6.98464489764072,2.70899372698069));
#28591=CARTESIAN_POINT('Ctrl Pts',(40.7334806923573,-6.93981550268964,5.14971273833323));
#28592=CARTESIAN_POINT('Ctrl Pts',(41.9274012982345,-6.89498610773854,7.59043174968577));
#28593=CARTESIAN_POINT('Ctrl Pts',(44.054315968839,-6.98430100772137,9.27946171175751));
#28594=CARTESIAN_POINT('Ctrl Pts',(46.1812306394436,-7.07361590770423,10.9684916738293));
#28595=CARTESIAN_POINT('Ctrl Pts',(48.8259179534577,-7.23737527503378,11.5712994880388));
#28596=CARTESIAN_POINT('Ctrl Pts',(51.4706052674719,-7.40113464236333,12.1741073022483));
#28597=CARTESIAN_POINT('Ctrl Pts',(54.115292581486,-7.56489400969289,11.5712994880388));
#28598=CARTESIAN_POINT('Ctrl Pts',(41.6230663715376,-8.27145263712742,0.));
#28599=CARTESIAN_POINT('Ctrl Pts',(41.6535624083104,-8.05934804243867,2.19648874705824));
#28600=CARTESIAN_POINT('Ctrl Pts',(42.6273788184889,-7.98287244172884,4.17545672685568));
#28601=CARTESIAN_POINT('Ctrl Pts',(43.6011952286674,-7.90639684101905,6.15442470665314));
#28602=CARTESIAN_POINT('Ctrl Pts',(45.3314958432332,-7.93868724865023,7.5239130403414));
#28603=CARTESIAN_POINT('Ctrl Pts',(47.0617964577991,-7.97097765628139,8.89340137402967));
#28604=CARTESIAN_POINT('Ctrl Pts',(49.2119141333854,-8.06362864473609,9.38216610144961));
#28605=CARTESIAN_POINT('Ctrl Pts',(51.3620318089718,-8.15627963319078,9.87093082886954));
#28606=CARTESIAN_POINT('Ctrl Pts',(53.5121494845582,-8.24893062164547,9.3821661014496));
#28607=CARTESIAN_POINT('Ctrl Pts',(43.4867804707269,-9.73793223897177,0.));
#28608=CARTESIAN_POINT('Ctrl Pts',(43.5172765074998,-9.525827644283,1.72780310113342));
#28609=CARTESIAN_POINT('Ctrl Pts',(44.2898076986596,-9.42041159817628,3.28449990511991));
#28610=CARTESIAN_POINT('Ctrl Pts',(45.0623388898194,-9.31499555206956,4.84119670910639));
#28611=CARTESIAN_POINT('Ctrl Pts',(46.4299360725758,-9.29513707904906,5.91846432228298));
#28612=CARTESIAN_POINT('Ctrl Pts',(47.7975332553323,-9.27527860602855,6.99573193545956));
#28613=CARTESIAN_POINT('Ctrl Pts',(49.4953671492539,-9.30290100395389,7.38020429521639));
#28614=CARTESIAN_POINT('Ctrl Pts',(51.1932010431756,-9.33052340187922,7.76467665497322));
#28615=CARTESIAN_POINT('Ctrl Pts',(52.8910349370971,-9.35814579980457,7.38020429521639));
#28616=CARTESIAN_POINT('',(37.226015722685,-6.55512420967655,-1.21941697785192E-9));
#28617=CARTESIAN_POINT('Origin',(32.3559861244009,-23.8837944332601,0.));
#28618=CARTESIAN_POINT('Ctrl Pts',(37.2260157227862,-6.55512420987448,0.));
#28619=CARTESIAN_POINT('Ctrl Pts',(37.256511759559,-6.34301961518571,3.24562220582792));
#28620=CARTESIAN_POINT('Ctrl Pts',(38.6808968181789,-6.33132600607645,6.16982677025168));
#28621=CARTESIAN_POINT('Ctrl Pts',(39.8771654641448,-6.32150513787023,8.62571762198518));
#28622=CARTESIAN_POINT('Ctrl Pts',(41.8897230480066,-6.42659123460911,10.4701702229062));
#28623=CARTESIAN_POINT('Ctrl Pts',(44.4687528548127,-2.90816428999336,0.));
#28624=CARTESIAN_POINT('Ctrl Pts',(44.4992488915855,-2.69605969530457,1.72780310113343));
#28625=CARTESIAN_POINT('Ctrl Pts',(45.2717800827454,-2.59064364919786,3.28449990511992));
#28626=CARTESIAN_POINT('Ctrl Pts',(46.0443112739052,-2.48522760309115,4.84119670910639));
#28627=CARTESIAN_POINT('Ctrl Pts',(47.4119084566616,-2.46536913007065,5.91846432228298));
#28628=CARTESIAN_POINT('Ctrl Pts',(48.779505639418,-2.44551065705014,6.99573193545957));
#28629=CARTESIAN_POINT('Ctrl Pts',(50.4773395333396,-2.47313305497548,7.3802042952164));
#28630=CARTESIAN_POINT('Ctrl Pts',(52.1751734272613,-2.50075545290081,7.76467665497322));
#28631=CARTESIAN_POINT('Ctrl Pts',(53.8730073211829,-2.52837785082615,7.3802042952164));
#28632=CARTESIAN_POINT('Ctrl Pts',(42.2673772240308,-3.7901722255259,0.));
#28633=CARTESIAN_POINT('Ctrl Pts',(42.2978732608037,-3.57806763083714,2.19648874705823));
#28634=CARTESIAN_POINT('Ctrl Pts',(43.2716896709821,-3.50159203012731,4.17545672685568));
#28635=CARTESIAN_POINT('Ctrl Pts',(44.2455060811606,-3.42511642941753,6.15442470665314));
#28636=CARTESIAN_POINT('Ctrl Pts',(45.9758066957264,-3.4574068370487,7.5239130403414));
#28637=CARTESIAN_POINT('Ctrl Pts',(47.7061073102923,-3.48969724467988,8.89340137402967));
#28638=CARTESIAN_POINT('Ctrl Pts',(49.8562249858787,-3.58234823313457,9.3821661014496));
#28639=CARTESIAN_POINT('Ctrl Pts',(52.006342661465,-3.67499922158926,9.87093082886954));
#28640=CARTESIAN_POINT('Ctrl Pts',(54.1564603370514,-3.76765021004393,9.38216610144961));
#28641=CARTESIAN_POINT('Ctrl Pts',(39.9362279852004,-4.22575906238287,-1.05434036998093E-14));
#28642=CARTESIAN_POINT('Ctrl Pts',(39.9667240219732,-4.01365446769409,2.70899372698069));
#28643=CARTESIAN_POINT('Ctrl Pts',(41.1606446278505,-3.968825072743,5.14971273833323));
#28644=CARTESIAN_POINT('Ctrl Pts',(42.3545652337277,-3.92399567779192,7.59043174968577));
#28645=CARTESIAN_POINT('Ctrl Pts',(44.4814799043322,-4.01331057777475,9.27946171175751));
#28646=CARTESIAN_POINT('Ctrl Pts',(46.6083945749367,-4.1026254777576,10.9684916738292));
#28647=CARTESIAN_POINT('Ctrl Pts',(49.2530818889508,-4.26638484508716,11.5712994880388));
#28648=CARTESIAN_POINT('Ctrl Pts',(51.897769202965,-4.43014421241671,12.1741073022483));
#28649=CARTESIAN_POINT('Ctrl Pts',(54.5424565169792,-4.59390357974626,11.5712994880388));
#28650=CARTESIAN_POINT('Ctrl Pts',(37.5648924257371,-4.19818497005578,0.));
#28651=CARTESIAN_POINT('Ctrl Pts',(37.59538846251,-3.98608037536701,3.24562220582793));
#28652=CARTESIAN_POINT('Ctrl Pts',(39.0197735211298,-3.97438676625777,6.16982677025168));
#28653=CARTESIAN_POINT('Ctrl Pts',(40.4441585797498,-3.96269315714849,9.09403133467541));
#28654=CARTESIAN_POINT('Ctrl Pts',(42.986355844513,-4.11171668004528,11.1176436806954));
#28655=CARTESIAN_POINT('Ctrl Pts',(45.5285531092761,-4.26074020294207,13.1412560267153));
#28656=CARTESIAN_POINT('Ctrl Pts',(48.691089347985,-4.49895500521137,13.8634749112255));
#28657=CARTESIAN_POINT('Ctrl Pts',(51.8536255866939,-4.73716980748066,14.5856937957357));
#28658=CARTESIAN_POINT('Ctrl Pts',(55.0161618254028,-4.97538460974997,13.8634749112255));
#28659=CARTESIAN_POINT('',(37.5648924257371,-4.19818497005578,0.));
#28660=CARTESIAN_POINT('Ctrl Pts',(37.5648924257371,-4.19818497005578,0.));
#28661=CARTESIAN_POINT('Ctrl Pts',(37.59538846251,-3.98608037536701,3.24562220582793));
#28662=CARTESIAN_POINT('Ctrl Pts',(39.0197735211299,-3.97438676625775,6.16982677025168));
#28663=CARTESIAN_POINT('Ctrl Pts',(40.2089043379837,-3.96462449666083,8.61106394926976));
#28664=CARTESIAN_POINT('Ctrl Pts',(42.2054524109828,-4.06844583510822,10.4489096280657));
#28665=CARTESIAN_POINT('Origin',(37.7741838134886,13.800598242012,0.));
#28666=CARTESIAN_POINT('Ctrl Pts',(37.5648924257371,-4.19818497005578,0.));
#28667=CARTESIAN_POINT('Ctrl Pts',(37.59538846251,-3.98608037536701,3.24562220582793));
#28668=CARTESIAN_POINT('Ctrl Pts',(39.0197735211298,-3.97438676625777,6.16982677025168));
#28669=CARTESIAN_POINT('Ctrl Pts',(40.4441585797498,-3.96269315714849,9.09403133467541));
#28670=CARTESIAN_POINT('Ctrl Pts',(42.986355844513,-4.11171668004528,11.1176436806954));
#28671=CARTESIAN_POINT('Ctrl Pts',(45.5285531092761,-4.26074020294207,13.1412560267153));
#28672=CARTESIAN_POINT('Ctrl Pts',(48.691089347985,-4.49895500521137,13.8634749112255));
#28673=CARTESIAN_POINT('Ctrl Pts',(51.8536255866939,-4.73716980748066,14.5856937957357));
#28674=CARTESIAN_POINT('Ctrl Pts',(55.0161618254028,-4.97538460974997,13.8634749112255));
#28675=CARTESIAN_POINT('Ctrl Pts',(36.8396419064668,-4.81560839388922,6.24500451351651E-15));
#28676=CARTESIAN_POINT('Ctrl Pts',(36.8701379432397,-4.60350379920046,3.38941559469372));
#28677=CARTESIAN_POINT('Ctrl Pts',(38.3562775787769,-4.60068915780673,6.44317352589573));
#28678=CARTESIAN_POINT('Ctrl Pts',(39.8424172143141,-4.59787451641302,9.49693145709773));
#28679=CARTESIAN_POINT('Ctrl Pts',(42.4958923815831,-4.76289738629144,11.6101975146502));
#28680=CARTESIAN_POINT('Ctrl Pts',(45.1493675488522,-4.92792025616987,13.7234635722027));
#28681=CARTESIAN_POINT('Ctrl Pts',(48.4506650623304,-5.18608591779808,14.4776794959001));
#28682=CARTESIAN_POINT('Ctrl Pts',(51.7519625758086,-5.44425157942627,15.2318954195974));
#28683=CARTESIAN_POINT('Ctrl Pts',(55.0532600892868,-5.70241724105448,14.4776794959001));
#28684=CARTESIAN_POINT('Ctrl Pts',(36.7040912252864,-5.7583840898167,0.));
#28685=CARTESIAN_POINT('Ctrl Pts',(36.7345872620593,-5.54627949512793,3.38941559469372));
#28686=CARTESIAN_POINT('Ctrl Pts',(38.2207268975965,-5.54346485373421,6.44317352589573));
#28687=CARTESIAN_POINT('Ctrl Pts',(39.7068665331337,-5.5406502123405,9.49693145709774));
#28688=CARTESIAN_POINT('Ctrl Pts',(42.3603417004027,-5.70567308221891,11.6101975146502));
#28689=CARTESIAN_POINT('Ctrl Pts',(45.0138168676718,-5.87069595209734,13.7234635722027));
#28690=CARTESIAN_POINT('Ctrl Pts',(48.31511438115,-6.12886161372555,14.4776794959001));
#28691=CARTESIAN_POINT('Ctrl Pts',(51.6164118946282,-6.38702727535376,15.2318954195974));
#28692=CARTESIAN_POINT('Ctrl Pts',(54.9177094081065,-6.64519293698195,14.4776794959001));
#28693=CARTESIAN_POINT('Ctrl Pts',(37.2260157227862,-6.55512420987448,0.));
#28694=CARTESIAN_POINT('Ctrl Pts',(37.256511759559,-6.34301961518571,3.24562220582792));
#28695=CARTESIAN_POINT('Ctrl Pts',(38.6808968181789,-6.33132600607645,6.16982677025168));
#28696=CARTESIAN_POINT('Ctrl Pts',(40.1052818767988,-6.31963239696717,9.09403133467541));
#28697=CARTESIAN_POINT('Ctrl Pts',(42.647479141562,-6.46865591986398,11.1176436806954));
#28698=CARTESIAN_POINT('Ctrl Pts',(45.1896764063252,-6.61767944276075,13.1412560267153));
#28699=CARTESIAN_POINT('Ctrl Pts',(48.3522126450341,-6.85589424503005,13.8634749112255));
#28700=CARTESIAN_POINT('Ctrl Pts',(51.5147488837429,-7.09410904729936,14.5856937957357));
#28701=CARTESIAN_POINT('Ctrl Pts',(54.6772851224518,-7.33232384956867,13.8634749112255));
#28702=CARTESIAN_POINT('',(36.9500337175455,-5.31261783613237,1.46702345117554E-29));
#28703=CARTESIAN_POINT('Origin',(38.7317130208009,-5.56877962163409,0.));
#28704=CARTESIAN_POINT('Origin',(38.7317130208009,-5.56877962163409,0.));
#28705=CARTESIAN_POINT('Ctrl Pts',(35.9142171164209,-11.7862169042736,0.));
#28706=CARTESIAN_POINT('Ctrl Pts',(35.9745883786012,-11.5806112670705,3.24562220582793));
#28707=CARTESIAN_POINT('Ctrl Pts',(37.3861394252072,-11.7717478112976,6.16982677025167));
#28708=CARTESIAN_POINT('Ctrl Pts',(38.7976904718132,-11.9628843555247,9.09403133467541));
#28709=CARTESIAN_POINT('Ctrl Pts',(41.2928035754069,-12.4721834264261,11.1176436806954));
#28710=CARTESIAN_POINT('Ctrl Pts',(43.7879166790006,-12.9814824973275,13.1412560267153));
#28711=CARTESIAN_POINT('Ctrl Pts',(46.8843613577409,-13.6673484497324,13.8634749112255));
#28712=CARTESIAN_POINT('Ctrl Pts',(49.9808060364812,-14.3532144021372,14.5856937957357));
#28713=CARTESIAN_POINT('Ctrl Pts',(53.0772507152214,-15.039080354542,13.8634749112255));
#28714=CARTESIAN_POINT('Ctrl Pts',(38.0827145049531,-12.7462230199164,0.));
#28715=CARTESIAN_POINT('Ctrl Pts',(38.1430857671334,-12.5406173827133,2.70899372698069));
#28716=CARTESIAN_POINT('Ctrl Pts',(39.3312338708265,-12.6661569043007,5.14971273833323));
#28717=CARTESIAN_POINT('Ctrl Pts',(40.5193819745196,-12.7916964258881,7.59043174968578));
#28718=CARTESIAN_POINT('Ctrl Pts',(42.6119368849886,-13.1827937463388,9.27946171175752));
#28719=CARTESIAN_POINT('Ctrl Pts',(44.7044917954577,-13.5738910667894,10.9684916738293));
#28720=CARTESIAN_POINT('Ctrl Pts',(47.2989546180621,-14.1123618472584,11.5712994880388));
#28721=CARTESIAN_POINT('Ctrl Pts',(49.8934174406666,-14.6508326277274,12.1741073022483));
#28722=CARTESIAN_POINT('Ctrl Pts',(52.487880263271,-15.1893034081963,11.5712994880388));
#28723=CARTESIAN_POINT('Ctrl Pts',(40.0222531270432,-14.1108411348349,0.));
#28724=CARTESIAN_POINT('Ctrl Pts',(40.0826243892235,-13.9052354976318,2.19648874705824));
#28725=CARTESIAN_POINT('Ctrl Pts',(41.0574123652205,-13.9681268331909,4.17545672685568));
#28726=CARTESIAN_POINT('Ctrl Pts',(42.0322003412175,-14.03101816875,6.15442470665314));
#28727=CARTESIAN_POINT('Ctrl Pts',(43.7402935862748,-14.3092273587166,7.5239130403414));
#28728=CARTESIAN_POINT('Ctrl Pts',(45.4483868313321,-14.5874365486831,8.89340137402968));
#28729=CARTESIAN_POINT('Ctrl Pts',(47.5634337987568,-14.9851381329366,9.38216610144961));
#28730=CARTESIAN_POINT('Ctrl Pts',(49.6784807661816,-15.3828397171901,9.87093082886955));
#28731=CARTESIAN_POINT('Ctrl Pts',(51.7935277336064,-15.7805413014436,9.38216610144961));
#28732=CARTESIAN_POINT('Ctrl Pts',(41.6582954965891,-15.8276282594352,0.));
#28733=CARTESIAN_POINT('Ctrl Pts',(41.7186667587694,-15.6220226222321,1.72780310113343));
#28734=CARTESIAN_POINT('Ctrl Pts',(42.4983369638542,-15.6276222110084,3.28449990511991));
#28735=CARTESIAN_POINT('Ctrl Pts',(43.2780071689391,-15.6332217997846,4.84119670910639));
#28736=CARTESIAN_POINT('Ctrl Pts',(44.6345103396636,-15.8081948292729,5.91846432228298));
#28737=CARTESIAN_POINT('Ctrl Pts',(45.9910135103882,-15.9831678587611,6.99573193545957));
#28738=CARTESIAN_POINT('Ctrl Pts',(47.6676348262506,-16.2521360565322,7.38020429521639));
#28739=CARTESIAN_POINT('Ctrl Pts',(49.344256142113,-16.5211042543032,7.76467665497321));
#28740=CARTESIAN_POINT('Ctrl Pts',(51.0208774579753,-16.7900724520742,7.38020429521639));
#28741=CARTESIAN_POINT('',(35.9142171164435,-11.7862169042834,1.57948957610185E-9));
#28742=CARTESIAN_POINT('Origin',(28.6276304970122,-28.2454287759841,0.));
#28743=CARTESIAN_POINT('Ctrl Pts',(35.9142171165573,-11.7862169041099,3.13105350628993E-9));
#28744=CARTESIAN_POINT('Ctrl Pts',(35.9187750292272,-11.7706940792792,0.245038153335639));
#28745=CARTESIAN_POINT('Ctrl Pts',(35.9294543009581,-11.7568199184781,0.490791160522051));
#28746=CARTESIAN_POINT('Ctrl Pts',(35.9463285033517,-11.7446485667476,0.736766500725875));
#28747=CARTESIAN_POINT('Ctrl Pts',(35.9631473086864,-11.7325171728813,0.981934317701509));
#28748=CARTESIAN_POINT('Ctrl Pts',(35.9861205266374,-11.7220774809613,1.22732257376614));
#28749=CARTESIAN_POINT('Ctrl Pts',(36.0152719968248,-11.713370240977,1.47243294816389));
#28750=CARTESIAN_POINT('Ctrl Pts',(36.0443795639103,-11.7046761143913,1.71717417803068));
#28751=CARTESIAN_POINT('Ctrl Pts',(36.079646826587,-11.6977092667639,1.96163791541639));
#28752=CARTESIAN_POINT('Ctrl Pts',(36.1210475853283,-11.6924966907345,2.2053240877858));
#28753=CARTESIAN_POINT('Ctrl Pts',(36.1624128366599,-11.687288585277,2.4488012624212));
#28754=CARTESIAN_POINT('Ctrl Pts',(36.2099010442177,-11.6838317679615,2.69150175431102));
#28755=CARTESIAN_POINT('Ctrl Pts',(36.2634360706163,-11.6821391062288,2.93292951866858));
#28756=CARTESIAN_POINT('Ctrl Pts',(36.3169598973807,-11.6804467986043,3.17430677585647));
#28757=CARTESIAN_POINT('Ctrl Pts',(36.3765279276399,-11.6805179152423,3.41441139318408));
#28758=CARTESIAN_POINT('Ctrl Pts',(36.442014877408,-11.6823510237344,3.65275710614708));
#28759=CARTESIAN_POINT('Ctrl Pts',(36.5075849814588,-11.6841864598785,3.89140546668862));
#28760=CARTESIAN_POINT('Ctrl Pts',(36.579088906284,-11.6877883562712,4.1282900208124));
#28761=CARTESIAN_POINT('Ctrl Pts',(36.6563532415796,-11.6931409581038,4.36293874377886));
#28762=CARTESIAN_POINT('Ctrl Pts',(36.7336964173084,-11.6984990217247,4.59782690201532));
#28763=CARTESIAN_POINT('Ctrl Pts',(36.8168115609902,-11.7056113365133,4.83047425895048));
#28764=CARTESIAN_POINT('Ctrl Pts',(36.9054796074173,-11.714448049605,5.06042975959526));
#28765=CARTESIAN_POINT('Ctrl Pts',(36.9944068844552,-11.723310597782,5.291057559984));
#28766=CARTESIAN_POINT('Ctrl Pts',(37.0889193314435,-11.7339075987039,5.51897736305783));
#28767=CARTESIAN_POINT('Ctrl Pts',(37.1887539873585,-11.7461953488412,5.74376259354426));
#28768=CARTESIAN_POINT('Ctrl Pts',(37.252411532658,-11.7540303837179,5.88709234072682));
#28769=CARTESIAN_POINT('Ctrl Pts',(37.318232100817,-11.7625525566678,6.02914825314224));
#28770=CARTESIAN_POINT('Ctrl Pts',(37.3861394252393,-11.7717478113124,6.16982677023484));
#28771=CARTESIAN_POINT('Ctrl Pts',(37.4926201075705,-11.7861662410928,6.39041482339093));
#28772=CARTESIAN_POINT('Ctrl Pts',(37.6049078439221,-11.8021412942478,6.60890054011811));
#28773=CARTESIAN_POINT('Ctrl Pts',(37.7228633758095,-11.8196645413942,6.8248041200805));
#28774=CARTESIAN_POINT('Ctrl Pts',(37.8405526164631,-11.8371482288266,7.04022028559291));
#28775=CARTESIAN_POINT('Ctrl Pts',(37.9638839981996,-11.8561731288313,7.25306552029626));
#28776=CARTESIAN_POINT('Ctrl Pts',(38.0926705666681,-11.876718115565,7.46287566269397));
#28777=CARTESIAN_POINT('Ctrl Pts',(38.2212499935677,-11.8972300575423,7.67234834441866));
#28778=CARTESIAN_POINT('Ctrl Pts',(38.3552669199725,-11.9192571854562,7.87879526533018));
#28779=CARTESIAN_POINT('Ctrl Pts',(38.4944885898566,-11.9427658506833,8.08177334612189));
#28780=CARTESIAN_POINT('Ctrl Pts',(38.6335766715385,-11.9662519585001,8.28455666214066));
#28781=CARTESIAN_POINT('Ctrl Pts',(38.7778593027053,-11.9912167312945,8.48387739272773));
#28782=CARTESIAN_POINT('Ctrl Pts',(38.9270604658997,-12.0176143452911,8.67931873610978));
#28783=CARTESIAN_POINT('Ctrl Pts',(39.0762688052756,-12.0440132289432,8.87476947970365));
#28784=CARTESIAN_POINT('Ctrl Pts',(39.2303958882193,-12.071845046704,9.06634009532691));
#28785=CARTESIAN_POINT('Ctrl Pts',(39.3891252359316,-12.1010522527169,9.25364450340837));
#28786=CARTESIAN_POINT('Ctrl Pts',(39.5479128119385,-12.130270173105,9.44101762226336));
#28787=CARTESIAN_POINT('Ctrl Pts',(39.7113057183244,-12.1608644313195,9.62412107874861));
#28788=CARTESIAN_POINT('Ctrl Pts',(39.8789509826175,-12.1927664798388,9.80260437465941));
#28789=CARTESIAN_POINT('Ctrl Pts',(40.0468697110609,-12.2247205672071,9.9813788137949));
#28790=CARTESIAN_POINT('Ctrl Pts',(40.219054331768,-12.2579866432889,10.1555177270905));
#28791=CARTESIAN_POINT('Ctrl Pts',(40.3951188515048,-12.2924858372374,10.3247095747688));
#28792=CARTESIAN_POINT('Ctrl Pts',(40.4460074573685,-12.3024572720619,10.3736117457726));
#28793=CARTESIAN_POINT('Ctrl Pts',(40.4972200117257,-12.3125316625314,10.4221009095717));
#28794=CARTESIAN_POINT('Ctrl Pts',(40.5487467751689,-12.3227069631099,10.4701702229062));
#28795=CARTESIAN_POINT('Ctrl Pts',(43.602250138795,-9.2071267414952,0.));
#28796=CARTESIAN_POINT('Ctrl Pts',(43.6626214009753,-9.00152110429209,1.72780310113343));
#28797=CARTESIAN_POINT('Ctrl Pts',(44.4422916060602,-9.00712069306833,3.28449990511991));
#28798=CARTESIAN_POINT('Ctrl Pts',(45.2219618111451,-9.01272028184456,4.84119670910638));
#28799=CARTESIAN_POINT('Ctrl Pts',(46.5784649818696,-9.18769331133286,5.91846432228298));
#28800=CARTESIAN_POINT('Ctrl Pts',(47.9349681525942,-9.36266634082112,6.99573193545957));
#28801=CARTESIAN_POINT('Ctrl Pts',(49.6115894684565,-9.63163453859214,7.38020429521639));
#28802=CARTESIAN_POINT('Ctrl Pts',(51.2882107843189,-9.90060273636318,7.76467665497322));
#28803=CARTESIAN_POINT('Ctrl Pts',(52.9648321001812,-10.1695709341342,7.38020429521639));
#28804=CARTESIAN_POINT('Ctrl Pts',(41.2977585211119,-9.76686869112097,0.));
#28805=CARTESIAN_POINT('Ctrl Pts',(41.3581297832922,-9.56126305391789,2.19648874705823));
#28806=CARTESIAN_POINT('Ctrl Pts',(42.3329177592892,-9.624154389477,4.17545672685569));
#28807=CARTESIAN_POINT('Ctrl Pts',(43.3077057352862,-9.68704572503613,6.15442470665315));
#28808=CARTESIAN_POINT('Ctrl Pts',(45.0157989803434,-9.96525491500266,7.52391304034141));
#28809=CARTESIAN_POINT('Ctrl Pts',(46.7238922254007,-10.2434641049692,8.89340137402968));
#28810=CARTESIAN_POINT('Ctrl Pts',(48.8389391928255,-10.6411656892227,9.38216610144961));
#28811=CARTESIAN_POINT('Ctrl Pts',(50.9539861602503,-11.0388672734762,9.87093082886955));
#28812=CARTESIAN_POINT('Ctrl Pts',(53.0690331276751,-11.4365688577297,9.38216610144962));
#28813=CARTESIAN_POINT('Ctrl Pts',(38.9283465500518,-9.86626475512805,0.));
#28814=CARTESIAN_POINT('Ctrl Pts',(38.9887178122321,-9.66065911792495,2.70899372698069));
#28815=CARTESIAN_POINT('Ctrl Pts',(40.1768659159253,-9.78619863951237,5.14971273833323));
#28816=CARTESIAN_POINT('Ctrl Pts',(41.3650140196183,-9.91173816109979,7.59043174968577));
#28817=CARTESIAN_POINT('Ctrl Pts',(43.4575689300874,-10.3028354815504,9.27946171175751));
#28818=CARTESIAN_POINT('Ctrl Pts',(45.5501238405564,-10.693932802001,10.9684916738293));
#28819=CARTESIAN_POINT('Ctrl Pts',(48.1445866631608,-11.23240358247,11.5712994880388));
#28820=CARTESIAN_POINT('Ctrl Pts',(50.7390494857653,-11.770874362939,12.1741073022483));
#28821=CARTESIAN_POINT('Ctrl Pts',(53.3335123083697,-12.309345143408,11.5712994880388));
#28822=CARTESIAN_POINT('Ctrl Pts',(36.5850719698904,-9.50149509066561,0.));
#28823=CARTESIAN_POINT('Ctrl Pts',(36.6454432320707,-9.2958894534625,3.24562220582793));
#28824=CARTESIAN_POINT('Ctrl Pts',(38.0569942786767,-9.48702599768955,6.16982677025167));
#28825=CARTESIAN_POINT('Ctrl Pts',(39.4685453252828,-9.6781625419166,9.09403133467541));
#28826=CARTESIAN_POINT('Ctrl Pts',(41.9636584288764,-10.1874616128181,11.1176436806954));
#28827=CARTESIAN_POINT('Ctrl Pts',(44.4587715324701,-10.6967606837195,13.1412560267153));
#28828=CARTESIAN_POINT('Ctrl Pts',(47.5552162112104,-11.3826266361243,13.8634749112255));
#28829=CARTESIAN_POINT('Ctrl Pts',(50.6516608899507,-12.0684925885292,14.5856937957357));
#28830=CARTESIAN_POINT('Ctrl Pts',(53.748105568691,-12.754358540934,13.8634749112255));
#28831=CARTESIAN_POINT('',(36.5850719698904,-9.50149509066561,0.));
#28832=CARTESIAN_POINT('Ctrl Pts',(36.5850719698904,-9.50149509066561,0.));
#28833=CARTESIAN_POINT('Ctrl Pts',(36.6454432320707,-9.2958894534625,3.24562220582793));
#28834=CARTESIAN_POINT('Ctrl Pts',(38.0569942786767,-9.48702599768957,6.16982677025167));
#28835=CARTESIAN_POINT('Ctrl Pts',(39.2354107742189,-9.64659405380744,8.61106394926976));
#28836=CARTESIAN_POINT('Ctrl Pts',(41.196861549629,-10.0334970568411,10.4489096280657));
#28837=CARTESIAN_POINT('Origin',(39.3537269950292,8.28430119040582,0.));
#28838=CARTESIAN_POINT('Ctrl Pts',(36.5850719698904,-9.50149509066561,0.));
#28839=CARTESIAN_POINT('Ctrl Pts',(36.6454432320707,-9.2958894534625,3.24562220582793));
#28840=CARTESIAN_POINT('Ctrl Pts',(38.0569942786767,-9.48702599768957,6.16982677025167));
#28841=CARTESIAN_POINT('Ctrl Pts',(39.4685453252828,-9.67816254191661,9.09403133467541));
#28842=CARTESIAN_POINT('Ctrl Pts',(41.9636584288765,-10.187461612818,11.1176436806954));
#28843=CARTESIAN_POINT('Ctrl Pts',(44.4587715324701,-10.6967606837195,13.1412560267153));
#28844=CARTESIAN_POINT('Ctrl Pts',(47.5552162112104,-11.3826266361243,13.8634749112255));
#28845=CARTESIAN_POINT('Ctrl Pts',(50.6516608899507,-12.0684925885292,14.5856937957357));
#28846=CARTESIAN_POINT('Ctrl Pts',(53.748105568691,-12.754358540934,13.8634749112255));
#28847=CARTESIAN_POINT('Ctrl Pts',(35.7793349404724,-10.0094201239379,0.));
#28848=CARTESIAN_POINT('Ctrl Pts',(35.8397062026527,-9.80381448673481,3.38941559469373));
#28849=CARTESIAN_POINT('Ctrl Pts',(37.3111196447713,-10.0125282162151,6.44317352589573));
#28850=CARTESIAN_POINT('Ctrl Pts',(38.7825330868899,-10.2212419456954,9.49693145709775));
#28851=CARTESIAN_POINT('Ctrl Pts',(41.3855144999132,-10.7622140099939,11.6101975146502));
#28852=CARTESIAN_POINT('Ctrl Pts',(43.9884959129366,-11.3031860742923,13.7234635722027));
#28853=CARTESIAN_POINT('Ctrl Pts',(47.2194501734232,-12.028547603452,14.4776794959001));
#28854=CARTESIAN_POINT('Ctrl Pts',(50.4504044339098,-12.7539091326116,15.2318954195974));
#28855=CARTESIAN_POINT('Ctrl Pts',(53.6813586943964,-13.4792706617712,14.4776794959001));
#28856=CARTESIAN_POINT('Ctrl Pts',(35.5109929990846,-10.9233088493811,0.));
#28857=CARTESIAN_POINT('Ctrl Pts',(35.5713642612649,-10.717703212178,3.38941559469372));
#28858=CARTESIAN_POINT('Ctrl Pts',(37.0427777033835,-10.9264169416583,6.44317352589573));
#28859=CARTESIAN_POINT('Ctrl Pts',(38.514191145502,-11.1351306711386,9.49693145709775));
#28860=CARTESIAN_POINT('Ctrl Pts',(41.1171725585254,-11.6761027354371,11.6101975146502));
#28861=CARTESIAN_POINT('Ctrl Pts',(43.7201539715488,-12.2170747997355,13.7234635722027));
#28862=CARTESIAN_POINT('Ctrl Pts',(46.9511082320354,-12.9424363288952,14.4776794959001));
#28863=CARTESIAN_POINT('Ctrl Pts',(50.182062492522,-13.6677978580548,15.2318954195974));
#28864=CARTESIAN_POINT('Ctrl Pts',(53.4130167530086,-14.3931593872144,14.4776794959001));
#28865=CARTESIAN_POINT('Ctrl Pts',(35.9142171164209,-11.7862169042736,0.));
#28866=CARTESIAN_POINT('Ctrl Pts',(35.9745883786012,-11.5806112670705,3.24562220582793));
#28867=CARTESIAN_POINT('Ctrl Pts',(37.3861394252072,-11.7717478112976,6.16982677025167));
#28868=CARTESIAN_POINT('Ctrl Pts',(38.7976904718132,-11.9628843555247,9.09403133467541));
#28869=CARTESIAN_POINT('Ctrl Pts',(41.2928035754069,-12.4721834264261,11.1176436806954));
#28870=CARTESIAN_POINT('Ctrl Pts',(43.7879166790006,-12.9814824973275,13.1412560267153));
#28871=CARTESIAN_POINT('Ctrl Pts',(46.8843613577409,-13.6673484497324,13.8634749112255));
#28872=CARTESIAN_POINT('Ctrl Pts',(49.9808060364812,-14.3532144021372,14.5856937957357));
#28873=CARTESIAN_POINT('Ctrl Pts',(53.0772507152214,-15.039080354542,13.8634749112255));
#28874=CARTESIAN_POINT('',(35.8178713036688,-10.5170811195104,1.62623179273832E-29));
#28875=CARTESIAN_POINT('Origin',(37.5449600575352,-11.0241949492056,0.));
#28876=CARTESIAN_POINT('Origin',(37.5449600575352,-11.0241949492056,0.));
#28877=CARTESIAN_POINT('Ctrl Pts',(33.871308617615,-16.7773762111447,0.));
#28878=CARTESIAN_POINT('Ctrl Pts',(33.9603261204011,-16.582455069283,3.24562220582793));
#28879=CARTESIAN_POINT('Ctrl Pts',(35.3303080462614,-16.9725307779982,6.16982677025168));
#28880=CARTESIAN_POINT('Ctrl Pts',(36.7002899721218,-17.3626064867134,9.09403133467541));
#28881=CARTESIAN_POINT('Ctrl Pts',(39.0975256070688,-18.2218132452332,11.1176436806954));
#28882=CARTESIAN_POINT('Ctrl Pts',(41.4947612420158,-19.0810200037529,13.1412560267153));
#28883=CARTESIAN_POINT('Ctrl Pts',(44.4620796765374,-20.2005748533764,13.8634749112255));
#28884=CARTESIAN_POINT('Ctrl Pts',(47.4293981110591,-21.3201297029999,14.5856937957357));
#28885=CARTESIAN_POINT('Ctrl Pts',(50.3967165455806,-22.4396845526234,13.8634749112255));
#28886=CARTESIAN_POINT('Ctrl Pts',(35.881110714358,-18.0362202038897,0.));
#28887=CARTESIAN_POINT('Ctrl Pts',(35.9701282171441,-17.841299062028,2.70899372698069));
#28888=CARTESIAN_POINT('Ctrl Pts',(37.1283165495981,-18.1346518775205,5.14971273833323));
#28889=CARTESIAN_POINT('Ctrl Pts',(38.2865048820521,-18.428004693013,7.59043174968578));
#28890=CARTESIAN_POINT('Ctrl Pts',(40.3021016488385,-19.1129228203186,9.27946171175752));
#28891=CARTESIAN_POINT('Ctrl Pts',(42.3176984156249,-19.7978409476242,10.9684916738293));
#28892=CARTESIAN_POINT('Ctrl Pts',(44.8091209655643,-20.7000614289637,11.5712994880388));
#28893=CARTESIAN_POINT('Ctrl Pts',(47.3005435155039,-21.6022819103033,12.1741073022483));
#28894=CARTESIAN_POINT('Ctrl Pts',(49.7919660654433,-22.5045023916429,11.5712994880388));
#28895=CARTESIAN_POINT('Ctrl Pts',(37.6067022235295,-19.6629735993427,0.));
#28896=CARTESIAN_POINT('Ctrl Pts',(37.6957197263156,-19.468052457481,2.19648874705823));
#28897=CARTESIAN_POINT('Ctrl Pts',(38.6516353959963,-19.6690304430807,4.17545672685568));
#28898=CARTESIAN_POINT('Ctrl Pts',(39.607551065677,-19.8700084286804,6.15442470665314));
#28899=CARTESIAN_POINT('Ctrl Pts',(41.2586650884904,-20.3884728641637,7.5239130403414));
#28900=CARTESIAN_POINT('Ctrl Pts',(42.9097791113038,-20.9069372996469,8.89340137402966));
#28901=CARTESIAN_POINT('Ctrl Pts',(44.946699113602,-21.6015934223205,9.38216610144959));
#28902=CARTESIAN_POINT('Ctrl Pts',(46.9836191159003,-22.2962495449941,9.87093082886953));
#28903=CARTESIAN_POINT('Ctrl Pts',(49.0205391181984,-22.9909056676677,9.3821661014496));
#28904=CARTESIAN_POINT('Ctrl Pts',(38.9817677587446,-21.5951194116474,0.));
#28905=CARTESIAN_POINT('Ctrl Pts',(39.0707852615307,-21.4001982697857,1.72780310113343));
#28906=CARTESIAN_POINT('Ctrl Pts',(39.8417226435483,-21.5166995019653,3.28449990511991));
#28907=CARTESIAN_POINT('Ctrl Pts',(40.6126600255659,-21.6332007341449,4.84119670910639));
#28908=CARTESIAN_POINT('Ctrl Pts',(41.9304546915347,-21.9994433198421,5.91846432228298));
#28909=CARTESIAN_POINT('Ctrl Pts',(43.2482493575035,-22.3656859055393,6.99573193545955));
#28910=CARTESIAN_POINT('Ctrl Pts',(44.8695269202923,-22.8705244862897,7.38020429521639));
#28911=CARTESIAN_POINT('Ctrl Pts',(46.4908044830811,-23.37536306704,7.76467665497322));
#28912=CARTESIAN_POINT('Ctrl Pts',(48.1120820458698,-23.8802016477904,7.38020429521639));
#28913=CARTESIAN_POINT('',(33.871308617636,-16.7773762111576,1.57949292205503E-9));
#28914=CARTESIAN_POINT('Origin',(24.3164988679733,-32.0320676419195,0.));
#28915=CARTESIAN_POINT('Ctrl Pts',(33.8713086177734,-16.777376211002,3.13106037980953E-9));
#28916=CARTESIAN_POINT('Ctrl Pts',(33.8780292657696,-16.7626600447505,0.245038153335595));
#28917=CARTESIAN_POINT('Ctrl Pts',(33.8905743368631,-16.7504469217307,0.490791160521955));
#28918=CARTESIAN_POINT('Ctrl Pts',(33.90900894816,-16.7408009061958,0.736766500725727));
#28919=CARTESIAN_POINT('Ctrl Pts',(33.9273830396632,-16.7311865579883,0.981934317701375));
#28920=CARTESIAN_POINT('Ctrl Pts',(33.9516081464472,-16.7241225568764,1.22732257376602));
#28921=CARTESIAN_POINT('Ctrl Pts',(33.9817020661513,-16.7196526308056,1.47243294816379));
#28922=CARTESIAN_POINT('Ctrl Pts',(34.0117506633924,-16.7151894365949,1.71717417803055));
#28923=CARTESIAN_POINT('Ctrl Pts',(34.0476504419797,-16.7133125562152,1.96163791541624));
#28924=CARTESIAN_POINT('Ctrl Pts',(34.0893716276066,-16.7140449789785,2.20532408778562));
#28925=CARTESIAN_POINT('Ctrl Pts',(34.1310570310093,-16.7147767735785,2.44880126242103));
#28926=CARTESIAN_POINT('Ctrl Pts',(34.1785538334837,-16.7181134182575,2.69150175431087));
#28927=CARTESIAN_POINT('Ctrl Pts',(34.2317848413854,-16.7240568140044,2.93292951866844));
#28928=CARTESIAN_POINT('Ctrl Pts',(34.2850047132542,-16.7299989663812,3.17430677585624));
#28929=CARTESIAN_POINT('Ctrl Pts',(34.3439563059025,-16.7385467737469,3.41441139318376));
#28930=CARTESIAN_POINT('Ctrl Pts',(34.4085158144078,-16.749680988503,3.65275710614667));
#28931=CARTESIAN_POINT('Ctrl Pts',(34.4731572995456,-16.7608293413071,3.89140546668821));
#28932=CARTESIAN_POINT('Ctrl Pts',(34.5434208142135,-16.7745706450855,4.12829002081199));
#28933=CARTESIAN_POINT('Ctrl Pts',(34.6191369553176,-16.7908646265311,4.36293874377845));
#28934=CARTESIAN_POINT('Ctrl Pts',(34.6949303570795,-16.8071752343354,4.59782690201486));
#28935=CARTESIAN_POINT('Ctrl Pts',(34.7761873205119,-16.8260436742457,4.83047425894996));
#28936=CARTESIAN_POINT('Ctrl Pts',(34.8626952586805,-16.8474092210269,5.06042975959468));
#28937=CARTESIAN_POINT('Ctrl Pts',(34.9494561121503,-16.8688372322919,5.29105755998348));
#28938=CARTESIAN_POINT('Ctrl Pts',(35.0414984482316,-16.8927768946321,5.51897736305738));
#28939=CARTESIAN_POINT('Ctrl Pts',(35.1385682021255,-16.9191475261011,5.74376259354388));
#28940=CARTESIAN_POINT('Ctrl Pts',(35.2004627636792,-16.9359622248841,5.88709234072657));
#28941=CARTESIAN_POINT('Ctrl Pts',(35.2644005416947,-16.9537648979139,6.02914825314211));
#28942=CARTESIAN_POINT('Ctrl Pts',(35.3303080462911,-16.9725307780174,6.16982677023484));
#28943=CARTESIAN_POINT('Ctrl Pts',(35.4336529523063,-17.0019562300575,6.39041482339096));
#28944=CARTESIAN_POINT('Ctrl Pts',(35.5425242743013,-17.0337488912445,6.60890054011815));
#28945=CARTESIAN_POINT('Ctrl Pts',(35.6567853708682,-17.0678805994453,6.82480412008056));
#28946=CARTESIAN_POINT('Ctrl Pts',(35.7707885165964,-17.1019352533992,7.04022028559298));
#28947=CARTESIAN_POINT('Ctrl Pts',(35.8901570371288,-17.1383183929993,7.25306552029635));
#28948=CARTESIAN_POINT('Ctrl Pts',(36.0147088875608,-17.1769825010549,7.46287566269407));
#28949=CARTESIAN_POINT('Ctrl Pts',(36.1390604075855,-17.2155844213831,7.6723483444187));
#28950=CARTESIAN_POINT('Ctrl Pts',(36.2685784477692,-17.2564599421026,7.87879526533015));
#28951=CARTESIAN_POINT('Ctrl Pts',(36.4030374099052,-17.299542632448,8.0817733461218));
#28952=CARTESIAN_POINT('Ctrl Pts',(36.5373673538287,-17.3425839834018,8.28455666214107));
#28953=CARTESIAN_POINT('Ctrl Pts',(36.6766285382462,-17.3878282101257,8.48387739272861));
#28954=CARTESIAN_POINT('Ctrl Pts',(36.8205542765633,-17.4351906738843,8.67931873611112));
#28955=CARTESIAN_POINT('Ctrl Pts',(36.9644869373274,-17.4825554156522,8.87476947970492));
#28956=CARTESIAN_POINT('Ctrl Pts',(37.1130843481561,-17.532038516521,9.06634009532812));
#28957=CARTESIAN_POINT('Ctrl Pts',(37.2660414411774,-17.5835379767389,9.2536445034095));
#28958=CARTESIAN_POINT('Ctrl Pts',(37.4190546449988,-17.6350563290255,9.4410176222646));
#28959=CARTESIAN_POINT('Ctrl Pts',(37.576430430281,-17.6885924168519,9.62412107874996));
#28960=CARTESIAN_POINT('Ctrl Pts',(37.7378291726326,-17.7440281571915,9.80260437466087));
#28961=CARTESIAN_POINT('Ctrl Pts',(37.8994911897635,-17.7995543247059,9.98137881379659));
#28962=CARTESIAN_POINT('Ctrl Pts',(38.0651889630643,-17.8569862265482,10.1555177270924));
#28963=CARTESIAN_POINT('Ctrl Pts',(38.2345516526472,-17.9161908620981,10.3247095747709));
#28964=CARTESIAN_POINT('Ctrl Pts',(38.2835032027451,-17.9333030058075,10.3736117457756));
#28965=CARTESIAN_POINT('Ctrl Pts',(38.3327607518919,-17.9505631598993,10.4221009095757));
#28966=CARTESIAN_POINT('Ctrl Pts',(38.3823149509235,-17.9679679135961,10.4701702229111));
#28967=CARTESIAN_POINT('Ctrl Pts',(41.8481313484576,-15.3186586437012,0.));
#28968=CARTESIAN_POINT('Ctrl Pts',(41.9371488512437,-15.1237375018396,1.72780310113343));
#28969=CARTESIAN_POINT('Ctrl Pts',(42.7080862332614,-15.2402387340191,3.28449990511991));
#28970=CARTESIAN_POINT('Ctrl Pts',(43.479023615279,-15.3567399661987,4.84119670910638));
#28971=CARTESIAN_POINT('Ctrl Pts',(44.7968182812478,-15.722982551896,5.91846432228297));
#28972=CARTESIAN_POINT('Ctrl Pts',(46.1146129472166,-16.0892251375932,6.99573193545956));
#28973=CARTESIAN_POINT('Ctrl Pts',(47.7358905100054,-16.5940637183435,7.38020429521639));
#28974=CARTESIAN_POINT('Ctrl Pts',(49.3571680727942,-17.0989022990938,7.76467665497322));
#28975=CARTESIAN_POINT('Ctrl Pts',(50.9784456355829,-17.6037408798442,7.38020429521639));
#28976=CARTESIAN_POINT('Ctrl Pts',(39.4874365476042,-15.5447398754884,0.));
#28977=CARTESIAN_POINT('Ctrl Pts',(39.5764540503904,-15.3498187336267,2.19648874705824));
#28978=CARTESIAN_POINT('Ctrl Pts',(40.532369720071,-15.5507967192264,4.17545672685568));
#28979=CARTESIAN_POINT('Ctrl Pts',(41.4882853897517,-15.7517747048261,6.15442470665313));
#28980=CARTESIAN_POINT('Ctrl Pts',(43.1393994125651,-16.2702391403093,7.5239130403414));
#28981=CARTESIAN_POINT('Ctrl Pts',(44.7905134353786,-16.7887035757925,8.89340137402968));
#28982=CARTESIAN_POINT('Ctrl Pts',(46.8274334376768,-17.4833596984661,9.3821661014496));
#28983=CARTESIAN_POINT('Ctrl Pts',(48.864353439975,-18.1780158211397,9.87093082886952));
#28984=CARTESIAN_POINT('Ctrl Pts',(50.9012734422732,-18.8726719438133,9.3821661014496));
#28985=CARTESIAN_POINT('Ctrl Pts',(37.1279962392254,-15.3059217494169,0.));
#28986=CARTESIAN_POINT('Ctrl Pts',(37.2170137420116,-15.1110006075553,2.70899372698069));
#28987=CARTESIAN_POINT('Ctrl Pts',(38.3752020744656,-15.4043534230478,5.14971273833323));
#28988=CARTESIAN_POINT('Ctrl Pts',(39.5333904069196,-15.6977062385402,7.59043174968578));
#28989=CARTESIAN_POINT('Ctrl Pts',(41.548987173706,-16.3826243658458,9.27946171175751));
#28990=CARTESIAN_POINT('Ctrl Pts',(43.5645839404924,-17.0675424931514,10.9684916738293));
#28991=CARTESIAN_POINT('Ctrl Pts',(46.0560064904318,-17.969762974491,11.5712994880388));
#28992=CARTESIAN_POINT('Ctrl Pts',(48.5474290403713,-18.8719834558305,12.1741073022483));
#28993=CARTESIAN_POINT('Ctrl Pts',(51.0388515903108,-19.7742039371701,11.5712994880388));
#28994=CARTESIAN_POINT('Ctrl Pts',(34.8604849513721,-14.6113821712787,0.));
#28995=CARTESIAN_POINT('Ctrl Pts',(34.9495024541582,-14.416461029417,3.24562220582792));
#28996=CARTESIAN_POINT('Ctrl Pts',(36.3194843800186,-14.8065367381322,6.16982677025167));
#28997=CARTESIAN_POINT('Ctrl Pts',(37.6894663058789,-15.1966124468474,9.09403133467541));
#28998=CARTESIAN_POINT('Ctrl Pts',(40.086701940826,-16.0558192053672,11.1176436806954));
#28999=CARTESIAN_POINT('Ctrl Pts',(42.483937575773,-16.9150259638869,13.1412560267153));
#29000=CARTESIAN_POINT('Ctrl Pts',(45.4512560102946,-18.0345808135104,13.8634749112255));
#29001=CARTESIAN_POINT('Ctrl Pts',(48.4185744448162,-19.1541356631339,14.5856937957357));
#29002=CARTESIAN_POINT('Ctrl Pts',(51.3858928793377,-20.2736905127574,13.8634749112255));
#29003=CARTESIAN_POINT('',(34.8604849513721,-14.6113821712787,0.));
#29004=CARTESIAN_POINT('Ctrl Pts',(34.8604849513721,-14.6113821712787,0.));
#29005=CARTESIAN_POINT('Ctrl Pts',(34.9495024541582,-14.416461029417,3.24562220582792));
#29006=CARTESIAN_POINT('Ctrl Pts',(36.3194843800186,-14.8065367381322,6.16982677025167));
#29007=CARTESIAN_POINT('Ctrl Pts',(37.4631973926724,-15.1321867744986,8.61106394926975));
#29008=CARTESIAN_POINT('Ctrl Pts',(39.3496213890631,-15.794295212713,10.4489096280657));
#29009=CARTESIAN_POINT('Origin',(40.1321417817282,2.59935965651478,0.));
#29010=CARTESIAN_POINT('Ctrl Pts',(34.8604849513721,-14.6113821712787,0.));
#29011=CARTESIAN_POINT('Ctrl Pts',(34.9495024541582,-14.416461029417,3.24562220582792));
#29012=CARTESIAN_POINT('Ctrl Pts',(36.3194843800186,-14.8065367381322,6.16982677025167));
#29013=CARTESIAN_POINT('Ctrl Pts',(37.6894663058789,-15.1966124468474,9.09403133467541));
#29014=CARTESIAN_POINT('Ctrl Pts',(40.086701940826,-16.0558192053672,11.1176436806954));
#29015=CARTESIAN_POINT('Ctrl Pts',(42.483937575773,-16.9150259638869,13.1412560267153));
#29016=CARTESIAN_POINT('Ctrl Pts',(45.4512560102946,-18.0345808135104,13.8634749112255));
#29017=CARTESIAN_POINT('Ctrl Pts',(48.4185744448162,-19.1541356631339,14.5856937957357));
#29018=CARTESIAN_POINT('Ctrl Pts',(51.3858928793377,-20.2736905127574,13.8634749112255));
#29019=CARTESIAN_POINT('Ctrl Pts',(33.9906638941716,-14.9994689250473,6.24500451351652E-15));
#29020=CARTESIAN_POINT('Ctrl Pts',(34.0796813969578,-14.8045477831856,3.38941559469372));
#29021=CARTESIAN_POINT('Ctrl Pts',(35.5064149111821,-15.2205410738884,6.44317352589573));
#29022=CARTESIAN_POINT('Ctrl Pts',(36.9331484254065,-15.6365343645912,9.49693145709774));
#29023=CARTESIAN_POINT('Ctrl Pts',(39.4326468889936,-16.5424429921152,11.6101975146502));
#29024=CARTESIAN_POINT('Ctrl Pts',(41.9321453525807,-17.4483516196392,13.7234635722027));
#29025=CARTESIAN_POINT('Ctrl Pts',(45.0269834486349,-18.6261427473665,14.4776794959001));
#29026=CARTESIAN_POINT('Ctrl Pts',(48.121821544689,-19.8039338750937,15.2318954195974));
#29027=CARTESIAN_POINT('Ctrl Pts',(51.2166596407432,-20.981725002821,14.4776794959001));
#29028=CARTESIAN_POINT('Ctrl Pts',(33.5949933606688,-15.8658665409937,6.24500451351652E-15));
#29029=CARTESIAN_POINT('Ctrl Pts',(33.6840108634549,-15.670945399132,3.38941559469373));
#29030=CARTESIAN_POINT('Ctrl Pts',(35.1107443776793,-16.0869386898348,6.44317352589574));
#29031=CARTESIAN_POINT('Ctrl Pts',(36.5374778919037,-16.5029319805376,9.49693145709775));
#29032=CARTESIAN_POINT('Ctrl Pts',(39.0369763554907,-17.4088406080616,11.6101975146502));
#29033=CARTESIAN_POINT('Ctrl Pts',(41.5364748190778,-18.3147492355856,13.7234635722027));
#29034=CARTESIAN_POINT('Ctrl Pts',(44.631312915132,-19.4925403633128,14.4776794959001));
#29035=CARTESIAN_POINT('Ctrl Pts',(47.7261510111862,-20.6703314910401,15.2318954195974));
#29036=CARTESIAN_POINT('Ctrl Pts',(50.8209891072403,-21.8481226187674,14.4776794959001));
#29037=CARTESIAN_POINT('Ctrl Pts',(33.871308617615,-16.7773762111447,0.));
#29038=CARTESIAN_POINT('Ctrl Pts',(33.9603261204011,-16.582455069283,3.24562220582793));
#29039=CARTESIAN_POINT('Ctrl Pts',(35.3303080462614,-16.9725307779982,6.16982677025168));
#29040=CARTESIAN_POINT('Ctrl Pts',(36.7002899721218,-17.3626064867134,9.09403133467541));
#29041=CARTESIAN_POINT('Ctrl Pts',(39.0975256070688,-18.2218132452332,11.1176436806954));
#29042=CARTESIAN_POINT('Ctrl Pts',(41.4947612420158,-19.0810200037529,13.1412560267153));
#29043=CARTESIAN_POINT('Ctrl Pts',(44.4620796765374,-20.2005748533764,13.8634749112255));
#29044=CARTESIAN_POINT('Ctrl Pts',(47.4293981110591,-21.3201297029999,14.5856937957357));
#29045=CARTESIAN_POINT('Ctrl Pts',(50.3967165455806,-22.4396845526234,13.8634749112255));
#29046=CARTESIAN_POINT('',(33.9565603202809,-15.5074469599502,1.75233474473275E-29));
#29047=CARTESIAN_POINT('Origin',(35.5938999782222,-16.2551894587643,0.));
#29048=CARTESIAN_POINT('Origin',(35.5938999782222,-16.2551894587643,0.));
#29049=CARTESIAN_POINT('Ctrl Pts',(39.242105283911,-21.1183468312851,0.));
#29050=CARTESIAN_POINT('Ctrl Pts',(39.3579568876515,-20.938078217107,1.72780310113343));
#29051=CARTESIAN_POINT('Ctrl Pts',(40.1044673847038,-21.1631094635646,3.28449990511991));
#29052=CARTESIAN_POINT('Ctrl Pts',(40.8509778817561,-21.3881407100222,4.84119670910638));
#29053=CARTESIAN_POINT('Ctrl Pts',(42.1032375437761,-21.9381972090399,5.91846432228298));
#29054=CARTESIAN_POINT('Ctrl Pts',(43.355497205796,-22.4882537080577,6.99573193545956));
#29055=CARTESIAN_POINT('Ctrl Pts',(44.8884264797112,-23.2186856141175,7.38020429521639));
#29056=CARTESIAN_POINT('Ctrl Pts',(45.6451607014122,-23.5792650807266,7.56999999999999));
#29057=CARTESIAN_POINT('Ctrl Pts',(46.4213557536264,-23.9491175201773,7.56999999999998));
#29058=CARTESIAN_POINT('Ctrl Pts',(36.873264238351,-21.0061649833188,0.));
#29059=CARTESIAN_POINT('Ctrl Pts',(36.9891158420916,-20.8258963691407,2.19648874705823));
#29060=CARTESIAN_POINT('Ctrl Pts',(37.9066995190543,-21.1608696725668,4.17545672685568));
#29061=CARTESIAN_POINT('Ctrl Pts',(38.8242831960171,-21.495842975993,6.15442470665313));
#29062=CARTESIAN_POINT('Ctrl Pts',(40.3848060765019,-22.2440082162144,7.5239130403414));
#29063=CARTESIAN_POINT('Ctrl Pts',(41.9453289569866,-22.9921734564358,8.89340137402968));
#29064=CARTESIAN_POINT('Ctrl Pts',(43.8626561769037,-23.9696429220947,9.3821661014496));
#29065=CARTESIAN_POINT('Ctrl Pts',(44.8091493688593,-24.4521730739541,9.62344598428096));
#29066=CARTESIAN_POINT('Ctrl Pts',(45.7799833968209,-24.9471123877536,9.62344598428097));
#29067=CARTESIAN_POINT('Ctrl Pts',(34.5718269932681,-20.4339943155211,0.));
#29068=CARTESIAN_POINT('Ctrl Pts',(34.6876785970087,-20.253725701343,2.70899372698069));
#29069=CARTESIAN_POINT('Ctrl Pts',(35.7923297837141,-20.7089199933768,5.14971273833323));
#29070=CARTESIAN_POINT('Ctrl Pts',(36.8969809704195,-21.1641142854106,7.59043174968577));
#29071=CARTESIAN_POINT('Ctrl Pts',(38.7945878558527,-22.12891026164,9.27946171175751));
#29072=CARTESIAN_POINT('Ctrl Pts',(40.6921947412858,-23.0937062378693,10.9684916738293));
#29073=CARTESIAN_POINT('Ctrl Pts',(43.0298588401129,-24.3413098128684,11.5712994880388));
#29074=CARTESIAN_POINT('Ctrl Pts',(44.1838523429614,-24.9571923172889,11.8688770148584));
#29075=CARTESIAN_POINT('Ctrl Pts',(45.36752293894,-25.5889133878675,11.8688770148585));
#29076=CARTESIAN_POINT('Ctrl Pts',(32.426238988581,-19.4238236466313,0.));
#29077=CARTESIAN_POINT('Ctrl Pts',(32.5420905923215,-19.2435550324532,3.24562220582792));
#29078=CARTESIAN_POINT('Ctrl Pts',(33.8426145161273,-19.8246290891125,6.16982677025168));
#29079=CARTESIAN_POINT('Ctrl Pts',(35.143138439933,-20.4057031457718,9.09403133467541));
#29080=CARTESIAN_POINT('Ctrl Pts',(37.3936958017626,-21.5973266200541,11.1176436806954));
#29081=CARTESIAN_POINT('Ctrl Pts',(39.6442531635922,-22.7889500943365,13.1412560267153));
#29082=CARTESIAN_POINT('Ctrl Pts',(42.4220393076079,-24.3194029329699,13.8634749112255));
#29083=CARTESIAN_POINT('Ctrl Pts',(43.7933001162524,-25.0749146564399,14.22));
#29084=CARTESIAN_POINT('Ctrl Pts',(45.1998254516238,-25.8498557716033,14.22));
#29085=CARTESIAN_POINT('',(32.426238988581,-19.4238236466313,0.));
#29086=CARTESIAN_POINT('Ctrl Pts',(32.426238988581,-19.4238236466313,0.));
#29087=CARTESIAN_POINT('Ctrl Pts',(32.5420905923215,-19.2435550324532,3.24562220582792));
#29088=CARTESIAN_POINT('Ctrl Pts',(33.8426145161273,-19.8246290891125,6.16982677025168));
#29089=CARTESIAN_POINT('Ctrl Pts',(34.9283413471525,-20.3097318100848,8.61106394927298));
#29090=CARTESIAN_POINT('Ctrl Pts',(36.7013364119534,-21.2335670650402,10.4489096280657));
#29091=CARTESIAN_POINT('Origin',(40.0935818932912,-3.1384973440487,0.));
#29092=CARTESIAN_POINT('Ctrl Pts',(31.1388779521426,-21.4269965203145,1.04083408558608E-14));
#29093=CARTESIAN_POINT('Ctrl Pts',(31.2547295558831,-21.2467279061364,3.24562220582792));
#29094=CARTESIAN_POINT('Ctrl Pts',(32.5552534796889,-21.8278019627957,6.16982677025168));
#29095=CARTESIAN_POINT('Ctrl Pts',(33.8557774034946,-22.4088760194551,9.09403133467541));
#29096=CARTESIAN_POINT('Ctrl Pts',(36.1063347653242,-23.6004994937374,11.1176436806954));
#29097=CARTESIAN_POINT('Ctrl Pts',(38.3568921271538,-24.7921229680197,13.1412560267153));
#29098=CARTESIAN_POINT('Ctrl Pts',(41.1346782711696,-26.3225758066531,13.8634749112255));
#29099=CARTESIAN_POINT('Ctrl Pts',(42.505939079814,-27.0780875301231,14.22));
#29100=CARTESIAN_POINT('Ctrl Pts',(43.9124644151854,-27.8530286452865,14.22));
#29101=CARTESIAN_POINT('Ctrl Pts',(32.9490709821973,-22.9590519566758,0.));
#29102=CARTESIAN_POINT('Ctrl Pts',(33.0649225859378,-22.7787833424977,2.70899372698069));
#29103=CARTESIAN_POINT('Ctrl Pts',(34.1695737726432,-23.2339776345315,5.14971273833323));
#29104=CARTESIAN_POINT('Ctrl Pts',(35.2742249593487,-23.6891719265653,7.59043174968577));
#29105=CARTESIAN_POINT('Ctrl Pts',(37.1718318447818,-24.6539679027947,9.27946171175751));
#29106=CARTESIAN_POINT('Ctrl Pts',(39.0694387302149,-25.618763879024,10.9684916738293));
#29107=CARTESIAN_POINT('Ctrl Pts',(41.407102829042,-26.8663674540231,11.5712994880388));
#29108=CARTESIAN_POINT('Ctrl Pts',(42.5610963318905,-27.4822499584436,11.8688770148584));
#29109=CARTESIAN_POINT('Ctrl Pts',(43.7447669278692,-28.1139710290222,11.8688770148585));
#29110=CARTESIAN_POINT('Ctrl Pts',(34.4255873115185,-24.8148246247013,0.));
#29111=CARTESIAN_POINT('Ctrl Pts',(34.541438915259,-24.6345560105232,2.19648874705824));
#29112=CARTESIAN_POINT('Ctrl Pts',(35.4590225922217,-24.9695293139493,4.17545672685568));
#29113=CARTESIAN_POINT('Ctrl Pts',(36.3766062691845,-25.3045026173755,6.15442470665314));
#29114=CARTESIAN_POINT('Ctrl Pts',(37.9371291496693,-26.0526678575969,7.5239130403414));
#29115=CARTESIAN_POINT('Ctrl Pts',(39.4976520301541,-26.8008330978183,8.89340137402967));
#29116=CARTESIAN_POINT('Ctrl Pts',(41.4149792500712,-27.7783025634772,9.38216610144961));
#29117=CARTESIAN_POINT('Ctrl Pts',(42.3614724420268,-28.2608327153365,9.62344598428098));
#29118=CARTESIAN_POINT('Ctrl Pts',(43.3323064699883,-28.7557720291361,9.62344598428099));
#29119=CARTESIAN_POINT('Ctrl Pts',(35.5116836434673,-26.9229962078202,0.));
#29120=CARTESIAN_POINT('Ctrl Pts',(35.6275352472078,-26.7427275936421,1.72780310113343));
#29121=CARTESIAN_POINT('Ctrl Pts',(36.3740457442601,-26.9677588400997,3.28449990511991));
#29122=CARTESIAN_POINT('Ctrl Pts',(37.1205562413124,-27.1927900865573,4.84119670910639));
#29123=CARTESIAN_POINT('Ctrl Pts',(38.3728159033324,-27.742846585575,5.91846432228298));
#29124=CARTESIAN_POINT('Ctrl Pts',(39.6250755653524,-28.2929030845928,6.99573193545956));
#29125=CARTESIAN_POINT('Ctrl Pts',(41.1580048392676,-29.0233349906526,7.38020429521641));
#29126=CARTESIAN_POINT('Ctrl Pts',(41.9147390609686,-29.3839144572617,7.57));
#29127=CARTESIAN_POINT('Ctrl Pts',(42.6909341131827,-29.7537668967124,7.57));
#29128=CARTESIAN_POINT('',(31.1388779521917,-21.4269965202912,2.36595504102218E-9));
#29129=CARTESIAN_POINT('Origin',(19.5103534449748,-35.1666259835204,1.04083408558608E-14));
#29130=CARTESIAN_POINT('Ctrl Pts',(31.1388779521426,-21.4269965203145,1.04083408558608E-14));
#29131=CARTESIAN_POINT('Ctrl Pts',(31.2547295558831,-21.2467279061364,3.24562220582792));
#29132=CARTESIAN_POINT('Ctrl Pts',(32.5552534796889,-21.8278019627957,6.16982677025168));
#29133=CARTESIAN_POINT('Ctrl Pts',(33.6474974511925,-22.3158165419709,8.62571762198519));
#29134=CARTESIAN_POINT('Ctrl Pts',(35.4345298797234,-23.2474528526984,10.4701702229062));
#29135=CARTESIAN_POINT('Ctrl Pts',(32.426238988581,-19.4238236466313,0.));
#29136=CARTESIAN_POINT('Ctrl Pts',(32.5420905923215,-19.2435550324532,3.24562220582792));
#29137=CARTESIAN_POINT('Ctrl Pts',(33.8426145161273,-19.8246290891125,6.16982677025168));
#29138=CARTESIAN_POINT('Ctrl Pts',(35.143138439933,-20.4057031457718,9.09403133467541));
#29139=CARTESIAN_POINT('Ctrl Pts',(37.3936958017626,-21.5973266200541,11.1176436806954));
#29140=CARTESIAN_POINT('Ctrl Pts',(39.6442531635922,-22.7889500943365,13.1412560267153));
#29141=CARTESIAN_POINT('Ctrl Pts',(42.4220393076079,-24.3194029329699,13.8634749112255));
#29142=CARTESIAN_POINT('Ctrl Pts',(43.7933001162524,-25.0749146564399,14.22));
#29143=CARTESIAN_POINT('Ctrl Pts',(45.1998254516238,-25.8498557716033,14.22));
#29144=CARTESIAN_POINT('Ctrl Pts',(31.5100409519659,-19.6841717937392,0.));
#29145=CARTESIAN_POINT('Ctrl Pts',(31.6258925557063,-19.5039031795611,3.38941559469373));
#29146=CARTESIAN_POINT('Ctrl Pts',(32.9789019620466,-20.1187076077132,6.44317352589574));
#29147=CARTESIAN_POINT('Ctrl Pts',(34.3319113683869,-20.7335120358653,9.49693145709774));
#29148=CARTESIAN_POINT('Ctrl Pts',(36.6770443017774,-21.9859155393833,11.6101975146502));
#29149=CARTESIAN_POINT('Ctrl Pts',(39.0221772351679,-23.2383190429012,13.7234635722027));
#29150=CARTESIAN_POINT('Ctrl Pts',(41.9178971879301,-24.8445633383047,14.4776794959001));
#29151=CARTESIAN_POINT('Ctrl Pts',(43.3473763048113,-25.6374896966353,14.85));
#29152=CARTESIAN_POINT('Ctrl Pts',(44.8136171406923,-26.4508076337082,14.85));
#29153=CARTESIAN_POINT('Ctrl Pts',(30.9950965373905,-20.4854409432125,0.));
#29154=CARTESIAN_POINT('Ctrl Pts',(31.110948141131,-20.3051723290344,3.38941559469373));
#29155=CARTESIAN_POINT('Ctrl Pts',(32.4639575474713,-20.9199767571865,6.44317352589574));
#29156=CARTESIAN_POINT('Ctrl Pts',(33.8169669538116,-21.5347811853386,9.49693145709775));
#29157=CARTESIAN_POINT('Ctrl Pts',(36.1620998872021,-22.7871846888565,11.6101975146502));
#29158=CARTESIAN_POINT('Ctrl Pts',(38.5072328205925,-24.0395881923744,13.7234635722027));
#29159=CARTESIAN_POINT('Ctrl Pts',(41.4029527733547,-25.645832487778,14.4776794959001));
#29160=CARTESIAN_POINT('Ctrl Pts',(42.8324318902359,-26.4387588461085,14.85));
#29161=CARTESIAN_POINT('Ctrl Pts',(44.2986727261169,-27.2520767831815,14.85));
#29162=CARTESIAN_POINT('Ctrl Pts',(31.1388779521426,-21.4269965203145,1.04083408558608E-14));
#29163=CARTESIAN_POINT('Ctrl Pts',(31.2547295558831,-21.2467279061364,3.24562220582792));
#29164=CARTESIAN_POINT('Ctrl Pts',(32.5552534796889,-21.8278019627957,6.16982677025168));
#29165=CARTESIAN_POINT('Ctrl Pts',(33.8557774034946,-22.4088760194551,9.09403133467541));
#29166=CARTESIAN_POINT('Ctrl Pts',(36.1063347653242,-23.6004994937374,11.1176436806954));
#29167=CARTESIAN_POINT('Ctrl Pts',(38.3568921271537,-24.7921229680197,13.1412560267153));
#29168=CARTESIAN_POINT('Ctrl Pts',(41.1346782711696,-26.3225758066531,13.8634749112255));
#29169=CARTESIAN_POINT('Ctrl Pts',(42.505939079814,-27.0780875301231,14.22));
#29170=CARTESIAN_POINT('Ctrl Pts',(43.9124644151854,-27.8530286452865,14.22));
#29171=CARTESIAN_POINT('',(31.4039916914005,-20.1821259000877,1.90249220280833E-29));
#29172=CARTESIAN_POINT('Origin',(32.9182507396839,-21.1552751870379,0.));
#29173=CARTESIAN_POINT('Origin',(32.9182507396839,-21.1552751870379,0.));
#29174=CARTESIAN_POINT('Ctrl Pts',(27.7725495286734,-25.6404249706862,0.));
#29175=CARTESIAN_POINT('Ctrl Pts',(27.9128768288045,-25.4784786333246,3.24562220582792));
#29176=CARTESIAN_POINT('Ctrl Pts',(29.1174678338683,-26.2387220458137,6.16982677025168));
#29177=CARTESIAN_POINT('Ctrl Pts',(30.3220588389321,-26.9989654583028,9.09403133467541));
#29178=CARTESIAN_POINT('Ctrl Pts',(32.3801230698288,-28.4987476307696,11.1176436806954));
#29179=CARTESIAN_POINT('Ctrl Pts',(34.4381873007256,-29.9985298032364,13.1412560267153));
#29180=CARTESIAN_POINT('Ctrl Pts',(36.9698934388172,-31.9087250245467,13.8634749112255));
#29181=CARTESIAN_POINT('Ctrl Pts',(39.5015995769088,-33.8189202458569,14.5856937957357));
#29182=CARTESIAN_POINT('Ctrl Pts',(42.0333057150004,-35.7291154671672,13.8634749112255));
#29183=CARTESIAN_POINT('Ctrl Pts',(29.3462831821134,-27.4145036200625,0.));
#29184=CARTESIAN_POINT('Ctrl Pts',(29.4866104822446,-27.2525572827009,2.70899372698069));
#29185=CARTESIAN_POINT('Ctrl Pts',(30.5152370105911,-27.8603266081622,5.14971273833323));
#29186=CARTESIAN_POINT('Ctrl Pts',(31.5438635389376,-28.4680959336234,7.59043174968578));
#29187=CARTESIAN_POINT('Ctrl Pts',(33.2848507390765,-29.6931292949424,9.27946171175751));
#29188=CARTESIAN_POINT('Ctrl Pts',(35.0258379392153,-30.9181626562613,10.9684916738293));
#29189=CARTESIAN_POINT('Ctrl Pts',(37.1621554871444,-32.4857517139246,11.5712994880388));
#29190=CARTESIAN_POINT('Ctrl Pts',(39.2984730350736,-34.0533407715878,12.1741073022483));
#29191=CARTESIAN_POINT('Ctrl Pts',(41.4347905830027,-35.6209298292511,11.5712994880388));
#29192=CARTESIAN_POINT('Ctrl Pts',(30.5436667170408,-29.461517380746,0.));
#29193=CARTESIAN_POINT('Ctrl Pts',(30.683994017172,-29.2995710433843,2.19648874705823));
#29194=CARTESIAN_POINT('Ctrl Pts',(31.5445663438467,-29.7617205741624,4.17545672685568));
#29195=CARTESIAN_POINT('Ctrl Pts',(32.4051386705215,-30.2238701049404,6.15442470665314));
#29196=CARTESIAN_POINT('Ctrl Pts',(33.8433026630073,-31.1865056631395,7.5239130403414));
#29197=CARTESIAN_POINT('Ctrl Pts',(35.2814666554931,-32.1491412213386,8.89340137402967));
#29198=CARTESIAN_POINT('Ctrl Pts',(37.0401698399467,-33.3895255704512,9.3821661014496));
#29199=CARTESIAN_POINT('Ctrl Pts',(38.7988730244003,-34.6299099195637,9.87093082886953));
#29200=CARTESIAN_POINT('Ctrl Pts',(40.5575762088539,-35.8702942686763,9.3821661014496));
#29201=CARTESIAN_POINT('Ctrl Pts',(31.3186840564481,-31.7027984407116,0.));
#29202=CARTESIAN_POINT('Ctrl Pts',(31.4590113565792,-31.54085210335,1.72780310113342));
#29203=CARTESIAN_POINT('Ctrl Pts',(32.1658981677048,-31.8698323768442,3.28449990511991));
#29204=CARTESIAN_POINT('Ctrl Pts',(32.8727849788303,-32.1988126503384,4.84119670910639));
#29205=CARTESIAN_POINT('Ctrl Pts',(34.0340172414013,-32.9214854985887,5.91846432228298));
#29206=CARTESIAN_POINT('Ctrl Pts',(35.1952495039724,-33.644158346839,6.99573193545957));
#29207=CARTESIAN_POINT('Ctrl Pts',(36.6086244696001,-34.5853140909926,7.38020429521639));
#29208=CARTESIAN_POINT('Ctrl Pts',(38.0219994352277,-35.5264698351462,7.76467665497322));
#29209=CARTESIAN_POINT('Ctrl Pts',(39.4353744008554,-36.4676255792997,7.38020429521639));
#29210=CARTESIAN_POINT('',(27.7725495286886,-25.6404249706929,1.57949994983948E-9));
#29211=CARTESIAN_POINT('Origin',(14.3070334890497,-37.5852932322719,0.));
#29212=CARTESIAN_POINT('Ctrl Pts',(27.7725495288655,-25.640424970594,3.13107432308264E-9));
#29213=CARTESIAN_POINT('Ctrl Pts',(27.783143966541,-25.6281983378207,0.245038153335697));
#29214=CARTESIAN_POINT('Ctrl Pts',(27.7986217084841,-25.6200142870522,0.490791160522144));
#29215=CARTESIAN_POINT('Ctrl Pts',(27.8190271851147,-25.6159526330982,0.736766500726005));
#29216=CARTESIAN_POINT('Ctrl Pts',(27.8393656717115,-25.611904313326,0.981934317701654));
#29217=CARTESIAN_POINT('Ctrl Pts',(27.8645996505507,-25.6119514551676,1.2273225737663));
#29218=CARTESIAN_POINT('Ctrl Pts',(27.8947338787561,-25.6161410294537,1.47243294816407));
#29219=CARTESIAN_POINT('Ctrl Pts',(27.9248227237926,-25.6203242940989,1.71717417803081));
#29220=CARTESIAN_POINT('Ctrl Pts',(27.9597970874096,-25.6286375769737,1.96163791541648));
#29221=CARTESIAN_POINT('Ctrl Pts',(27.9996219245317,-25.6410945477699,2.20532408778584));
#29222=CARTESIAN_POINT('Ctrl Pts',(28.0394126058351,-25.6535408348303,2.44880126242126));
#29223=CARTESIAN_POINT('Ctrl Pts',(28.0840454126418,-25.6701237175581,2.6915017543111));
#29224=CARTESIAN_POINT('Ctrl Pts',(28.1334457426218,-25.6908232719762,2.93292951866868));
#29225=CARTESIAN_POINT('Ctrl Pts',(28.1828357379543,-25.7115184960062,3.17430677585651));
#29226=CARTESIAN_POINT('Ctrl Pts',(28.2369911812592,-25.7363286400401,3.41441139318407));
#29227=CARTESIAN_POINT('Ctrl Pts',(28.2957987052584,-25.7652003562649,3.65275710614702));
#29228=CARTESIAN_POINT('Ctrl Pts',(28.3546809021121,-25.7941087333337,3.8914054666885));
#29229=CARTESIAN_POINT('Ctrl Pts',(28.4182268780896,-25.8270889373975,4.12829002081223));
#29230=CARTESIAN_POINT('Ctrl Pts',(28.4862854384144,-25.8640546001341,4.36293874377863));
#29231=CARTESIAN_POINT('Ctrl Pts',(28.5544134456109,-25.9010579825879,4.59782690201503));
#29232=CARTESIAN_POINT('Ctrl Pts',(28.627063077262,-25.9420548501738,4.83047425895014));
#29233=CARTESIAN_POINT('Ctrl Pts',(28.7040474659737,-25.9869270447951,5.06042975959485));
#29234=CARTESIAN_POINT('Ctrl Pts',(28.781256926861,-26.0319304281242,5.29105755998367));
#29235=CARTESIAN_POINT('Ctrl Pts',(28.8628263193251,-26.0808316886121,5.51897736305757));
#29236=CARTESIAN_POINT('Ctrl Pts',(28.9485346007075,-26.1334818341729,5.74376259354408));
#29237=CARTESIAN_POINT('Ctrl Pts',(29.0031847495425,-26.1670531325897,5.8870923407267));
#29238=CARTESIAN_POINT('Ctrl Pts',(29.0595170057056,-26.2021480259525,6.02914825314218));
#29239=CARTESIAN_POINT('Ctrl Pts',(29.1174678338914,-26.2387220458404,6.16982677023484));
#29240=CARTESIAN_POINT('Ctrl Pts',(29.2083364372323,-26.2960711849266,6.39041482339096));
#29241=CARTESIAN_POINT('Ctrl Pts',(29.3038406779896,-26.3572486158603,6.60890054011817));
#29242=CARTESIAN_POINT('Ctrl Pts',(29.4038573838823,-26.4221888209398,6.82480412008059));
#29243=CARTESIAN_POINT('Ctrl Pts',(29.5036482964477,-26.4869824198614,7.04022028559291));
#29244=CARTESIAN_POINT('Ctrl Pts',(29.6079312382237,-26.5555217851617,7.25306552029617));
#29245=CARTESIAN_POINT('Ctrl Pts',(29.7165449255433,-26.6277100364536,7.4628756626938));
#29246=CARTESIAN_POINT('Ctrl Pts',(29.8249839175523,-26.6997821794602,7.67234834441843));
#29247=CARTESIAN_POINT('Ctrl Pts',(29.9377396021004,-26.7754914030014,7.87879526532988));
#29248=CARTESIAN_POINT('Ctrl Pts',(30.0546142350027,-26.8547104088651,8.08177334612154));
#29249=CARTESIAN_POINT('Ctrl Pts',(30.1713767224891,-26.933853401242,8.28455666214074));
#29250=CARTESIAN_POINT('Ctrl Pts',(30.2922500787577,-27.0164993284348,8.48387739272822));
#29251=CARTESIAN_POINT('Ctrl Pts',(30.4170022653821,-27.1024918458757,8.67931873611067));
#29252=CARTESIAN_POINT('Ctrl Pts',(30.5417604522566,-27.1884884993291,8.87476947970451));
#29253=CARTESIAN_POINT('Ctrl Pts',(30.6703976233158,-27.2778319154182,9.06634009532774));
#29254=CARTESIAN_POINT('Ctrl Pts',(30.8026498047311,-27.3703382785461,9.25364450340917));
#29255=CARTESIAN_POINT('Ctrl Pts',(30.9349505015539,-27.4628785767203,9.44101762226418));
#29256=CARTESIAN_POINT('Ctrl Pts',(31.0708686028425,-27.558583959197,9.62412107874945));
#29257=CARTESIAN_POINT('Ctrl Pts',(31.2101115092128,-27.6572454428936,9.80260437466027));
#29258=CARTESIAN_POINT('Ctrl Pts',(31.3495815496048,-27.7560678639059,9.98137881379597));
#29259=CARTESIAN_POINT('Ctrl Pts',(31.4923869622801,-27.8578558275198,10.1555177270918));
#29260=CARTESIAN_POINT('Ctrl Pts',(31.638209399577,-27.962377242905,10.3247095747703));
#29261=CARTESIAN_POINT('Ctrl Pts',(31.6803570199419,-27.9925874699272,10.3736117457735));
#29262=CARTESIAN_POINT('Ctrl Pts',(31.7227565449007,-28.0230259217658,10.4221009095722));
#29263=CARTESIAN_POINT('Ctrl Pts',(31.7653999649232,-28.0536866918398,10.4701702229062));
#29264=CARTESIAN_POINT('Ctrl Pts',(35.8372231206706,-26.4881263776673,0.));
#29265=CARTESIAN_POINT('Ctrl Pts',(35.9775504208018,-26.3261800403057,1.72780310113343));
#29266=CARTESIAN_POINT('Ctrl Pts',(36.6844372319273,-26.6551603137999,3.28449990511991));
#29267=CARTESIAN_POINT('Ctrl Pts',(37.3913240430528,-26.9841405872941,4.84119670910638));
#29268=CARTESIAN_POINT('Ctrl Pts',(38.5525563056238,-27.7068134355444,5.91846432228298));
#29269=CARTESIAN_POINT('Ctrl Pts',(39.7137885681949,-28.4294862837947,6.99573193545956));
#29270=CARTESIAN_POINT('Ctrl Pts',(41.1271635338226,-29.3706420279483,7.38020429521639));
#29271=CARTESIAN_POINT('Ctrl Pts',(42.5405384994503,-30.3117977721018,7.76467665497322));
#29272=CARTESIAN_POINT('Ctrl Pts',(43.953913465078,-31.2529535162554,7.38020429521639));
#29273=CARTESIAN_POINT('Ctrl Pts',(33.5084586029183,-26.0399651488665,0.));
#29274=CARTESIAN_POINT('Ctrl Pts',(33.6487859030494,-25.8780188115048,2.19648874705823));
#29275=CARTESIAN_POINT('Ctrl Pts',(34.5093582297241,-26.3401683422829,4.17545672685568));
#29276=CARTESIAN_POINT('Ctrl Pts',(35.3699305563989,-26.8023178730609,6.15442470665314));
#29277=CARTESIAN_POINT('Ctrl Pts',(36.8080945488847,-27.76495343126,7.5239130403414));
#29278=CARTESIAN_POINT('Ctrl Pts',(38.2462585413705,-28.7275889894591,8.89340137402967));
#29279=CARTESIAN_POINT('Ctrl Pts',(40.0049617258241,-29.9679733385717,9.3821661014496));
#29280=CARTESIAN_POINT('Ctrl Pts',(41.7636649102777,-31.2083576876842,9.87093082886953));
#29281=CARTESIAN_POINT('Ctrl Pts',(43.5223680947313,-32.4487420367968,9.3821661014496));
#29282=CARTESIAN_POINT('Ctrl Pts',(31.3118750466442,-25.1460896841349,0.));
#29283=CARTESIAN_POINT('Ctrl Pts',(31.4522023467754,-24.9841433467732,2.70899372698069));
#29284=CARTESIAN_POINT('Ctrl Pts',(32.4808288751219,-25.5919126722345,5.14971273833323));
#29285=CARTESIAN_POINT('Ctrl Pts',(33.5094554034684,-26.1996819976958,7.59043174968578));
#29286=CARTESIAN_POINT('Ctrl Pts',(35.2504426036073,-27.4247153590147,9.27946171175752));
#29287=CARTESIAN_POINT('Ctrl Pts',(36.9914298037461,-28.6497487203337,10.9684916738293));
#29288=CARTESIAN_POINT('Ctrl Pts',(39.1277473516752,-30.2173377779969,11.5712994880388));
#29289=CARTESIAN_POINT('Ctrl Pts',(41.2640648996044,-31.7849268356602,12.1741073022483));
#29290=CARTESIAN_POINT('Ctrl Pts',(43.4003824475335,-33.3525158933234,11.5712994880388));
#29291=CARTESIAN_POINT('Ctrl Pts',(29.3318883095338,-23.8408520862203,0.));
#29292=CARTESIAN_POINT('Ctrl Pts',(29.4722156096649,-23.6789057488587,3.24562220582793));
#29293=CARTESIAN_POINT('Ctrl Pts',(30.6768066147287,-24.4391491613478,6.16982677025167));
#29294=CARTESIAN_POINT('Ctrl Pts',(31.8813976197925,-25.1993925738369,9.09403133467541));
#29295=CARTESIAN_POINT('Ctrl Pts',(33.9394618506893,-26.6991747463037,11.1176436806954));
#29296=CARTESIAN_POINT('Ctrl Pts',(35.997526081586,-28.1989569187706,13.1412560267153));
#29297=CARTESIAN_POINT('Ctrl Pts',(38.5292322196776,-30.1091521400808,13.8634749112255));
#29298=CARTESIAN_POINT('Ctrl Pts',(41.0609383577692,-32.0193473613911,14.5856937957357));
#29299=CARTESIAN_POINT('Ctrl Pts',(43.5926444958608,-33.9295425827013,13.8634749112255));
#29300=CARTESIAN_POINT('',(29.3318883095338,-23.8408520862203,0.));
#29301=CARTESIAN_POINT('Ctrl Pts',(29.3318883095338,-23.8408520862203,0.));
#29302=CARTESIAN_POINT('Ctrl Pts',(29.472215609665,-23.6789057488587,3.24562220582793));
#29303=CARTESIAN_POINT('Ctrl Pts',(30.6768066147287,-24.4391491613478,6.16982677025167));
#29304=CARTESIAN_POINT('Ctrl Pts',(31.6824449968205,-25.0738292744465,8.61106394926976));
#29305=CARTESIAN_POINT('Ctrl Pts',(33.3059180634108,-26.2405847244742,10.4489096280657));
#29306=CARTESIAN_POINT('Origin',(39.2388322978494,-8.81246358936616,0.));
#29307=CARTESIAN_POINT('Ctrl Pts',(29.3318883095338,-23.8408520862204,0.));
#29308=CARTESIAN_POINT('Ctrl Pts',(29.472215609665,-23.6789057488587,3.24562220582793));
#29309=CARTESIAN_POINT('Ctrl Pts',(30.6768066147287,-24.4391491613478,6.16982677025167));
#29310=CARTESIAN_POINT('Ctrl Pts',(31.8813976197925,-25.1993925738369,9.09403133467541));
#29311=CARTESIAN_POINT('Ctrl Pts',(33.9394618506893,-26.6991747463037,11.1176436806954));
#29312=CARTESIAN_POINT('Ctrl Pts',(35.997526081586,-28.1989569187706,13.1412560267153));
#29313=CARTESIAN_POINT('Ctrl Pts',(38.5292322196776,-30.1091521400808,13.8634749112255));
#29314=CARTESIAN_POINT('Ctrl Pts',(41.0609383577692,-32.0193473613911,14.5856937957357));
#29315=CARTESIAN_POINT('Ctrl Pts',(43.5926444958608,-33.9295425827013,13.8634749112255));
#29316=CARTESIAN_POINT('Ctrl Pts',(28.3879644434325,-23.9681616891746,0.));
#29317=CARTESIAN_POINT('Ctrl Pts',(28.5282917435636,-23.8062153518129,3.38941559469372));
#29318=CARTESIAN_POINT('Ctrl Pts',(29.7800336722637,-24.6073152722068,6.44317352589573));
#29319=CARTESIAN_POINT('Ctrl Pts',(31.0317756009638,-25.4084151926007,9.49693145709773));
#29320=CARTESIAN_POINT('Ctrl Pts',(33.1748028604387,-26.9818182484143,11.6101975146502));
#29321=CARTESIAN_POINT('Ctrl Pts',(35.3178301199137,-28.555221304228,13.7234635722027));
#29322=CARTESIAN_POINT('Ctrl Pts',(37.9554834217124,-30.5572202654794,14.4776794959001));
#29323=CARTESIAN_POINT('Ctrl Pts',(40.5931367235111,-32.5592192267308,15.2318954195974));
#29324=CARTESIAN_POINT('Ctrl Pts',(43.2307900253098,-34.5612181879822,14.4776794959001));
#29325=CARTESIAN_POINT('Ctrl Pts',(27.7642289310883,-24.6879908429609,0.));
#29326=CARTESIAN_POINT('Ctrl Pts',(27.9045562312195,-24.5260445055993,3.38941559469372));
#29327=CARTESIAN_POINT('Ctrl Pts',(29.1562981599195,-25.3271444259932,6.44317352589573));
#29328=CARTESIAN_POINT('Ctrl Pts',(30.4080400886196,-26.128244346387,9.49693145709774));
#29329=CARTESIAN_POINT('Ctrl Pts',(32.5510673480945,-27.7016474022007,11.6101975146502));
#29330=CARTESIAN_POINT('Ctrl Pts',(34.6940946075695,-29.2750504580143,13.7234635722027));
#29331=CARTESIAN_POINT('Ctrl Pts',(37.3317479093682,-31.2770494192658,14.4776794959001));
#29332=CARTESIAN_POINT('Ctrl Pts',(39.9694012111669,-33.2790483805172,15.2318954195974));
#29333=CARTESIAN_POINT('Ctrl Pts',(42.6070545129656,-35.2810473417686,14.4776794959001));
#29334=CARTESIAN_POINT('Ctrl Pts',(27.7725495286734,-25.6404249706862,0.));
#29335=CARTESIAN_POINT('Ctrl Pts',(27.9128768288045,-25.4784786333246,3.24562220582792));
#29336=CARTESIAN_POINT('Ctrl Pts',(29.1174678338683,-26.2387220458137,6.16982677025167));
#29337=CARTESIAN_POINT('Ctrl Pts',(30.3220588389321,-26.9989654583028,9.09403133467541));
#29338=CARTESIAN_POINT('Ctrl Pts',(32.3801230698288,-28.4987476307696,11.1176436806954));
#29339=CARTESIAN_POINT('Ctrl Pts',(34.4381873007256,-29.9985298032364,13.1412560267153));
#29340=CARTESIAN_POINT('Ctrl Pts',(36.9698934388172,-31.9087250245467,13.8634749112255));
#29341=CARTESIAN_POINT('Ctrl Pts',(39.5015995769088,-33.8189202458569,14.5856937957357));
#29342=CARTESIAN_POINT('Ctrl Pts',(42.0333057150004,-35.7291154671672,13.8634749112255));
#29343=CARTESIAN_POINT('',(28.2121283533189,-24.4459549573422,1.89568229885369E-29));
#29344=CARTESIAN_POINT('Origin',(29.5724808444819,-25.6247005192794,0.));
#29345=CARTESIAN_POINT('Origin',(29.5724808444819,-25.6247005192794,0.));
#29346=CARTESIAN_POINT('Ctrl Pts',(23.8408520862196,-29.3318883095344,0.));
#29347=CARTESIAN_POINT('Ctrl Pts',(24.0027984235812,-29.1915610094033,3.24562220582793));
#29348=CARTESIAN_POINT('Ctrl Pts',(25.0869345107936,-30.1154974142048,6.16982677025167));
#29349=CARTESIAN_POINT('Ctrl Pts',(26.1710705980059,-31.0394338190064,9.09403133467541));
#29350=CARTESIAN_POINT('Ctrl Pts',(27.9947454451959,-32.8168434496409,11.1176436806954));
#29351=CARTESIAN_POINT('Ctrl Pts',(29.8184202923859,-34.5942530802755,13.1412560267153));
#29352=CARTESIAN_POINT('Ctrl Pts',(32.0525081884194,-36.8453046181048,13.8634749112255));
#29353=CARTESIAN_POINT('Ctrl Pts',(34.2865960844529,-39.0963561559342,14.5856937957357));
#29354=CARTESIAN_POINT('Ctrl Pts',(36.5206839804863,-41.3474076937636,13.8634749112255));
#29355=CARTESIAN_POINT('Ctrl Pts',(25.1460896841341,-31.3118750466448,0.));
#29356=CARTESIAN_POINT('Ctrl Pts',(25.3080360214957,-31.1715477465137,2.70899372698069));
#29357=CARTESIAN_POINT('Ctrl Pts',(26.2396980216802,-31.919519674598,5.14971273833323));
#29358=CARTESIAN_POINT('Ctrl Pts',(27.1713600218647,-32.6674916026823,7.59043174968577));
#29359=CARTESIAN_POINT('Ctrl Pts',(28.7202860579068,-34.1278242025589,9.27946171175751));
#29360=CARTESIAN_POINT('Ctrl Pts',(30.269212093949,-35.5881568024355,10.9684916738293));
#29361=CARTESIAN_POINT('Ctrl Pts',(32.1606938263354,-37.4438197501024,11.5712994880388));
#29362=CARTESIAN_POINT('Ctrl Pts',(34.0521755587219,-39.2994826977694,12.1741073022483));
#29363=CARTESIAN_POINT('Ctrl Pts',(35.9436572911084,-41.1551456454363,11.5712994880388));
#29364=CARTESIAN_POINT('Ctrl Pts',(26.0399651488656,-33.5084586029189,0.));
#29365=CARTESIAN_POINT('Ctrl Pts',(26.2019114862272,-33.3681313027878,2.19648874705823));
#29366=CARTESIAN_POINT('Ctrl Pts',(26.9879536917285,-33.9480490292003,4.17545672685567));
#29367=CARTESIAN_POINT('Ctrl Pts',(27.7739958972298,-34.5279667556128,6.15442470665314));
#29368=CARTESIAN_POINT('Ctrl Pts',(29.0605241301521,-35.6854761478364,7.5239130403414));
#29369=CARTESIAN_POINT('Ctrl Pts',(30.3470523630745,-36.84298554006,8.89340137402967));
#29370=CARTESIAN_POINT('Ctrl Pts',(31.9113293869102,-38.3210341242513,9.3821661014496));
#29371=CARTESIAN_POINT('Ctrl Pts',(33.475606410746,-39.7990827084427,9.87093082886954));
#29372=CARTESIAN_POINT('Ctrl Pts',(35.0398834345817,-41.277131292634,9.3821661014496));
#29373=CARTESIAN_POINT('Ctrl Pts',(26.4881263776664,-35.8372231206713,0.));
#29374=CARTESIAN_POINT('Ctrl Pts',(26.650072715028,-35.6968958205402,1.72780310113342));
#29375=CARTESIAN_POINT('Ctrl Pts',(27.3029456632455,-36.1231280314035,3.28449990511991));
#29376=CARTESIAN_POINT('Ctrl Pts',(27.955818611463,-36.5493602422667,4.84119670910638));
#29377=CARTESIAN_POINT('Ctrl Pts',(29.0023841344365,-37.4299379045755,5.91846432228297));
#29378=CARTESIAN_POINT('Ctrl Pts',(30.0489496574099,-38.3105155668843,6.99573193545956));
#29379=CARTESIAN_POINT('Ctrl Pts',(31.3139980762868,-39.4432359322498,7.38020429521639));
#29380=CARTESIAN_POINT('Ctrl Pts',(32.5790464951636,-40.5759562976152,7.76467665497321));
#29381=CARTESIAN_POINT('Ctrl Pts',(33.8440949140404,-41.7086766629806,7.38020429521638));
#29382=CARTESIAN_POINT('',(23.8408520862337,-29.3318883095433,1.57949914646235E-9));
#29383=CARTESIAN_POINT('Origin',(8.81246358936518,-39.2388322978496,0.));
#29384=CARTESIAN_POINT('Ctrl Pts',(23.8408520864229,-29.3318883094705,3.13107447079983E-9));
#29385=CARTESIAN_POINT('Ctrl Pts',(23.8530787192645,-29.3212938718739,0.245038153335542));
#29386=CARTESIAN_POINT('Ctrl Pts',(23.8695636319732,-29.3153958352833,0.490791160521833));
#29387=CARTESIAN_POINT('Ctrl Pts',(23.8903394438996,-29.3142795252166,0.736766500725538));
#29388=CARTESIAN_POINT('Ctrl Pts',(23.9110470500022,-29.3131668799333,0.98193431770121));
#29389=CARTESIAN_POINT('Ctrl Pts',(23.9360174743375,-29.3168047115564,1.22732257376588));
#29390=CARTESIAN_POINT('Ctrl Pts',(23.9652487409628,-29.3252401898307,1.47243294816367));
#29391=CARTESIAN_POINT('Ctrl Pts',(23.9944359843099,-29.3336629639887,1.71717417803045));
#29392=CARTESIAN_POINT('Ctrl Pts',(24.0278712558264,-29.3468690005325,1.96163791541615));
#29393=CARTESIAN_POINT('Ctrl Pts',(24.065517921745,-29.3648668425817,2.20532408778555));
#29394=CARTESIAN_POINT('Ctrl Pts',(24.1031322999561,-29.3828492487604,2.44880126242098));
#29395=CARTESIAN_POINT('Ctrl Pts',(24.1449508188711,-29.405615252335,2.69150175431084));
#29396=CARTESIAN_POINT('Ctrl Pts',(24.190902470982,-29.4331345151071,2.93292951866843));
#29397=CARTESIAN_POINT('Ctrl Pts',(24.2368445099157,-29.4606480207946,3.1743067758563));
#29398=CARTESIAN_POINT('Ctrl Pts',(24.2869178772577,-29.4929127564911,3.41441139318389));
#29399=CARTESIAN_POINT('Ctrl Pts',(24.3410179518308,-29.5298597835415,3.65275710614686));
#29400=CARTESIAN_POINT('Ctrl Pts',(24.3951867218144,-29.5668537253366,3.8914054666884));
#29401=CARTESIAN_POINT('Ctrl Pts',(24.4533923189747,-29.6085417737707,4.12829002081218));
#29402=CARTESIAN_POINT('Ctrl Pts',(24.5154973789737,-29.6548169223665,4.36293874377864));
#29403=CARTESIAN_POINT('Ctrl Pts',(24.5776658108999,-29.7011392900673,4.59782690201484));
#29404=CARTESIAN_POINT('Ctrl Pts',(24.6437415114726,-29.7520579892328,4.83047425894975));
#29405=CARTESIAN_POINT('Ctrl Pts',(24.713556330989,-29.8074294704423,5.06042975959428));
#29406=CARTESIAN_POINT('Ctrl Pts',(24.7835752616711,-29.8629628361579,5.29105755998308));
#29407=CARTESIAN_POINT('Ctrl Pts',(24.8573550203555,-29.9229748872205,5.51897736305697));
#29408=CARTESIAN_POINT('Ctrl Pts',(24.934698018064,-29.9872866904183,5.74376259354346));
#29409=CARTESIAN_POINT('Ctrl Pts',(24.9840142132782,-30.0282938085162,5.88709234072629));
#29410=CARTESIAN_POINT('Ctrl Pts',(25.0347785642248,-30.0710484023926,6.02914825314197));
#29411=CARTESIAN_POINT('Ctrl Pts',(25.0869345108126,-30.1154974142346,6.16982677023484));
#29412=CARTESIAN_POINT('Ctrl Pts',(25.1687165693391,-30.1851947723641,6.39041482339095));
#29413=CARTESIAN_POINT('Ctrl Pts',(25.2545422584419,-30.2593411758393,6.60890054011814));
#29414=CARTESIAN_POINT('Ctrl Pts',(25.3442989836975,-30.3378542445908,6.82480412008055));
#29415=CARTESIAN_POINT('Ctrl Pts',(25.4338530781079,-30.4161900656829,7.04022028559292));
#29416=CARTESIAN_POINT('Ctrl Pts',(25.5273204012121,-30.4988728090636,7.25306552029623));
#29417=CARTESIAN_POINT('Ctrl Pts',(25.6245550984951,-30.5857836273894,7.4628756626939));
#29418=CARTESIAN_POINT('Ctrl Pts',(25.7216334025455,-30.67255465751,7.67234834441854));
#29419=CARTESIAN_POINT('Ctrl Pts',(25.8224668509011,-30.76354007733,7.87879526533001));
#29420=CARTESIAN_POINT('Ctrl Pts',(25.9268778285521,-30.8585857424181,8.08177334612168));
#29421=CARTESIAN_POINT('Ctrl Pts',(26.031188620113,-30.9535402077705,8.28455666214093));
#29422=CARTESIAN_POINT('Ctrl Pts',(26.1390699181374,-31.052546990739,8.48387739272847));
#29423=CARTESIAN_POINT('Ctrl Pts',(26.2503142961675,-31.155418315607,8.67931873611097));
#29424=CARTESIAN_POINT('Ctrl Pts',(26.3615640247578,-31.2582945883135,8.87476947970483));
#29425=CARTESIAN_POINT('Ctrl Pts',(26.4761769610836,-31.3650355954447,9.06634009532807));
#29426=CARTESIAN_POINT('Ctrl Pts',(26.5939179778762,-31.4754218249885,9.2536445034095));
#29427=CARTESIAN_POINT('Ctrl Pts',(26.711702186799,-31.5858485486314,9.44101762226479));
#29428=CARTESIAN_POINT('Ctrl Pts',(26.8326165417653,-31.6999229509137,9.62412107875033));
#29429=CARTESIAN_POINT('Ctrl Pts',(26.9564011630246,-31.8173965346654,9.8026043746614));
#29430=CARTESIAN_POINT('Ctrl Pts',(27.0803877026405,-31.9350617421642,9.98137881379707));
#29431=CARTESIAN_POINT('Ctrl Pts',(27.2072536245433,-32.0561369802841,10.1555177270928));
#29432=CARTESIAN_POINT('Ctrl Pts',(27.3367168513604,-32.1803472149487,10.3247095747713));
#29433=CARTESIAN_POINT('Ctrl Pts',(27.3741361061487,-32.2162481771949,10.3736117457742));
#29434=CARTESIAN_POINT('Ctrl Pts',(27.4117722217276,-32.2524108910196,10.4221009095725));
#29435=CARTESIAN_POINT('Ctrl Pts',(27.4496181106863,-32.288828370087,10.4701702229062));
#29436=CARTESIAN_POINT('Ctrl Pts',(31.7027984407109,-31.3186840564489,1.04083408558608E-14));
#29437=CARTESIAN_POINT('Ctrl Pts',(31.8647447780725,-31.1783567563178,1.72780310113343));
#29438=CARTESIAN_POINT('Ctrl Pts',(32.5176177262899,-31.604588967181,3.28449990511991));
#29439=CARTESIAN_POINT('Ctrl Pts',(33.1704906745074,-32.0308211780443,4.84119670910639));
#29440=CARTESIAN_POINT('Ctrl Pts',(34.2170561974809,-32.9113988403531,5.91846432228298));
#29441=CARTESIAN_POINT('Ctrl Pts',(35.2636217204544,-33.791976502662,6.99573193545957));
#29442=CARTESIAN_POINT('Ctrl Pts',(36.5286701393312,-34.9246968680274,7.3802042952164));
#29443=CARTESIAN_POINT('Ctrl Pts',(37.793718558208,-36.0574172333928,7.76467665497322));
#29444=CARTESIAN_POINT('Ctrl Pts',(39.0587669770848,-37.1901375987582,7.38020429521639));
#29445=CARTESIAN_POINT('Ctrl Pts',(29.4615173807452,-30.5436667170416,0.));
#29446=CARTESIAN_POINT('Ctrl Pts',(29.6234637181068,-30.4033394169105,2.19648874705823));
#29447=CARTESIAN_POINT('Ctrl Pts',(30.4095059236081,-30.983257143323,4.17545672685568));
#29448=CARTESIAN_POINT('Ctrl Pts',(31.1955481291094,-31.5631748697354,6.15442470665313));
#29449=CARTESIAN_POINT('Ctrl Pts',(32.4820763620317,-32.720684261959,7.5239130403414));
#29450=CARTESIAN_POINT('Ctrl Pts',(33.7686045949541,-33.8781936541826,8.89340137402968));
#29451=CARTESIAN_POINT('Ctrl Pts',(35.3328816187898,-35.356242238374,9.3821661014496));
#29452=CARTESIAN_POINT('Ctrl Pts',(36.8971586426256,-36.8342908225653,9.87093082886953));
#29453=CARTESIAN_POINT('Ctrl Pts',(38.4614356664613,-38.3123394067567,9.3821661014496));
#29454=CARTESIAN_POINT('Ctrl Pts',(27.4145036200618,-29.3462831821141,-1.05434036998093E-14));
#29455=CARTESIAN_POINT('Ctrl Pts',(27.5764499574234,-29.205955881983,2.7089937269807));
#29456=CARTESIAN_POINT('Ctrl Pts',(28.5081119576079,-29.9539278100673,5.14971273833323));
#29457=CARTESIAN_POINT('Ctrl Pts',(29.4397739577924,-30.7018997381516,7.59043174968578));
#29458=CARTESIAN_POINT('Ctrl Pts',(30.9886999938346,-32.1622323380282,9.27946171175751));
#29459=CARTESIAN_POINT('Ctrl Pts',(32.5376260298767,-33.6225649379048,10.9684916738293));
#29460=CARTESIAN_POINT('Ctrl Pts',(34.4291077622632,-35.4782278855717,11.5712994880388));
#29461=CARTESIAN_POINT('Ctrl Pts',(36.3205894946496,-37.3338908332386,12.1741073022483));
#29462=CARTESIAN_POINT('Ctrl Pts',(38.2120712270361,-39.1895537809055,11.5712994880388));
#29463=CARTESIAN_POINT('Ctrl Pts',(25.6404249706855,-27.772549528674,0.));
#29464=CARTESIAN_POINT('Ctrl Pts',(25.8023713080471,-27.6322222285429,3.24562220582793));
#29465=CARTESIAN_POINT('Ctrl Pts',(26.8865073952594,-28.5561586333444,6.16982677025167));
#29466=CARTESIAN_POINT('Ctrl Pts',(27.9706434824718,-29.480095038146,9.09403133467541));
#29467=CARTESIAN_POINT('Ctrl Pts',(29.7943183296618,-31.2575046687805,11.1176436806954));
#29468=CARTESIAN_POINT('Ctrl Pts',(31.6179931768518,-33.034914299415,13.1412560267153));
#29469=CARTESIAN_POINT('Ctrl Pts',(33.8520810728853,-35.2859658372444,13.8634749112255));
#29470=CARTESIAN_POINT('Ctrl Pts',(36.0861689689187,-37.5370173750738,14.5856937957357));
#29471=CARTESIAN_POINT('Ctrl Pts',(38.3202568649522,-39.7880689129032,13.8634749112255));
#29472=CARTESIAN_POINT('',(25.6404249706855,-27.772549528674,0.));
#29473=CARTESIAN_POINT('Ctrl Pts',(25.6404249706855,-27.772549528674,0.));
#29474=CARTESIAN_POINT('Ctrl Pts',(25.8023713080471,-27.6322222285429,3.24562220582793));
#29475=CARTESIAN_POINT('Ctrl Pts',(26.8865073952594,-28.5561586333444,6.16982677025168));
#29476=CARTESIAN_POINT('Ctrl Pts',(27.7915854309814,-29.3274958817337,8.61106394926977));
#29477=CARTESIAN_POINT('Ctrl Pts',(29.2324872694335,-30.7134197505154,10.4489096280657));
#29478=CARTESIAN_POINT('Origin',(37.5852932322715,-14.3070334890506,0.));
#29479=CARTESIAN_POINT('Ctrl Pts',(25.6404249706855,-27.772549528674,0.));
#29480=CARTESIAN_POINT('Ctrl Pts',(25.8023713080471,-27.6322222285429,3.24562220582793));
#29481=CARTESIAN_POINT('Ctrl Pts',(26.8865073952594,-28.5561586333444,6.16982677025168));
#29482=CARTESIAN_POINT('Ctrl Pts',(27.9706434824718,-29.480095038146,9.09403133467541));
#29483=CARTESIAN_POINT('Ctrl Pts',(29.7943183296618,-31.2575046687805,11.1176436806954));
#29484=CARTESIAN_POINT('Ctrl Pts',(31.6179931768518,-33.0349142994151,13.1412560267153));
#29485=CARTESIAN_POINT('Ctrl Pts',(33.8520810728853,-35.2859658372444,13.8634749112255));
#29486=CARTESIAN_POINT('Ctrl Pts',(36.0861689689187,-37.5370173750738,14.5856937957357));
#29487=CARTESIAN_POINT('Ctrl Pts',(38.3202568649522,-39.7880689129032,13.8634749112255));
#29488=CARTESIAN_POINT('Ctrl Pts',(24.6879908429602,-27.764228931089,6.24500451351652E-15));
#29489=CARTESIAN_POINT('Ctrl Pts',(24.8499371803218,-27.6239016309578,3.38941559469372));
#29490=CARTESIAN_POINT('Ctrl Pts',(25.9749297754389,-28.5949889593956,6.44317352589574));
#29491=CARTESIAN_POINT('Ctrl Pts',(27.0999223705561,-29.5660762878334,9.49693145709774));
#29492=CARTESIAN_POINT('Ctrl Pts',(28.9972181010929,-31.4284489470462,11.6101975146502));
#29493=CARTESIAN_POINT('Ctrl Pts',(30.8945138316298,-33.2908216062589,13.7234635722027));
#29494=CARTESIAN_POINT('Ctrl Pts',(33.2204054676043,-35.6478203077954,14.4776794959001));
#29495=CARTESIAN_POINT('Ctrl Pts',(35.5462971035789,-38.0048190093319,15.2318954195974));
#29496=CARTESIAN_POINT('Ctrl Pts',(37.8721887395536,-40.3618177108684,14.4776794959001));
#29497=CARTESIAN_POINT('Ctrl Pts',(23.9681616891738,-28.3879644434331,0.));
#29498=CARTESIAN_POINT('Ctrl Pts',(24.1301080265355,-28.247637143302,3.38941559469374));
#29499=CARTESIAN_POINT('Ctrl Pts',(25.2551006216526,-29.2187244717398,6.44317352589574));
#29500=CARTESIAN_POINT('Ctrl Pts',(26.3800932167697,-30.1898118001776,9.49693145709774));
#29501=CARTESIAN_POINT('Ctrl Pts',(28.2773889473065,-32.0521844593903,11.6101975146502));
#29502=CARTESIAN_POINT('Ctrl Pts',(30.1746846778434,-33.9145571186031,13.7234635722027));
#29503=CARTESIAN_POINT('Ctrl Pts',(32.500576313818,-36.2715558201396,14.4776794959001));
#29504=CARTESIAN_POINT('Ctrl Pts',(34.8264679497926,-38.6285545216761,15.2318954195974));
#29505=CARTESIAN_POINT('Ctrl Pts',(37.1523595857672,-40.9855532232126,14.4776794959001));
#29506=CARTESIAN_POINT('Ctrl Pts',(23.8408520862196,-29.3318883095344,0.));
#29507=CARTESIAN_POINT('Ctrl Pts',(24.0027984235812,-29.1915610094033,3.24562220582793));
#29508=CARTESIAN_POINT('Ctrl Pts',(25.0869345107935,-30.1154974142048,6.16982677025168));
#29509=CARTESIAN_POINT('Ctrl Pts',(26.1710705980059,-31.0394338190064,9.09403133467541));
#29510=CARTESIAN_POINT('Ctrl Pts',(27.9947454451959,-32.8168434496409,11.1176436806954));
#29511=CARTESIAN_POINT('Ctrl Pts',(29.8184202923859,-34.5942530802755,13.1412560267153));
#29512=CARTESIAN_POINT('Ctrl Pts',(32.0525081884194,-36.8453046181048,13.8634749112255));
#29513=CARTESIAN_POINT('Ctrl Pts',(34.2865960844529,-39.0963561559342,14.5856937957357));
#29514=CARTESIAN_POINT('Ctrl Pts',(36.5206839804863,-41.3474076937636,13.8634749112255));
#29515=CARTESIAN_POINT('',(24.4459474390596,-28.2121348679478,1.9100087581672E-29));
#29516=CARTESIAN_POINT('Origin',(25.6247005192787,-29.5724808444825,0.));
#29517=CARTESIAN_POINT('Origin',(25.6247005192787,-29.5724808444825,0.));
#29518=CARTESIAN_POINT('Ctrl Pts',(19.4238236466305,-32.4262389885815,0.));
#29519=CARTESIAN_POINT('Ctrl Pts',(19.6040922608086,-32.3103873848411,3.24562220582793));
#29520=CARTESIAN_POINT('Ctrl Pts',(20.5457035458241,-33.3792081011658,6.16982677025167));
#29521=CARTESIAN_POINT('Ctrl Pts',(21.4873148308396,-34.4480288174907,9.09403133467541));
#29522=CARTESIAN_POINT('Ctrl Pts',(23.0394755334781,-36.4668829718393,11.1176436806954));
#29523=CARTESIAN_POINT('Ctrl Pts',(24.5916362361166,-38.4857371261879,13.1412560267153));
#29524=CARTESIAN_POINT('Ctrl Pts',(26.4826263031061,-41.0318200627228,13.8634749112255));
#29525=CARTESIAN_POINT('Ctrl Pts',(28.3736163700957,-43.5779029992577,14.5856937957357));
#29526=CARTESIAN_POINT('Ctrl Pts',(30.2646064370852,-46.1239859357925,13.8634749112255));
#29527=CARTESIAN_POINT('Ctrl Pts',(20.4339943155202,-34.5718269932687,-1.05434036998093E-14));
#29528=CARTESIAN_POINT('Ctrl Pts',(20.6142629296984,-34.4559753895282,2.7089937269807));
#29529=CARTESIAN_POINT('Ctrl Pts',(21.4299944500884,-35.3289233687527,5.14971273833323));
#29530=CARTESIAN_POINT('Ctrl Pts',(22.2457259704784,-36.2018713479772,7.59043174968578));
#29531=CARTESIAN_POINT('Ctrl Pts',(23.5710591750639,-37.8677750259294,9.27946171175752));
#29532=CARTESIAN_POINT('Ctrl Pts',(24.8963923796494,-39.5336787038816,10.9684916738293));
#29533=CARTESIAN_POINT('Ctrl Pts',(26.5045331830047,-41.6396395952277,11.5712994880388));
#29534=CARTESIAN_POINT('Ctrl Pts',(28.1126739863599,-43.7456004865739,12.1741073022483));
#29535=CARTESIAN_POINT('Ctrl Pts',(29.7208147897152,-45.8515613779201,11.5712994880388));
#29536=CARTESIAN_POINT('Ctrl Pts',(21.0061649833179,-36.8732642383516,-1.05434036998093E-14));
#29537=CARTESIAN_POINT('Ctrl Pts',(21.186433597496,-36.7574126346111,2.19648874705824));
#29538=CARTESIAN_POINT('Ctrl Pts',(21.8819441292783,-37.4432931040929,4.17545672685568));
#29539=CARTESIAN_POINT('Ctrl Pts',(22.5774546610607,-38.1291735735747,6.15442470665314));
#29540=CARTESIAN_POINT('Ctrl Pts',(23.6861571296383,-39.4579932465786,7.5239130403414));
#29541=CARTESIAN_POINT('Ctrl Pts',(24.7948595982159,-40.7868129195824,8.89340137402968));
#29542=CARTESIAN_POINT('Ctrl Pts',(26.1328662922309,-42.4724369320186,9.38216610144961));
#29543=CARTESIAN_POINT('Ctrl Pts',(27.470872986246,-44.1580609444547,9.87093082886954));
#29544=CARTESIAN_POINT('Ctrl Pts',(28.8088796802611,-45.8436849568909,9.3821661014496));
#29545=CARTESIAN_POINT('Ctrl Pts',(21.1183468312841,-39.2421052839115,0.));
#29546=CARTESIAN_POINT('Ctrl Pts',(21.2986154454622,-39.1262536801711,1.72780310113343));
#29547=CARTESIAN_POINT('Ctrl Pts',(21.884183920276,-39.6410609697424,3.28449990511991));
#29548=CARTESIAN_POINT('Ctrl Pts',(22.4697523950898,-40.1558682593138,4.84119670910639));
#29549=CARTESIAN_POINT('Ctrl Pts',(23.3803461224637,-41.1764247138528,5.91846432228298));
#29550=CARTESIAN_POINT('Ctrl Pts',(24.2909398498377,-42.1969811683918,6.99573193545956));
#29551=CARTESIAN_POINT('Ctrl Pts',(25.3819089842537,-43.4982072348261,7.38020429521639));
#29552=CARTESIAN_POINT('Ctrl Pts',(26.4728781186697,-44.7994333012603,7.76467665497321));
#29553=CARTESIAN_POINT('Ctrl Pts',(27.5638472530857,-46.1006593676945,7.38020429521639));
#29554=CARTESIAN_POINT('',(19.4238236466412,-32.4262389886037,1.57949788822268E-9));
#29555=CARTESIAN_POINT('Origin',(3.1384973440476,-40.0935818932913,0.));
#29556=CARTESIAN_POINT('Ctrl Pts',(19.4238236468408,-32.4262389885472,3.13107065661919E-9));
#29557=CARTESIAN_POINT('Ctrl Pts',(19.4374335758626,-32.4174924183249,0.245038153335379));
#29558=CARTESIAN_POINT('Ctrl Pts',(19.4545900740527,-32.4140004629286,0.490791160521511));
#29559=CARTESIAN_POINT('Ctrl Pts',(19.4753132856565,-32.4158522216031,0.736766500725056));
#29560=CARTESIAN_POINT('Ctrl Pts',(19.4959684641204,-32.4176979010579,0.981934317700683));
#29561=CARTESIAN_POINT('Ctrl Pts',(19.5201670081213,-32.4248523667014,1.22732257376531));
#29562=CARTESIAN_POINT('Ctrl Pts',(19.547900248874,-32.437362026952,1.47243294816306));
#29563=CARTESIAN_POINT('Ctrl Pts',(19.5755917224262,-32.4498528472304,1.71717417802983));
#29564=CARTESIAN_POINT('Ctrl Pts',(19.6068072561333,-32.4676828006221,1.96163791541552));
#29565=CARTESIAN_POINT('Ctrl Pts',(19.6415093732944,-32.4908551297618,2.20532408778492));
#29566=CARTESIAN_POINT('Ctrl Pts',(19.6761817281436,-32.5140075851259,2.44880126242038));
#29567=CARTESIAN_POINT('Ctrl Pts',(19.7143346547166,-32.5424932593662,2.69150175431026));
#29568=CARTESIAN_POINT('Ctrl Pts',(19.755902185835,-32.5762720176614,2.93292951866789));
#29569=CARTESIAN_POINT('Ctrl Pts',(19.797461020943,-32.6100437093729,3.17430677585578));
#29570=CARTESIAN_POINT('Ctrl Pts',(19.8424329629628,-32.649106219757,3.4144113931834));
#29571=CARTESIAN_POINT('Ctrl Pts',(19.8907242666033,-32.6933764227087,3.6527571061464));
#29572=CARTESIAN_POINT('Ctrl Pts',(19.9390768897696,-32.7377028392568,3.89140546668789));
#29573=CARTESIAN_POINT('Ctrl Pts',(19.9907572100055,-32.7872500836135,4.12829002081164));
#29574=CARTESIAN_POINT('Ctrl Pts',(20.0456444897533,-32.8418926894896,4.36293874377806));
#29575=CARTESIAN_POINT('Ctrl Pts',(20.1005877764142,-32.8965910526139,4.59782690201453));
#29576=CARTESIAN_POINT('Ctrl Pts',(20.1587444351917,-32.9563950254815,4.83047425894971));
#29577=CARTESIAN_POINT('Ctrl Pts',(20.2199684571168,-33.0211385895999,5.0604297595945));
#29578=CARTESIAN_POINT('Ctrl Pts',(20.281371474083,-33.0860714385212,5.29105755998329));
#29579=CARTESIAN_POINT('Ctrl Pts',(20.3458596558642,-33.1559726078591,5.51897736305717));
#29580=CARTESIAN_POINT('Ctrl Pts',(20.4132628895043,-33.2306368658408,5.74376259354365));
#29581=CARTESIAN_POINT('Ctrl Pts',(20.456241195579,-33.27824501695,5.88709234072642));
#29582=CARTESIAN_POINT('Ctrl Pts',(20.5004042255162,-33.3277889511028,6.02914825314203));
#29583=CARTESIAN_POINT('Ctrl Pts',(20.5457035458387,-33.379208101198,6.16982677023483));
#29584=CARTESIAN_POINT('Ctrl Pts',(20.6167342126791,-33.4598348411499,6.39041482339093));
#29585=CARTESIAN_POINT('Ctrl Pts',(20.6911341865981,-33.5454408102123,6.6089005401181));
#29586=CARTESIAN_POINT('Ctrl Pts',(20.7688037431274,-33.6359284429692,6.8248041200805));
#29587=CARTESIAN_POINT('Ctrl Pts',(20.8462979562734,-33.7262117948162,7.04022028559294));
#29588=CARTESIAN_POINT('Ctrl Pts',(20.927046935545,-33.8213547340594,7.25306552029632));
#29589=CARTESIAN_POINT('Ctrl Pts',(21.0109232247562,-33.9212188657881,7.46287566269406));
#29590=CARTESIAN_POINT('Ctrl Pts',(21.0946646065284,-34.0209223750764,7.67234834441878));
#29591=CARTESIAN_POINT('Ctrl Pts',(21.1815231404626,-34.1253317904081,7.87879526533031));
#29592=CARTESIAN_POINT('Ctrl Pts',(21.2713449564538,-34.2342692590686,8.08177334612205));
#29593=CARTESIAN_POINT('Ctrl Pts',(21.3610805851804,-34.3431021983077,8.28455666214114));
#29594=CARTESIAN_POINT('Ctrl Pts',(21.4537736728366,-34.4564543444626,8.48387739272852));
#29595=CARTESIAN_POINT('Ctrl Pts',(21.5492456275379,-34.5741103132398,8.67931873611087));
#29596=CARTESIAN_POINT('Ctrl Pts',(21.6447221741876,-34.6917719409576,8.87476947970466));
#29597=CARTESIAN_POINT('Ctrl Pts',(21.7429776869128,-34.8137376000412,9.06634009532782));
#29598=CARTESIAN_POINT('Ctrl Pts',(21.8438106715178,-34.939756550695,9.25364450340919));
#29599=CARTESIAN_POINT('Ctrl Pts',(21.9446806457081,-35.0658217301572,9.44101762226418));
#29600=CARTESIAN_POINT('Ctrl Pts',(22.0481297867729,-35.1959429263777,9.62412107874944));
#29601=CARTESIAN_POINT('Ctrl Pts',(22.1539362249972,-35.3298371867847,9.80260437466024));
#29602=CARTESIAN_POINT('Ctrl Pts',(22.259915255438,-35.4639498564639,9.98137881379584));
#29603=CARTESIAN_POINT('Ctrl Pts',(22.3682590622494,-35.6018476263936,10.1555177270916));
#29604=CARTESIAN_POINT('Ctrl Pts',(22.4787275806298,-35.7432181181524,10.32470957477));
#29605=CARTESIAN_POINT('Ctrl Pts',(22.510656721724,-35.7840789755632,10.373611745775));
#29606=CARTESIAN_POINT('Ctrl Pts',(22.5427632651449,-35.825229782807,10.4221009095754));
#29607=CARTESIAN_POINT('Ctrl Pts',(22.5750411898809,-35.8666626160155,10.4701702229111));
#29608=CARTESIAN_POINT('Ctrl Pts',(26.9229962078193,-35.511683643468,0.));
#29609=CARTESIAN_POINT('Ctrl Pts',(27.1032648219974,-35.3958320397275,1.72780310113343));
#29610=CARTESIAN_POINT('Ctrl Pts',(27.6888332968112,-35.9106393292988,3.28449990511992));
#29611=CARTESIAN_POINT('Ctrl Pts',(28.274401771625,-36.4254466188702,4.84119670910639));
#29612=CARTESIAN_POINT('Ctrl Pts',(29.184995498999,-37.4460030734092,5.91846432228298));
#29613=CARTESIAN_POINT('Ctrl Pts',(30.0955892263729,-38.4665595279482,6.99573193545956));
#29614=CARTESIAN_POINT('Ctrl Pts',(31.1865583607889,-39.7677855943825,7.3802042952164));
#29615=CARTESIAN_POINT('Ctrl Pts',(32.2775274952049,-41.0690116608167,7.76467665497323));
#29616=CARTESIAN_POINT('Ctrl Pts',(33.3684966296209,-42.3702377272509,7.3802042952164));
#29617=CARTESIAN_POINT('Ctrl Pts',(24.8148246247004,-34.4255873115191,0.));
#29618=CARTESIAN_POINT('Ctrl Pts',(24.9950932388786,-34.3097357077786,2.19648874705823));
#29619=CARTESIAN_POINT('Ctrl Pts',(25.6906037706609,-34.9956161772605,4.17545672685568));
#29620=CARTESIAN_POINT('Ctrl Pts',(26.3861143024432,-35.6814966467423,6.15442470665315));
#29621=CARTESIAN_POINT('Ctrl Pts',(27.4948167710208,-37.0103163197461,7.52391304034141));
#29622=CARTESIAN_POINT('Ctrl Pts',(28.6035192395985,-38.33913599275,8.89340137402968));
#29623=CARTESIAN_POINT('Ctrl Pts',(29.9415259336135,-40.0247600051861,9.38216610144961));
#29624=CARTESIAN_POINT('Ctrl Pts',(31.2795326276286,-41.7103840176223,9.87093082886955));
#29625=CARTESIAN_POINT('Ctrl Pts',(32.6175393216436,-43.3960080300584,9.38216610144961));
#29626=CARTESIAN_POINT('Ctrl Pts',(22.959051956675,-32.9490709821979,0.));
#29627=CARTESIAN_POINT('Ctrl Pts',(23.1393205708531,-32.8332193784574,2.7089937269807));
#29628=CARTESIAN_POINT('Ctrl Pts',(23.9550520912431,-33.7061673576819,5.14971273833323));
#29629=CARTESIAN_POINT('Ctrl Pts',(24.7707836116331,-34.5791153369064,7.59043174968579));
#29630=CARTESIAN_POINT('Ctrl Pts',(26.0961168162186,-36.2450190148586,9.27946171175752));
#29631=CARTESIAN_POINT('Ctrl Pts',(27.4214500208042,-37.9109226928107,10.9684916738293));
#29632=CARTESIAN_POINT('Ctrl Pts',(29.0295908241594,-40.0168835841569,11.5712994880388));
#29633=CARTESIAN_POINT('Ctrl Pts',(30.6377316275147,-42.1228444755031,12.1741073022483));
#29634=CARTESIAN_POINT('Ctrl Pts',(32.2458724308699,-44.2288053668492,11.5712994880388));
#29635=CARTESIAN_POINT('Ctrl Pts',(21.4269965203137,-31.1388779521432,0.));
#29636=CARTESIAN_POINT('Ctrl Pts',(21.6072651344918,-31.0230263484027,3.24562220582792));
#29637=CARTESIAN_POINT('Ctrl Pts',(22.5488764195073,-32.0918470647275,6.16982677025168));
#29638=CARTESIAN_POINT('Ctrl Pts',(23.4904877045229,-33.1606677810523,9.09403133467541));
#29639=CARTESIAN_POINT('Ctrl Pts',(25.0426484071614,-35.1795219354009,11.1176436806954));
#29640=CARTESIAN_POINT('Ctrl Pts',(26.5948091097998,-37.1983760897496,13.1412560267153));
#29641=CARTESIAN_POINT('Ctrl Pts',(28.4857991767894,-39.7444590262845,13.8634749112255));
#29642=CARTESIAN_POINT('Ctrl Pts',(30.3767892437789,-42.2905419628193,14.5856937957357));
#29643=CARTESIAN_POINT('Ctrl Pts',(32.2677793107685,-44.8366248993542,13.8634749112255));
#29644=CARTESIAN_POINT('',(21.4269965203137,-31.1388779521432,0.));
#29645=CARTESIAN_POINT('Ctrl Pts',(21.4269965203137,-31.1388779521432,0.));
#29646=CARTESIAN_POINT('Ctrl Pts',(21.6072651344918,-31.0230263484027,3.24562220582792));
#29647=CARTESIAN_POINT('Ctrl Pts',(22.5488764195073,-32.0918470647275,6.16982677025168));
#29648=CARTESIAN_POINT('Ctrl Pts',(23.3349693300818,-32.9841392463831,8.61106394926976));
#29649=CARTESIAN_POINT('Ctrl Pts',(24.5639673341825,-34.5610181206248,10.4489096280657));
#29650=CARTESIAN_POINT('Origin',(35.1666259835199,-19.5103534449756,1.04083408558608E-14));
#29651=CARTESIAN_POINT('Ctrl Pts',(21.4269965203137,-31.1388779521432,0.));
#29652=CARTESIAN_POINT('Ctrl Pts',(21.6072651344918,-31.0230263484027,3.24562220582792));
#29653=CARTESIAN_POINT('Ctrl Pts',(22.5488764195073,-32.0918470647275,6.16982677025167));
#29654=CARTESIAN_POINT('Ctrl Pts',(23.4904877045229,-33.1606677810523,9.09403133467541));
#29655=CARTESIAN_POINT('Ctrl Pts',(25.0426484071614,-35.1795219354009,11.1176436806954));
#29656=CARTESIAN_POINT('Ctrl Pts',(26.5948091097998,-37.1983760897496,13.1412560267153));
#29657=CARTESIAN_POINT('Ctrl Pts',(28.4857991767894,-39.7444590262845,13.8634749112255));
#29658=CARTESIAN_POINT('Ctrl Pts',(30.3767892437789,-42.2905419628193,14.5856937957357));
#29659=CARTESIAN_POINT('Ctrl Pts',(32.2677793107685,-44.8366248993542,13.8634749112255));
#29660=CARTESIAN_POINT('Ctrl Pts',(20.4854409432117,-30.995096537391,0.));
#29661=CARTESIAN_POINT('Ctrl Pts',(20.6657095573898,-30.8792449336506,3.38941559469372));
#29662=CARTESIAN_POINT('Ctrl Pts',(21.6410512138981,-32.0005511325099,6.44317352589574));
#29663=CARTESIAN_POINT('Ctrl Pts',(22.6163928704065,-33.1218573313692,9.49693145709775));
#29664=CARTESIAN_POINT('Ctrl Pts',(24.2293336022805,-35.2352870572788,11.6101975146502));
#29665=CARTESIAN_POINT('Ctrl Pts',(25.8422743341546,-37.3487167831883,13.7234635722027));
#29666=CARTESIAN_POINT('Ctrl Pts',(27.8090558579143,-40.0127335284696,14.4776794959001));
#29667=CARTESIAN_POINT('Ctrl Pts',(29.775837381674,-42.6767502737508,15.2318954195974));
#29668=CARTESIAN_POINT('Ctrl Pts',(31.7426189054336,-45.3407670190321,14.4776794959001));
#29669=CARTESIAN_POINT('Ctrl Pts',(19.6841717937384,-31.5100409519664,0.));
#29670=CARTESIAN_POINT('Ctrl Pts',(19.8644404079165,-31.3941893482259,3.38941559469373));
#29671=CARTESIAN_POINT('Ctrl Pts',(20.8397820644248,-32.5154955470852,6.44317352589574));
#29672=CARTESIAN_POINT('Ctrl Pts',(21.8151237209332,-33.6368017459446,9.49693145709774));
#29673=CARTESIAN_POINT('Ctrl Pts',(23.4280644528072,-35.7502314718541,11.6101975146502));
#29674=CARTESIAN_POINT('Ctrl Pts',(25.0410051846813,-37.8636611977637,13.7234635722027));
#29675=CARTESIAN_POINT('Ctrl Pts',(27.007786708441,-40.5276779430449,14.4776794959001));
#29676=CARTESIAN_POINT('Ctrl Pts',(28.9745682322006,-43.1916946883262,15.2318954195974));
#29677=CARTESIAN_POINT('Ctrl Pts',(30.9413497559604,-45.8557114336074,14.4776794959001));
#29678=CARTESIAN_POINT('Ctrl Pts',(19.4238236466305,-32.4262389885815,0.));
#29679=CARTESIAN_POINT('Ctrl Pts',(19.6040922608086,-32.3103873848411,3.24562220582793));
#29680=CARTESIAN_POINT('Ctrl Pts',(20.5457035458241,-33.3792081011658,6.16982677025167));
#29681=CARTESIAN_POINT('Ctrl Pts',(21.4873148308396,-34.4480288174907,9.09403133467541));
#29682=CARTESIAN_POINT('Ctrl Pts',(23.0394755334781,-36.4668829718393,11.1176436806954));
#29683=CARTESIAN_POINT('Ctrl Pts',(24.5916362361166,-38.4857371261879,13.1412560267153));
#29684=CARTESIAN_POINT('Ctrl Pts',(26.4826263031061,-41.0318200627228,13.8634749112255));
#29685=CARTESIAN_POINT('Ctrl Pts',(28.3736163700957,-43.5779029992577,14.5856937957357));
#29686=CARTESIAN_POINT('Ctrl Pts',(30.2646064370852,-46.1239859357925,13.8634749112255));
#29687=CARTESIAN_POINT('',(20.182117531154,-31.4039970697876,1.88545294717751E-29));
#29688=CARTESIAN_POINT('Origin',(21.1552751870371,-32.9182507396845,0.));
#29689=CARTESIAN_POINT('Origin',(21.1552751870371,-32.9182507396845,0.));
#29690=CARTESIAN_POINT('Ctrl Pts',(14.6113821712778,-34.8604849513725,0.));
#29691=CARTESIAN_POINT('Ctrl Pts',(14.8063033131395,-34.7714674485864,3.24562220582793));
#29692=CARTESIAN_POINT('Ctrl Pts',(15.586221305578,-35.9634143688745,6.16982677025167));
#29693=CARTESIAN_POINT('Ctrl Pts',(16.3661392980166,-37.1553612891626,9.09403133467541));
#29694=CARTESIAN_POINT('Ctrl Pts',(17.6151883402596,-39.3745619185374,11.1176436806954));
#29695=CARTESIAN_POINT('Ctrl Pts',(18.8642373825027,-41.5937625479123,13.1412560267153));
#29696=CARTESIAN_POINT('Ctrl Pts',(20.3736345158495,-44.3830459768616,13.8634749112255));
#29697=CARTESIAN_POINT('Ctrl Pts',(21.8830316491963,-47.172329405811,14.5856937957357));
#29698=CARTESIAN_POINT('Ctrl Pts',(23.3924287825431,-49.9616128347604,13.8634749112255));
#29699=CARTESIAN_POINT('Ctrl Pts',(15.305921749416,-37.1279962392258,0.));
#29700=CARTESIAN_POINT('Ctrl Pts',(15.5008428912777,-37.0389787364397,2.70899372698069));
#29701=CARTESIAN_POINT('Ctrl Pts',(16.1840379904935,-38.0191320633215,5.14971273833323));
#29702=CARTESIAN_POINT('Ctrl Pts',(16.8672330897094,-38.9992853902033,7.59043174968577));
#29703=CARTESIAN_POINT('Ctrl Pts',(17.9419935007382,-40.8368471514174,9.27946171175751));
#29704=CARTESIAN_POINT('Ctrl Pts',(19.0167539117671,-42.6744089126316,10.9684916738292));
#29705=CARTESIAN_POINT('Ctrl Pts',(20.30881667683,-44.9877964569989,11.5712994880388));
#29706=CARTESIAN_POINT('Ctrl Pts',(21.6008794418929,-47.3011840013662,12.1741073022483));
#29707=CARTESIAN_POINT('Ctrl Pts',(22.8929422069557,-49.6145715457335,11.5712994880388));
#29708=CARTESIAN_POINT('Ctrl Pts',(15.5447398754874,-39.4874365476046,0.));
#29709=CARTESIAN_POINT('Ctrl Pts',(15.739661017349,-39.3984190448185,2.19648874705823));
#29710=CARTESIAN_POINT('Ctrl Pts',(16.3304812866721,-40.1762997089269,4.17545672685568));
#29711=CARTESIAN_POINT('Ctrl Pts',(16.9213015559951,-40.9541803730353,6.15442470665314));
#29712=CARTESIAN_POINT('Ctrl Pts',(17.8296082752017,-42.4272593902766,7.5239130403414));
#29713=CARTESIAN_POINT('Ctrl Pts',(18.7379149944082,-43.9003384075178,8.89340137402966));
#29714=CARTESIAN_POINT('Ctrl Pts',(19.8224134008051,-45.7592234042438,9.3821661014496));
#29715=CARTESIAN_POINT('Ctrl Pts',(20.9069118072021,-47.6181084009698,9.87093082886953));
#29716=CARTESIAN_POINT('Ctrl Pts',(21.991410213599,-49.4769933976958,9.3821661014496));
#29717=CARTESIAN_POINT('Ctrl Pts',(15.3186586437002,-41.848131348458,0.));
#29718=CARTESIAN_POINT('Ctrl Pts',(15.5135797855619,-41.7591138456719,1.72780310113342));
#29719=CARTESIAN_POINT('Ctrl Pts',(16.0199233014648,-42.3520162221173,3.28449990511991));
#29720=CARTESIAN_POINT('Ctrl Pts',(16.5262668173678,-42.9449185985627,4.84119670910638));
#29721=CARTESIAN_POINT('Ctrl Pts',(17.2823516867883,-44.0846782589593,5.91846432228297));
#29722=CARTESIAN_POINT('Ctrl Pts',(18.0384365562089,-45.2244379193559,6.99573193545956));
#29723=CARTESIAN_POINT('Ctrl Pts',(18.9331174206825,-46.6676804765724,7.38020429521639));
#29724=CARTESIAN_POINT('Ctrl Pts',(19.8277982851562,-48.1109230337889,7.76467665497321));
#29725=CARTESIAN_POINT('Ctrl Pts',(20.7224791496298,-49.5541655910055,7.38020429521638));
#29726=CARTESIAN_POINT('',(14.6113821712889,-34.8604849513849,1.57949468734771E-9));
#29727=CARTESIAN_POINT('Origin',(-2.59935965651579,-40.1321417817281,0.));
#29728=CARTESIAN_POINT('Ctrl Pts',(14.6113821714909,-34.8604849513684,3.13106366345279E-9));
#29729=CARTESIAN_POINT('Ctrl Pts',(14.6260983377858,-34.8537643034671,0.245038153335408));
#29730=CARTESIAN_POINT('Ctrl Pts',(14.6435771646294,-34.852749515407,0.490791160521576));
#29731=CARTESIAN_POINT('Ctrl Pts',(14.6638259110832,-34.8575316463562,0.736766500725157));
#29732=CARTESIAN_POINT('Ctrl Pts',(14.6840081820396,-34.862298077838,0.981934317700836));
#29733=CARTESIAN_POINT('Ctrl Pts',(14.706942233133,-34.872823533213,1.22732257376552));
#29734=CARTESIAN_POINT('Ctrl Pts',(14.7326128792074,-34.8891527148323,1.47243294816331));
#29735=CARTESIAN_POINT('Ctrl Pts',(14.7582448644189,-34.9054573041506,1.71717417803004));
#29736=CARTESIAN_POINT('Ctrl Pts',(14.7866052020686,-34.9275482079566,1.96163791541569));
#29737=CARTESIAN_POINT('Ctrl Pts',(14.8176563354393,-34.9554233023889,2.20532408778503));
#29738=CARTESIAN_POINT('Ctrl Pts',(14.8486808377688,-34.9832744897134,2.4488012624205));
#29739=CARTESIAN_POINT('Ctrl Pts',(14.8823914884387,-35.0168999484378,2.69150175431039));
#29740=CARTESIAN_POINT('Ctrl Pts',(14.9187287035019,-35.056250564147,2.93292951866801));
#29741=CARTESIAN_POINT('Ctrl Pts',(14.9550583167473,-35.0955929476289,3.17430677585596));
#29742=CARTESIAN_POINT('Ctrl Pts',(14.9940133343936,-35.1406580326362,3.41441139318363));
#29743=CARTESIAN_POINT('Ctrl Pts',(15.0355127954199,-35.1913501978218,3.65275710614669));
#29744=CARTESIAN_POINT('Ctrl Pts',(15.0770649517989,-35.2421067311089,3.89140546668819));
#29745=CARTESIAN_POINT('Ctrl Pts',(15.1211679328242,-35.2985045323755,4.12829002081193));
#29746=CARTESIAN_POINT('Ctrl Pts',(15.167720085587,-35.3604022296525,4.36293874377836));
#29747=CARTESIAN_POINT('Ctrl Pts',(15.2143197401095,-35.4223630872641,4.5978269020147));
#29748=CARTESIAN_POINT('Ctrl Pts',(15.2633734552288,-35.4898348974064,4.83047425894974));
#29749=CARTESIAN_POINT('Ctrl Pts',(15.3147603350317,-35.5626325521734,5.0604297595944));
#29750=CARTESIAN_POINT('Ctrl Pts',(15.3662974499281,-35.635643038747,5.29105755998315));
#29751=CARTESIAN_POINT('Ctrl Pts',(15.4201812613936,-35.714010340131,5.51897736305698));
#29752=CARTESIAN_POINT('Ctrl Pts',(15.4762725955032,-35.797507103918,5.74376259354342));
#29753=CARTESIAN_POINT('Ctrl Pts',(15.5120380980662,-35.8507471233724,5.88709234072627));
#29754=CARTESIAN_POINT('Ctrl Pts',(15.5487007750601,-35.9060718261752,6.02914825314196));
#29755=CARTESIAN_POINT('Ctrl Pts',(15.5862213055879,-35.9634143689084,6.16982677023484));
#29756=CARTESIAN_POINT('Ctrl Pts',(15.6450546012009,-36.0533291627655,6.39041482339095));
#29757=CARTESIAN_POINT('Ctrl Pts',(15.706514291019,-36.1486520067524,6.60890054011813));
#29758=CARTESIAN_POINT('Ctrl Pts',(15.7705155506315,-36.2492721362564,6.82480412008053));
#29759=CARTESIAN_POINT('Ctrl Pts',(15.8343723238082,-36.3496651101704,7.04022028559287));
#29760=CARTESIAN_POINT('Ctrl Pts',(15.9007591428899,-36.4553314094026,7.25306552029615));
#29761=CARTESIAN_POINT('Ctrl Pts',(15.9695695446603,-36.5661159087965,7.4628756626938));
#29762=CARTESIAN_POINT('Ctrl Pts',(16.0382692711115,-36.6767222213245,7.67234834441846));
#29763=CARTESIAN_POINT('Ctrl Pts',(16.1093847013528,-36.7924301575636,7.87879526532994));
#29764=CARTESIAN_POINT('Ctrl Pts',(16.1827888425353,-36.913041777084,8.08177334612163));
#29765=CARTESIAN_POINT('Ctrl Pts',(16.2561225498028,-37.0335376654154,8.28455666214069));
#29766=CARTESIAN_POINT('Ctrl Pts',(16.3317404631311,-37.1589276519416,8.48387739272803));
#29767=CARTESIAN_POINT('Ctrl Pts',(16.4094964608244,-37.2889731283954,8.67931873611035));
#29768=CARTESIAN_POINT('Ctrl Pts',(16.4872561983753,-37.4190248596925,8.87476947970416));
#29769=CARTESIAN_POINT('Ctrl Pts',(16.5671540886063,-37.5537323016295,9.06634009532735));
#29770=CARTESIAN_POINT('Ctrl Pts',(16.6490263722356,-37.6928185909666,9.25364450340874));
#29771=CARTESIAN_POINT('Ctrl Pts',(16.7309286899041,-37.8319559027364,9.44101762226376));
#29772=CARTESIAN_POINT('Ctrl Pts',(16.8148066908781,-37.9754750005788,9.62412107874904));
#29773=CARTESIAN_POINT('Ctrl Pts',(16.9004810321061,-38.1230642366186,9.80260437465986));
#29774=CARTESIAN_POINT('Ctrl Pts',(16.9862951259303,-38.2708942212726,9.9813788137956));
#29775=CARTESIAN_POINT('Ctrl Pts',(17.0739112501815,-38.4228073220811,10.1555177270914));
#29776=CARTESIAN_POINT('Ctrl Pts',(17.1631362396561,-38.5784601754009,10.32470957477));
#29777=CARTESIAN_POINT('Ctrl Pts',(17.1889252818169,-38.6234491187491,10.3736117457733));
#29778=CARTESIAN_POINT('Ctrl Pts',(17.2148486564411,-38.6687503076427,10.4221009095721));
#29779=CARTESIAN_POINT('Ctrl Pts',(17.240901531486,-38.7143550419874,10.4701702229062));
#29780=CARTESIAN_POINT('Ctrl Pts',(21.5951194116464,-38.9817677587451,0.));
#29781=CARTESIAN_POINT('Ctrl Pts',(21.7900405535081,-38.892750255959,1.72780310113343));
#29782=CARTESIAN_POINT('Ctrl Pts',(22.296384069411,-39.4856526324043,3.28449990511992));
#29783=CARTESIAN_POINT('Ctrl Pts',(22.802727585314,-40.0785550088497,4.84119670910638));
#29784=CARTESIAN_POINT('Ctrl Pts',(23.5588124547345,-41.2183146692463,5.91846432228299));
#29785=CARTESIAN_POINT('Ctrl Pts',(24.3148973241551,-42.3580743296429,6.99573193545957));
#29786=CARTESIAN_POINT('Ctrl Pts',(25.2095781886287,-43.8013168868595,7.3802042952164));
#29787=CARTESIAN_POINT('Ctrl Pts',(26.1042590531024,-45.244559444076,7.76467665497323));
#29788=CARTESIAN_POINT('Ctrl Pts',(26.9989399175761,-46.6878020012926,7.3802042952164));
#29789=CARTESIAN_POINT('Ctrl Pts',(19.6629735993418,-37.60670222353,0.));
#29790=CARTESIAN_POINT('Ctrl Pts',(19.8578947412035,-37.5176847207439,2.19648874705824));
#29791=CARTESIAN_POINT('Ctrl Pts',(20.4487150105265,-38.2955653848523,4.17545672685568));
#29792=CARTESIAN_POINT('Ctrl Pts',(21.0395352798495,-39.0734460489607,6.15442470665314));
#29793=CARTESIAN_POINT('Ctrl Pts',(21.9478419990561,-40.5465250662019,7.5239130403414));
#29794=CARTESIAN_POINT('Ctrl Pts',(22.8561487182626,-42.0196040834432,8.89340137402968));
#29795=CARTESIAN_POINT('Ctrl Pts',(23.9406471246595,-43.8784890801692,9.38216610144961));
#29796=CARTESIAN_POINT('Ctrl Pts',(25.0251455310565,-45.7373740768952,9.87093082886955));
#29797=CARTESIAN_POINT('Ctrl Pts',(26.1096439374534,-47.5962590736212,9.3821661014496));
#29798=CARTESIAN_POINT('Ctrl Pts',(18.0362202038888,-35.8811107143584,0.));
#29799=CARTESIAN_POINT('Ctrl Pts',(18.2311413457505,-35.7920932115723,2.70899372698068));
#29800=CARTESIAN_POINT('Ctrl Pts',(18.9143364449663,-36.7722465384541,5.14971273833322));
#29801=CARTESIAN_POINT('Ctrl Pts',(19.5975315441822,-37.7523998653359,7.59043174968576));
#29802=CARTESIAN_POINT('Ctrl Pts',(20.672291955211,-39.58996162655,9.2794617117575));
#29803=CARTESIAN_POINT('Ctrl Pts',(21.7470523662399,-41.4275233877642,10.9684916738292));
#29804=CARTESIAN_POINT('Ctrl Pts',(23.0391151313028,-43.7409109321315,11.5712994880388));
#29805=CARTESIAN_POINT('Ctrl Pts',(24.3311778963657,-46.0542984764988,12.1741073022483));
#29806=CARTESIAN_POINT('Ctrl Pts',(25.6232406614285,-48.367686020866,11.5712994880388));
#29807=CARTESIAN_POINT('Ctrl Pts',(16.7773762111438,-33.8713086176154,0.));
#29808=CARTESIAN_POINT('Ctrl Pts',(16.9722973530055,-33.7822911148293,3.24562220582793));
#29809=CARTESIAN_POINT('Ctrl Pts',(17.752215345444,-34.9742380351174,6.16982677025167));
#29810=CARTESIAN_POINT('Ctrl Pts',(18.5321333378825,-36.1661849554056,9.0940313346754));
#29811=CARTESIAN_POINT('Ctrl Pts',(19.7811823801256,-38.3853855847804,11.1176436806954));
#29812=CARTESIAN_POINT('Ctrl Pts',(21.0302314223687,-40.6045862141552,13.1412560267153));
#29813=CARTESIAN_POINT('Ctrl Pts',(22.5396285557155,-43.3938696431046,13.8634749112255));
#29814=CARTESIAN_POINT('Ctrl Pts',(24.0490256890623,-46.183153072054,14.5856937957357));
#29815=CARTESIAN_POINT('Ctrl Pts',(25.558422822409,-48.9724365010033,13.8634749112255));
#29816=CARTESIAN_POINT('',(16.7773762111438,-33.8713086176154,0.));
#29817=CARTESIAN_POINT('Ctrl Pts',(16.7773762111438,-33.8713086176154,0.));
#29818=CARTESIAN_POINT('Ctrl Pts',(16.9722973530055,-33.7822911148293,3.24562220582793));
#29819=CARTESIAN_POINT('Ctrl Pts',(17.752215345444,-34.9742380351174,6.16982677025167));
#29820=CARTESIAN_POINT('Ctrl Pts',(18.4033205461164,-35.969320654379,8.61106394926976));
#29821=CARTESIAN_POINT('Ctrl Pts',(19.3953958606399,-37.7050538275443,10.4489096280657));
#29822=CARTESIAN_POINT('Origin',(32.0320676419188,-24.3164988679741,0.));
#29823=CARTESIAN_POINT('Ctrl Pts',(16.7773762111438,-33.8713086176154,0.));
#29824=CARTESIAN_POINT('Ctrl Pts',(16.9722973530055,-33.7822911148293,3.24562220582793));
#29825=CARTESIAN_POINT('Ctrl Pts',(17.752215345444,-34.9742380351174,6.16982677025167));
#29826=CARTESIAN_POINT('Ctrl Pts',(18.5321333378825,-36.1661849554056,9.0940313346754));
#29827=CARTESIAN_POINT('Ctrl Pts',(19.7811823801256,-38.3853855847804,11.1176436806954));
#29828=CARTESIAN_POINT('Ctrl Pts',(21.0302314223687,-40.6045862141552,13.1412560267153));
#29829=CARTESIAN_POINT('Ctrl Pts',(22.5396285557155,-43.3938696431046,13.8634749112255));
#29830=CARTESIAN_POINT('Ctrl Pts',(24.0490256890623,-46.183153072054,14.5856937957357));
#29831=CARTESIAN_POINT('Ctrl Pts',(25.5584228224091,-48.9724365010033,13.8634749112255));
#29832=CARTESIAN_POINT('Ctrl Pts',(15.8658665409928,-33.5949933606692,0.));
#29833=CARTESIAN_POINT('Ctrl Pts',(16.0607876828545,-33.5059758578831,3.38941559469373));
#29834=CARTESIAN_POINT('Ctrl Pts',(16.8666232572806,-34.7546743665352,6.44317352589574));
#29835=CARTESIAN_POINT('Ctrl Pts',(17.6724588317067,-36.0033728751874,9.49693145709775));
#29836=CARTESIAN_POINT('Ctrl Pts',(18.968209742954,-38.3248363332023,11.6101975146502));
#29837=CARTESIAN_POINT('Ctrl Pts',(20.2639606542014,-40.6462997912171,13.7234635722027));
#29838=CARTESIAN_POINT('Ctrl Pts',(21.8315940656519,-43.5631028816991,14.4776794959001));
#29839=CARTESIAN_POINT('Ctrl Pts',(23.3992274771025,-46.4799059721811,15.2318954195974));
#29840=CARTESIAN_POINT('Ctrl Pts',(24.966860888553,-49.3967090626631,14.4776794959001));
#29841=CARTESIAN_POINT('Ctrl Pts',(14.9994689250464,-33.990663894172,0.));
#29842=CARTESIAN_POINT('Ctrl Pts',(15.1943900669081,-33.9016463913859,3.38941559469372));
#29843=CARTESIAN_POINT('Ctrl Pts',(16.0002256413342,-35.150344900038,6.44317352589574));
#29844=CARTESIAN_POINT('Ctrl Pts',(16.8060612157603,-36.3990434086902,9.49693145709774));
#29845=CARTESIAN_POINT('Ctrl Pts',(18.1018121270076,-38.7205068667051,11.6101975146502));
#29846=CARTESIAN_POINT('Ctrl Pts',(19.397563038255,-41.04197032472,13.7234635722027));
#29847=CARTESIAN_POINT('Ctrl Pts',(20.9651964497055,-43.9587734152019,14.4776794959001));
#29848=CARTESIAN_POINT('Ctrl Pts',(22.5328298611561,-46.8755765056839,15.2318954195974));
#29849=CARTESIAN_POINT('Ctrl Pts',(24.1004632726066,-49.7923795961659,14.4776794959001));
#29850=CARTESIAN_POINT('Ctrl Pts',(14.6113821712778,-34.8604849513725,0.));
#29851=CARTESIAN_POINT('Ctrl Pts',(14.8063033131395,-34.7714674485864,3.24562220582793));
#29852=CARTESIAN_POINT('Ctrl Pts',(15.586221305578,-35.9634143688745,6.16982677025167));
#29853=CARTESIAN_POINT('Ctrl Pts',(16.3661392980166,-37.1553612891626,9.0940313346754));
#29854=CARTESIAN_POINT('Ctrl Pts',(17.6151883402596,-39.3745619185374,11.1176436806954));
#29855=CARTESIAN_POINT('Ctrl Pts',(18.8642373825027,-41.5937625479123,13.1412560267153));
#29856=CARTESIAN_POINT('Ctrl Pts',(20.3736345158495,-44.3830459768616,13.8634749112255));
#29857=CARTESIAN_POINT('Ctrl Pts',(21.8830316491963,-47.172329405811,14.5856937957357));
#29858=CARTESIAN_POINT('Ctrl Pts',(23.3924287825431,-49.9616128347604,13.8634749112255));
#29859=CARTESIAN_POINT('',(15.5074379107559,-33.9565644529094,1.82251475138647E-29));
#29860=CARTESIAN_POINT('Origin',(16.2551894587634,-35.5938999782226,0.));
#29861=CARTESIAN_POINT('Origin',(16.2551894587634,-35.5938999782226,0.));
#29862=CARTESIAN_POINT('Ctrl Pts',(9.50149509066468,-36.5850719698906,0.));
#29863=CARTESIAN_POINT('Ctrl Pts',(9.7071007278678,-36.5247007077103,3.24562220582793));
#29864=CARTESIAN_POINT('Ctrl Pts',(10.309448546501,-37.8155092299558,6.16982677025168));
#29865=CARTESIAN_POINT('Ctrl Pts',(10.9117963651343,-39.1063177522012,9.09403133467541));
#29866=CARTESIAN_POINT('Ctrl Pts',(11.8323067104418,-41.4806883314343,11.1176436806954));
#29867=CARTESIAN_POINT('Ctrl Pts',(12.7528170557494,-43.8550589106674,13.1412560267153));
#29868=CARTESIAN_POINT('Ctrl Pts',(13.8498942825604,-46.8307610650471,13.8634749112255));
#29869=CARTESIAN_POINT('Ctrl Pts',(14.9469715093714,-49.8064632194268,14.5856937957357));
#29870=CARTESIAN_POINT('Ctrl Pts',(16.0440487361823,-52.7821653738064,13.8634749112255));
#29871=CARTESIAN_POINT('Ctrl Pts',(9.86626475512707,-38.9283465500521,0.));
#29872=CARTESIAN_POINT('Ctrl Pts',(10.0718703923302,-38.8679752878718,2.70899372698069));
#29873=CARTESIAN_POINT('Ctrl Pts',(10.6086211883238,-39.9353808672043,5.14971273833323));
#29874=CARTESIAN_POINT('Ctrl Pts',(11.1453719843174,-41.0027864465368,7.59043174968577));
#29875=CARTESIAN_POINT('Ctrl Pts',(11.9476805791742,-42.9745988326452,9.27946171175751));
#29876=CARTESIAN_POINT('Ctrl Pts',(12.7499891740309,-44.9464112187536,10.9684916738293));
#29877=CARTESIAN_POINT('Ctrl Pts',(13.6996712289061,-47.4201315169975,11.5712994880388));
#29878=CARTESIAN_POINT('Ctrl Pts',(14.6493532837812,-49.8938518152413,12.1741073022483));
#29879=CARTESIAN_POINT('Ctrl Pts',(15.5990353386564,-52.3675721134852,11.5712994880388));
#29880=CARTESIAN_POINT('Ctrl Pts',(9.76686869111994,-41.2977585211121,-1.05434036998093E-14));
#29881=CARTESIAN_POINT('Ctrl Pts',(9.97247432832304,-41.2373872589318,2.19648874705824));
#29882=CARTESIAN_POINT('Ctrl Pts',(10.4465769382884,-42.0914327105682,4.17545672685568));
#29883=CARTESIAN_POINT('Ctrl Pts',(10.9206795482537,-42.9454781622046,6.15442470665314));
#29884=CARTESIAN_POINT('Ctrl Pts',(11.6101000126264,-44.5328288829013,7.5239130403414));
#29885=CARTESIAN_POINT('Ctrl Pts',(12.2995204769991,-46.120179603598,8.89340137402967));
#29886=CARTESIAN_POINT('Ctrl Pts',(13.1084333356587,-48.1144840466621,9.3821661014496));
#29887=CARTESIAN_POINT('Ctrl Pts',(13.9173461943184,-50.1087884897263,9.87093082886953));
#29888=CARTESIAN_POINT('Ctrl Pts',(14.7262590529781,-52.1030929327905,9.3821661014496));
#29889=CARTESIAN_POINT('Ctrl Pts',(9.20712674149411,-43.6022501387952,0.));
#29890=CARTESIAN_POINT('Ctrl Pts',(9.41273237869722,-43.541878876615,1.72780310113342));
#29891=CARTESIAN_POINT('Ctrl Pts',(9.82954324187965,-44.2008065573392,3.28449990511991));
#29892=CARTESIAN_POINT('Ctrl Pts',(10.2463541050621,-44.8597342380635,4.84119670910639));
#29893=CARTESIAN_POINT('Ctrl Pts',(10.8325384089565,-46.0954948844274,5.91846432228298));
#29894=CARTESIAN_POINT('Ctrl Pts',(11.418722712851,-47.3312555307914,6.99573193545957));
#29895=CARTESIAN_POINT('Ctrl Pts',(12.0989021850282,-48.8871343222931,7.38020429521639));
#29896=CARTESIAN_POINT('Ctrl Pts',(12.7790816572054,-50.4430131137949,7.76467665497322));
#29897=CARTESIAN_POINT('Ctrl Pts',(13.4592611293826,-51.9988919052966,7.38020429521639));
#29898=CARTESIAN_POINT('',(9.50149509067387,-36.5850719699046,1.57948920827305E-9));
#29899=CARTESIAN_POINT('Origin',(-8.28430119040681,-39.353726995029,0.));
#29900=CARTESIAN_POINT('Ctrl Pts',(9.50149509087619,-36.5850719699169,3.13105453121543E-9));
#29901=CARTESIAN_POINT('Ctrl Pts',(9.5170179157363,-36.5805140573471,0.245038153335614));
#29902=CARTESIAN_POINT('Ctrl Pts',(9.53446325272375,-36.5819970947818,0.490791160521999));
#29903=CARTESIAN_POINT('Ctrl Pts',(9.5538253279423,-36.58961224761,0.736766500725797));
#29904=CARTESIAN_POINT('Ctrl Pts',(9.57312383855526,-36.5972024003191,0.981934317701467));
#29905=CARTESIAN_POINT('Ctrl Pts',(9.59432652559727,-36.6108845775071,1.22732257376614));
#29906=CARTESIAN_POINT('Ctrl Pts',(9.61741199666741,-36.6307008654467,1.47243294816393));
#29907=CARTESIAN_POINT('Ctrl Pts',(9.64046270023572,-36.6504873093851,1.7171741780307));
#29908=CARTESIAN_POINT('Ctrl Pts',(9.66539050713792,-36.6763894565088,1.9616379154164));
#29909=CARTESIAN_POINT('Ctrl Pts',(9.69215854518704,-36.7083998596962,2.2053240877858));
#29910=CARTESIAN_POINT('Ctrl Pts',(9.71890362559667,-36.7403828091234,2.44880126242122));
#29911=CARTESIAN_POINT('Ctrl Pts',(9.7474857487292,-36.7784635349601,2.69150175431106));
#29912=CARTESIAN_POINT('Ctrl Pts',(9.7778529268264,-36.8225849430253,2.93292951866864));
#29913=CARTESIAN_POINT('Ctrl Pts',(9.80821375204938,-36.8666971208039,3.17430677585648));
#29914=CARTESIAN_POINT('Ctrl Pts',(9.84035883349998,-36.9168473852606,3.41441139318403));
#29915=CARTESIAN_POINT('Ctrl Pts',(9.87422164256022,-36.972929566381,3.65275710614698));
#29916=CARTESIAN_POINT('Ctrl Pts',(9.90812745007443,-37.0290829597591,3.89140546668847));
#29917=CARTESIAN_POINT('Ctrl Pts',(9.94375528237788,-37.0911832213397,4.12829002081221));
#29918=CARTESIAN_POINT('Ctrl Pts',(9.98102464057076,-37.1590759513993,4.36293874377864));
#29919=CARTESIAN_POINT('Ctrl Pts',(10.0183320283712,-37.2270379591175,4.59782690201516));
#29920=CARTESIAN_POINT('Ctrl Pts',(10.0572842076518,-37.3008040750529,4.83047425895038));
#29921=CARTESIAN_POINT('Ctrl Pts',(10.0977878566473,-37.3801738701485,5.06042975959522));
#29922=CARTESIAN_POINT('Ctrl Pts',(10.1384099224354,-37.4597757114128,5.29105755998397));
#29923=CARTESIAN_POINT('Ctrl Pts',(10.1805924445719,-37.5450138125793,5.51897736305782));
#29924=CARTESIAN_POINT('Ctrl Pts',(10.2242300213426,-37.6356433288457,5.74376259354427));
#29925=CARTESIAN_POINT('Ctrl Pts',(10.2520546379007,-37.6934314033808,5.88709234072682));
#29926=CARTESIAN_POINT('Ctrl Pts',(10.280470615574,-37.7534106234276,6.02914825314224));
#29927=CARTESIAN_POINT('Ctrl Pts',(10.3094485465059,-37.8155092299908,6.16982677023484));
#29928=CARTESIAN_POINT('Ctrl Pts',(10.3548867946541,-37.9128816718431,6.39041482339091));
#29929=CARTESIAN_POINT('Ctrl Pts',(10.4021550583216,-38.0159808925391,6.60890054011806));
#29930=CARTESIAN_POINT('Ctrl Pts',(10.4511851399361,-38.124685183118,6.82480412008043));
#29931=CARTESIAN_POINT('Ctrl Pts',(10.5001045333893,-38.2331440676597,7.04022028559294));
#29932=CARTESIAN_POINT('Ctrl Pts',(10.5507777480886,-38.3471826657451,7.25306552029639));
#29933=CARTESIAN_POINT('Ctrl Pts',(10.603121481071,-38.4666322798728,7.4628756626942));
#29934=CARTESIAN_POINT('Ctrl Pts',(10.6553810238844,-38.5858897700798,7.67234834441904));
#29935=CARTESIAN_POINT('Ctrl Pts',(10.7093056453531,-38.7105407473187,7.87879526533069));
#29936=CARTESIAN_POINT('Ctrl Pts',(10.7647978150924,-38.8403712129412,8.08177334612254));
#29937=CARTESIAN_POINT('Ctrl Pts',(10.820236738098,-38.9700771015598,8.28455666214159));
#29938=CARTESIAN_POINT('Ctrl Pts',(10.8772401144471,-39.1049523499265,8.48387739272893));
#29939=CARTESIAN_POINT('Ctrl Pts',(10.935697267249,-39.2447399831766,8.67931873611124));
#29940=CARTESIAN_POINT('Ctrl Pts',(10.9941572316853,-39.384534339842,8.87476947970509));
#29941=CARTESIAN_POINT('Ctrl Pts',(11.0540710087835,-39.5292413095788,9.06634009532832));
#29942=CARTESIAN_POINT('Ctrl Pts',(11.1153159078425,-39.6785635418402,9.25364450340974));
#29943=CARTESIAN_POINT('Ctrl Pts',(11.1765832739882,-39.8279405514888,9.44101762226473));
#29944=CARTESIAN_POINT('Ctrl Pts',(11.2391826206558,-39.9819359159959,9.62412107874997));
#29945=CARTESIAN_POINT('Ctrl Pts',(11.3029807823644,-40.140215636435,9.80260437466077));
#29946=CARTESIAN_POINT('Ctrl Pts',(11.3668830120892,-40.2987535438825,9.98137881379633));
#29947=CARTESIAN_POINT('Ctrl Pts',(11.4319878421544,-40.4615894629181,10.155517727092));
#29948=CARTESIAN_POINT('Ctrl Pts',(11.4981529392408,-40.6283560345708,10.3247095747704));
#29949=CARTESIAN_POINT('Ctrl Pts',(11.5172768919405,-40.6765572187088,10.3736117457736));
#29950=CARTESIAN_POINT('Ctrl Pts',(11.5364893726183,-40.7250865876853,10.4221009095722));
#29951=CARTESIAN_POINT('Ctrl Pts',(11.5557868365676,-40.7739348422894,10.4701702229062));
#29952=CARTESIAN_POINT('Ctrl Pts',(15.8276282594342,-41.6582954965895,0.));
#29953=CARTESIAN_POINT('Ctrl Pts',(16.0332338966373,-41.5979242344092,1.72780310113342));
#29954=CARTESIAN_POINT('Ctrl Pts',(16.4500447598197,-42.2568519151334,3.28449990511991));
#29955=CARTESIAN_POINT('Ctrl Pts',(16.8668556230022,-42.9157795958577,4.84119670910639));
#29956=CARTESIAN_POINT('Ctrl Pts',(17.4530399268966,-44.1515402422216,5.91846432228298));
#29957=CARTESIAN_POINT('Ctrl Pts',(18.039224230791,-45.3873008885856,6.99573193545957));
#29958=CARTESIAN_POINT('Ctrl Pts',(18.7194037029683,-46.9431796800874,7.38020429521639));
#29959=CARTESIAN_POINT('Ctrl Pts',(19.3995831751455,-48.4990584715891,7.76467665497321));
#29960=CARTESIAN_POINT('Ctrl Pts',(20.0797626473227,-50.0549372630909,7.38020429521639));
#29961=CARTESIAN_POINT('Ctrl Pts',(14.1108411348339,-40.0222531270435,-1.05434036998093E-14));
#29962=CARTESIAN_POINT('Ctrl Pts',(14.316446772037,-39.9618818648632,2.19648874705824));
#29963=CARTESIAN_POINT('Ctrl Pts',(14.7905493820023,-40.8159273164997,4.17545672685568));
#29964=CARTESIAN_POINT('Ctrl Pts',(15.2646519919676,-41.669972768136,6.15442470665314));
#29965=CARTESIAN_POINT('Ctrl Pts',(15.9540724563403,-43.2573234888327,7.5239130403414));
#29966=CARTESIAN_POINT('Ctrl Pts',(16.643492920713,-44.8446742095294,8.89340137402968));
#29967=CARTESIAN_POINT('Ctrl Pts',(17.4524057793727,-46.8389786525935,9.38216610144961));
#29968=CARTESIAN_POINT('Ctrl Pts',(18.2613186380324,-48.8332830956577,9.87093082886954));
#29969=CARTESIAN_POINT('Ctrl Pts',(19.070231496692,-50.8275875387219,9.38216610144961));
#29970=CARTESIAN_POINT('Ctrl Pts',(12.7462230199154,-38.0827145049534,0.));
#29971=CARTESIAN_POINT('Ctrl Pts',(12.9518286571185,-38.0223432427732,2.70899372698069));
#29972=CARTESIAN_POINT('Ctrl Pts',(13.4885794531121,-39.0897488221056,5.14971273833323));
#29973=CARTESIAN_POINT('Ctrl Pts',(14.0253302491058,-40.1571544014381,7.59043174968578));
#29974=CARTESIAN_POINT('Ctrl Pts',(14.8276388439625,-42.1289667875466,9.27946171175751));
#29975=CARTESIAN_POINT('Ctrl Pts',(15.6299474388193,-44.1007791736549,10.9684916738292));
#29976=CARTESIAN_POINT('Ctrl Pts',(16.5796294936944,-46.5744994718988,11.5712994880388));
#29977=CARTESIAN_POINT('Ctrl Pts',(17.5293115485696,-49.0482197701427,12.1741073022483));
#29978=CARTESIAN_POINT('Ctrl Pts',(18.4789936034447,-51.5219400683866,11.5712994880388));
#29979=CARTESIAN_POINT('Ctrl Pts',(11.7862169042728,-35.9142171164212,0.));
#29980=CARTESIAN_POINT('Ctrl Pts',(11.9918225414759,-35.8538458542409,3.24562220582792));
#29981=CARTESIAN_POINT('Ctrl Pts',(12.5941703601091,-37.1446543764863,6.16982677025168));
#29982=CARTESIAN_POINT('Ctrl Pts',(13.1965181787423,-38.4354628987318,9.0940313346754));
#29983=CARTESIAN_POINT('Ctrl Pts',(14.1170285240499,-40.8098334779648,11.1176436806954));
#29984=CARTESIAN_POINT('Ctrl Pts',(15.0375388693575,-43.1842040571979,13.1412560267153));
#29985=CARTESIAN_POINT('Ctrl Pts',(16.1346160961685,-46.1599062115776,13.8634749112255));
#29986=CARTESIAN_POINT('Ctrl Pts',(17.2316933229794,-49.1356083659573,14.5856937957357));
#29987=CARTESIAN_POINT('Ctrl Pts',(18.3287705497904,-52.111310520337,13.8634749112255));
#29988=CARTESIAN_POINT('',(11.7862169042728,-35.9142171164212,0.));
#29989=CARTESIAN_POINT('Ctrl Pts',(11.7862169042728,-35.9142171164212,0.));
#29990=CARTESIAN_POINT('Ctrl Pts',(11.9918225414759,-35.8538458542409,3.24562220582792));
#29991=CARTESIAN_POINT('Ctrl Pts',(12.5941703601091,-37.1446543764863,6.16982677025168));
#29992=CARTESIAN_POINT('Ctrl Pts',(13.097033226626,-38.222270420807,8.61106394926975));
#29993=CARTESIAN_POINT('Ctrl Pts',(13.8319900590775,-40.0815233709314,10.4489096280657));
#29994=CARTESIAN_POINT('Origin',(28.2454287759834,-28.6276304970129,0.));
#29995=CARTESIAN_POINT('Ctrl Pts',(11.7862169042728,-35.9142171164212,0.));
#29996=CARTESIAN_POINT('Ctrl Pts',(11.9918225414759,-35.8538458542409,3.24562220582792));
#29997=CARTESIAN_POINT('Ctrl Pts',(12.5941703601091,-37.1446543764863,6.16982677025168));
#29998=CARTESIAN_POINT('Ctrl Pts',(13.1965181787423,-38.4354628987318,9.0940313346754));
#29999=CARTESIAN_POINT('Ctrl Pts',(14.1170285240499,-40.8098334779648,11.1176436806954));
#30000=CARTESIAN_POINT('Ctrl Pts',(15.0375388693575,-43.1842040571979,13.1412560267153));
#30001=CARTESIAN_POINT('Ctrl Pts',(16.1346160961685,-46.1599062115776,13.8634749112255));
#30002=CARTESIAN_POINT('Ctrl Pts',(17.2316933229794,-49.1356083659573,14.5856937957357));
#30003=CARTESIAN_POINT('Ctrl Pts',(18.3287705497904,-52.1113105203369,13.8634749112255));
#30004=CARTESIAN_POINT('Ctrl Pts',(10.9233088493802,-35.5109929990849,0.));
#30005=CARTESIAN_POINT('Ctrl Pts',(11.1289144865834,-35.4506217369046,3.38941559469371));
#30006=CARTESIAN_POINT('Ctrl Pts',(11.7488394904698,-36.8012926546625,6.44317352589574));
#30007=CARTESIAN_POINT('Ctrl Pts',(12.3687644943563,-38.1519635724205,9.49693145709774));
#30008=CARTESIAN_POINT('Ctrl Pts',(13.3209478330609,-40.6342024610833,11.6101975146502));
#30009=CARTESIAN_POINT('Ctrl Pts',(14.2731311717655,-43.1164413497461,13.7234635722027));
#30010=CARTESIAN_POINT('Ctrl Pts',(15.4097039753313,-46.2266530858721,14.4776794959001));
#30011=CARTESIAN_POINT('Ctrl Pts',(16.546276778897,-49.3368648219981,15.2318954195974));
#30012=CARTESIAN_POINT('Ctrl Pts',(17.6828495824628,-52.4470765581242,14.4776794959001));
#30013=CARTESIAN_POINT('Ctrl Pts',(10.009420123937,-35.7793349404727,0.));
#30014=CARTESIAN_POINT('Ctrl Pts',(10.2150257611401,-35.7189636782924,3.38941559469371));
#30015=CARTESIAN_POINT('Ctrl Pts',(10.8349507650266,-37.0696345960503,6.44317352589574));
#30016=CARTESIAN_POINT('Ctrl Pts',(11.4548757689131,-38.4203055138083,9.49693145709774));
#30017=CARTESIAN_POINT('Ctrl Pts',(12.4070591076177,-40.9025444024711,11.6101975146502));
#30018=CARTESIAN_POINT('Ctrl Pts',(13.3592424463223,-43.3847832911339,13.7234635722027));
#30019=CARTESIAN_POINT('Ctrl Pts',(14.4958152498881,-46.4949950272599,14.4776794959001));
#30020=CARTESIAN_POINT('Ctrl Pts',(15.6323880534538,-49.6052067633859,15.2318954195974));
#30021=CARTESIAN_POINT('Ctrl Pts',(16.7689608570196,-52.7154184995119,14.4776794959001));
#30022=CARTESIAN_POINT('Ctrl Pts',(9.50149509066469,-36.5850719698907,0.));
#30023=CARTESIAN_POINT('Ctrl Pts',(9.70710072786781,-36.5247007077104,3.24562220582793));
#30024=CARTESIAN_POINT('Ctrl Pts',(10.309448546501,-37.8155092299558,6.16982677025168));
#30025=CARTESIAN_POINT('Ctrl Pts',(10.9117963651343,-39.1063177522012,9.09403133467541));
#30026=CARTESIAN_POINT('Ctrl Pts',(11.8323067104419,-41.4806883314343,11.1176436806954));
#30027=CARTESIAN_POINT('Ctrl Pts',(12.7528170557494,-43.8550589106674,13.1412560267153));
#30028=CARTESIAN_POINT('Ctrl Pts',(13.8498942825604,-46.8307610650471,13.8634749112255));
#30029=CARTESIAN_POINT('Ctrl Pts',(14.9469715093714,-49.8064632194267,14.5856937957357));
#30030=CARTESIAN_POINT('Ctrl Pts',(16.0440487361824,-52.7821653738064,13.8634749112255));
#30031=CARTESIAN_POINT('',(10.5170715743482,-35.8178741063813,1.72247541091518E-29));
#30032=CARTESIAN_POINT('Origin',(11.0241949492046,-37.5449600575355,0.));
#30033=CARTESIAN_POINT('Origin',(11.0241949492046,-37.5449600575355,0.));
#30034=CARTESIAN_POINT('Ctrl Pts',(4.19818497005484,-37.5648924257372,0.));
#30035=CARTESIAN_POINT('Ctrl Pts',(4.41028956474361,-37.5343963889644,3.24562220582792));
#30036=CARTESIAN_POINT('Ctrl Pts',(4.82280514501186,-38.8977893740386,6.16982677025168));
#30037=CARTESIAN_POINT('Ctrl Pts',(5.23532072528011,-40.2611823591128,9.09403133467541));
#30038=CARTESIAN_POINT('Ctrl Pts',(5.80855343755438,-42.7423875503303,11.1176436806954));
#30039=CARTESIAN_POINT('Ctrl Pts',(6.38178614982864,-45.2235927415478,13.1412560267153));
#30040=CARTESIAN_POINT('Ctrl Pts',(7.0442101414754,-48.325136906711,13.8634749112255));
#30041=CARTESIAN_POINT('Ctrl Pts',(7.70663413312217,-51.4266810718742,14.5856937957357));
#30042=CARTESIAN_POINT('Ctrl Pts',(8.36905812476893,-54.5282252370374,13.8634749112255));
#30043=CARTESIAN_POINT('Ctrl Pts',(4.22575906238186,-39.9362279852005,0.));
#30044=CARTESIAN_POINT('Ctrl Pts',(4.43786365707062,-39.9057319484277,2.7089937269807));
#30045=CARTESIAN_POINT('Ctrl Pts',(4.81724345149705,-41.0386604807592,5.14971273833324));
#30046=CARTESIAN_POINT('Ctrl Pts',(5.19662324592347,-42.1715890130908,7.59043174968579));
#30047=CARTESIAN_POINT('Ctrl Pts',(5.71014733528379,-44.2375116101495,9.27946171175752));
#30048=CARTESIAN_POINT('Ctrl Pts',(6.22367142464412,-46.3034342072083,10.9684916738293));
#30049=CARTESIAN_POINT('Ctrl Pts',(6.81163998135116,-48.8871294476768,11.5712994880388));
#30050=CARTESIAN_POINT('Ctrl Pts',(7.39960853805819,-51.4708246881453,12.1741073022483));
#30051=CARTESIAN_POINT('Ctrl Pts',(7.98757709476522,-54.0545199286138,11.5712994880388));
#30052=CARTESIAN_POINT('Ctrl Pts',(3.79017222552483,-42.2673772240309,0.));
#30053=CARTESIAN_POINT('Ctrl Pts',(4.00227682021359,-42.2368811872581,2.19648874705823));
#30054=CARTESIAN_POINT('Ctrl Pts',(4.35001040888132,-43.1497055238908,4.17545672685568));
#30055=CARTESIAN_POINT('Ctrl Pts',(4.69774399754902,-44.0625298605236,6.15442470665315));
#30056=CARTESIAN_POINT('Ctrl Pts',(5.1542435945577,-45.7318384015438,7.5239130403414));
#30057=CARTESIAN_POINT('Ctrl Pts',(5.61074319156639,-47.401146942564,8.89340137402968));
#30058=CARTESIAN_POINT('Ctrl Pts',(6.12760336939855,-49.4902725446046,9.38216610144961));
#30059=CARTESIAN_POINT('Ctrl Pts',(6.64446354723073,-51.5793981466453,9.87093082886954));
#30060=CARTESIAN_POINT('Ctrl Pts',(7.16132372506291,-53.668523748686,9.38216610144961));
#30061=CARTESIAN_POINT('Ctrl Pts',(2.90816428999222,-44.4687528548128,0.));
#30062=CARTESIAN_POINT('Ctrl Pts',(3.120268884681,-44.43825681804,1.72780310113342));
#30063=CARTESIAN_POINT('Ctrl Pts',(3.43906202795181,-45.149795935654,3.28449990511991));
#30064=CARTESIAN_POINT('Ctrl Pts',(3.75785517122262,-45.8613350532681,4.84119670910638));
#30065=CARTESIAN_POINT('Ctrl Pts',(4.16220588757961,-47.1679401624789,5.91846432228298));
#30066=CARTESIAN_POINT('Ctrl Pts',(4.56655660393661,-48.4745452716896,6.99573193545956));
#30067=CARTESIAN_POINT('Ctrl Pts',(5.01838819123945,-50.1113870920656,7.38020429521639));
#30068=CARTESIAN_POINT('Ctrl Pts',(5.47021977854229,-51.7482289124416,7.76467665497321));
#30069=CARTESIAN_POINT('Ctrl Pts',(5.92205136584512,-53.3850707328175,7.38020429521638));
#30070=CARTESIAN_POINT('',(4.19818497029635,-37.5648924255374,-1.21941740813109E-9));
#30071=CARTESIAN_POINT('Origin',(-13.800598242013,-37.7741838134883,0.));
#30072=CARTESIAN_POINT('Ctrl Pts',(4.19818497005484,-37.5648924257372,0.));
#30073=CARTESIAN_POINT('Ctrl Pts',(4.41028956474361,-37.5343963889644,3.24562220582792));
#30074=CARTESIAN_POINT('Ctrl Pts',(4.82280514501186,-38.8977893740386,6.16982677025168));
#30075=CARTESIAN_POINT('Ctrl Pts',(5.16925602334772,-40.0428338760881,8.6257176219852));
#30076=CARTESIAN_POINT('Ctrl Pts',(5.63542964579419,-42.0034749115208,10.4701702229062));
#30077=CARTESIAN_POINT('Ctrl Pts',(9.73793223897069,-43.4867804707272,0.));
#30078=CARTESIAN_POINT('Ctrl Pts',(9.95003683365946,-43.4562844339544,1.72780310113343));
#30079=CARTESIAN_POINT('Ctrl Pts',(10.2688299769303,-44.1678235515685,3.28449990511991));
#30080=CARTESIAN_POINT('Ctrl Pts',(10.5876231202011,-44.8793626691825,4.84119670910638));
#30081=CARTESIAN_POINT('Ctrl Pts',(10.9919738365581,-46.1859677783933,5.91846432228297));
#30082=CARTESIAN_POINT('Ctrl Pts',(11.3963245529151,-47.4925728876041,6.99573193545955));
#30083=CARTESIAN_POINT('Ctrl Pts',(11.8481561402179,-49.12941470798,7.38020429521639));
#30084=CARTESIAN_POINT('Ctrl Pts',(12.2999877275208,-50.766256528356,7.76467665497321));
#30085=CARTESIAN_POINT('Ctrl Pts',(12.7518193148236,-52.4030983487319,7.38020429521638));
#30086=CARTESIAN_POINT('Ctrl Pts',(8.27145263712638,-41.6230663715378,0.));
#30087=CARTESIAN_POINT('Ctrl Pts',(8.48355723181515,-41.592570334765,2.19648874705824));
#30088=CARTESIAN_POINT('Ctrl Pts',(8.83129082048287,-42.5053946713977,4.17545672685568));
#30089=CARTESIAN_POINT('Ctrl Pts',(9.17902440915059,-43.4182190080305,6.15442470665314));
#30090=CARTESIAN_POINT('Ctrl Pts',(9.63552400615925,-45.0875275490507,7.5239130403414));
#30091=CARTESIAN_POINT('Ctrl Pts',(10.0920236031679,-46.7568360900709,8.89340137402966));
#30092=CARTESIAN_POINT('Ctrl Pts',(10.6088837810001,-48.8459616921115,9.3821661014496));
#30093=CARTESIAN_POINT('Ctrl Pts',(11.1257439588323,-50.9350872941522,9.87093082886954));
#30094=CARTESIAN_POINT('Ctrl Pts',(11.6426041366645,-53.0242128961929,9.3821661014496));
#30095=CARTESIAN_POINT('Ctrl Pts',(7.19674949232852,-39.5090640497074,0.));
#30096=CARTESIAN_POINT('Ctrl Pts',(7.40885408701727,-39.4785680129346,2.7089937269807));
#30097=CARTESIAN_POINT('Ctrl Pts',(7.7882338814437,-40.6114965452661,5.14971273833323));
#30098=CARTESIAN_POINT('Ctrl Pts',(8.16761367587013,-41.7444250775977,7.59043174968578));
#30099=CARTESIAN_POINT('Ctrl Pts',(8.68113776523044,-43.8103476746565,9.27946171175752));
#30100=CARTESIAN_POINT('Ctrl Pts',(9.19466185459077,-45.8762702717153,10.9684916738293));
#30101=CARTESIAN_POINT('Ctrl Pts',(9.78263041129781,-48.4599655121837,11.5712994880388));
#30102=CARTESIAN_POINT('Ctrl Pts',(10.3705989680048,-51.0436607526522,12.1741073022483));
#30103=CARTESIAN_POINT('Ctrl Pts',(10.9585675247119,-53.6273559931207,11.5712994880388));
#30104=CARTESIAN_POINT('Ctrl Pts',(6.55512420987355,-37.2260157227863,0.));
#30105=CARTESIAN_POINT('Ctrl Pts',(6.76722880456232,-37.1955196860135,3.24562220582793));
#30106=CARTESIAN_POINT('Ctrl Pts',(7.17974438483057,-38.5589126710877,6.16982677025168));
#30107=CARTESIAN_POINT('Ctrl Pts',(7.59225996509882,-39.922305656162,9.09403133467541));
#30108=CARTESIAN_POINT('Ctrl Pts',(8.16549267737308,-42.4035108473794,11.1176436806954));
#30109=CARTESIAN_POINT('Ctrl Pts',(8.73872538964735,-44.8847160385969,13.1412560267153));
#30110=CARTESIAN_POINT('Ctrl Pts',(9.4011493812941,-47.9862602037601,13.8634749112255));
#30111=CARTESIAN_POINT('Ctrl Pts',(10.0635733729409,-51.0878043689233,14.5856937957357));
#30112=CARTESIAN_POINT('Ctrl Pts',(10.7259973645876,-54.1893485340865,13.8634749112255));
#30113=CARTESIAN_POINT('',(6.55512420987355,-37.2260157227863,0.));
#30114=CARTESIAN_POINT('Ctrl Pts',(6.55512420987355,-37.2260157227863,0.));
#30115=CARTESIAN_POINT('Ctrl Pts',(6.76722880456232,-37.1955196860135,3.24562220582793));
#30116=CARTESIAN_POINT('Ctrl Pts',(7.17974438483056,-38.5589126710877,6.16982677025168));
#30117=CARTESIAN_POINT('Ctrl Pts',(7.52412807936649,-39.6971249853933,8.61106394926976));
#30118=CARTESIAN_POINT('Ctrl Pts',(7.98700482807783,-41.6420486840549,10.4489096280657));
#30119=CARTESIAN_POINT('Origin',(23.8837944332593,-32.3559861244015,0.));
#30120=CARTESIAN_POINT('Ctrl Pts',(6.55512420987355,-37.2260157227863,0.));
#30121=CARTESIAN_POINT('Ctrl Pts',(6.76722880456232,-37.1955196860135,3.24562220582793));
#30122=CARTESIAN_POINT('Ctrl Pts',(7.17974438483056,-38.5589126710877,6.16982677025168));
#30123=CARTESIAN_POINT('Ctrl Pts',(7.59225996509882,-39.922305656162,9.09403133467541));
#30124=CARTESIAN_POINT('Ctrl Pts',(8.16549267737308,-42.4035108473794,11.1176436806954));
#30125=CARTESIAN_POINT('Ctrl Pts',(8.73872538964735,-44.8847160385969,13.1412560267153));
#30126=CARTESIAN_POINT('Ctrl Pts',(9.4011493812941,-47.9862602037601,13.8634749112255));
#30127=CARTESIAN_POINT('Ctrl Pts',(10.0635733729409,-51.0878043689233,14.5856937957357));
#30128=CARTESIAN_POINT('Ctrl Pts',(10.7259973645876,-54.1893485340865,13.8634749112255));
#30129=CARTESIAN_POINT('Ctrl Pts',(5.75838408981577,-36.7040912252866,0.));
#30130=CARTESIAN_POINT('Ctrl Pts',(5.97048868450455,-36.6735951885137,3.38941559469373));
#30131=CARTESIAN_POINT('Ctrl Pts',(6.39188323248834,-38.0987427505053,6.44317352589574));
#30132=CARTESIAN_POINT('Ctrl Pts',(6.81327778047213,-39.5238903124967,9.49693145709775));
#30133=CARTESIAN_POINT('Ctrl Pts',(7.40250983972804,-42.1163734062201,11.6101975146502));
#30134=CARTESIAN_POINT('Ctrl Pts',(7.99174189898394,-44.7088564999435,13.7234635722027));
#30135=CARTESIAN_POINT('Ctrl Pts',(8.6741167499896,-47.9491619398761,14.4776794959001));
#30136=CARTESIAN_POINT('Ctrl Pts',(9.35649160099525,-51.1894673798086,15.2318954195974));
#30137=CARTESIAN_POINT('Ctrl Pts',(10.0388664520009,-54.4297728197412,14.4776794959001));
#30138=CARTESIAN_POINT('Ctrl Pts',(4.81560839388829,-36.839641906467,0.));
#30139=CARTESIAN_POINT('Ctrl Pts',(5.02771298857707,-36.8091458696941,3.38941559469373));
#30140=CARTESIAN_POINT('Ctrl Pts',(5.44910753656085,-38.2342934316856,6.44317352589574));
#30141=CARTESIAN_POINT('Ctrl Pts',(5.87050208454464,-39.6594409936771,9.49693145709774));
#30142=CARTESIAN_POINT('Ctrl Pts',(6.45973414380055,-42.2519240874005,11.6101975146502));
#30143=CARTESIAN_POINT('Ctrl Pts',(7.04896620305647,-44.8444071811239,13.7234635722027));
#30144=CARTESIAN_POINT('Ctrl Pts',(7.73134105406212,-48.0847126210564,14.4776794959001));
#30145=CARTESIAN_POINT('Ctrl Pts',(8.41371590506776,-51.3250180609889,15.2318954195974));
#30146=CARTESIAN_POINT('Ctrl Pts',(9.09609075607344,-54.5653235009215,14.4776794959001));
#30147=CARTESIAN_POINT('Ctrl Pts',(4.19818497005484,-37.5648924257372,0.));
#30148=CARTESIAN_POINT('Ctrl Pts',(4.41028956474361,-37.5343963889644,3.24562220582792));
#30149=CARTESIAN_POINT('Ctrl Pts',(4.82280514501185,-38.8977893740386,6.16982677025168));
#30150=CARTESIAN_POINT('Ctrl Pts',(5.23532072528011,-40.2611823591128,9.09403133467541));
#30151=CARTESIAN_POINT('Ctrl Pts',(5.80855343755438,-42.7423875503303,11.1176436806954));
#30152=CARTESIAN_POINT('Ctrl Pts',(6.38178614982865,-45.2235927415478,13.1412560267153));
#30153=CARTESIAN_POINT('Ctrl Pts',(7.0442101414754,-48.325136906711,13.8634749112255));
#30154=CARTESIAN_POINT('Ctrl Pts',(7.70663413312217,-51.4266810718742,14.5856937957357));
#30155=CARTESIAN_POINT('Ctrl Pts',(8.36905812476893,-54.5282252370374,13.8634749112255));
#30156=CARTESIAN_POINT('',(5.31260798926534,-36.9500351333113,1.04083408558609E-14));
#30157=CARTESIAN_POINT('Origin',(5.56877962163311,-38.731713020801,1.04083408558608E-14));
#30158=CARTESIAN_POINT('Origin',(5.56877962163311,-38.731713020801,1.04083408558608E-14));
#30159=CARTESIAN_POINT('Ctrl Pts',(-4.33370633274479,-37.6057474666452,
1.59647061166203));
#30160=CARTESIAN_POINT('Ctrl Pts',(-4.29042532205908,-37.58837141962,1.1525915890158));
#30161=CARTESIAN_POINT('Ctrl Pts',(-4.24082283094062,-37.5585354835099,
0.635572970286848));
#30162=CARTESIAN_POINT('Ctrl Pts',(-4.0728295363398,-37.5835818541808,-1.86858636184043));
#30163=CARTESIAN_POINT('Ctrl Pts',(-4.00528018448063,-37.9619119569937,
-3.71029995868706));
#30164=CARTESIAN_POINT('Ctrl Pts',(-3.95610755721523,-39.4161093304728,
-7.16936247494803));
#30165=CARTESIAN_POINT('Ctrl Pts',(-3.98510500544276,-40.4714275735321,
-8.73699595771102));
#30166=CARTESIAN_POINT('Ctrl Pts',(-4.11161181537858,-43.1170704486883,
-11.3730256982087));
#30167=CARTESIAN_POINT('Ctrl Pts',(-4.21430601439535,-44.6849606627836,
-12.423580519233));
#30168=CARTESIAN_POINT('Ctrl Pts',(-4.45373622019712,-48.1464351665928,
-13.8529470821493));
#30169=CARTESIAN_POINT('Ctrl Pts',(-4.59667050421776,-49.9934079386698,
-14.2204718556168));
#30170=CARTESIAN_POINT('Ctrl Pts',(-4.73676521641172,-51.8536466863969,
-14.2198708430667));
#30171=CARTESIAN_POINT('Ctrl Pts',(-4.95142919224136,-36.8815114147053,
1.62964605326969));
#30172=CARTESIAN_POINT('Ctrl Pts',(-4.90850926387041,-36.8642803315616,
1.18947019887277));
#30173=CARTESIAN_POINT('Ctrl Pts',(-4.85838298962999,-36.8334013785574,
0.664243925048727));
#30174=CARTESIAN_POINT('Ctrl Pts',(-4.6898509593033,-36.8579890764814,-1.95287905135618));
#30175=CARTESIAN_POINT('Ctrl Pts',(-4.62539547708617,-37.2526110659569,
-3.87337387077168));
#30176=CARTESIAN_POINT('Ctrl Pts',(-4.58435548150261,-38.7695270469137,
-7.48792130215392));
#30177=CARTESIAN_POINT('Ctrl Pts',(-4.62052713520802,-39.8706950784986,
-9.12360836232429));
#30178=CARTESIAN_POINT('Ctrl Pts',(-4.76347923308091,-42.6325290552054,
-11.8774049927068));
#30179=CARTESIAN_POINT('Ctrl Pts',(-4.87652118893798,-44.2683416970719,
-12.9732563608828));
#30180=CARTESIAN_POINT('Ctrl Pts',(-5.13710478159844,-47.8830959478653,
-14.467685804552));
#30181=CARTESIAN_POINT('Ctrl Pts',(-5.29206142837077,-49.8087293766692,
-14.8501851004961));
#30182=CARTESIAN_POINT('Ctrl Pts',(-5.44377846349937,-51.7519872491302,
-14.8499483202528));
#30183=CARTESIAN_POINT('Ctrl Pts',(-5.89423842867615,-36.7461942621623,
1.62975523620947));
#30184=CARTESIAN_POINT('Ctrl Pts',(-5.85132433672737,-36.7289655221682,
1.18963923865732));
#30185=CARTESIAN_POINT('Ctrl Pts',(-5.8011842412917,-36.6980284414522,0.664246367120141));
#30186=CARTESIAN_POINT('Ctrl Pts',(-5.63255152129859,-36.7219158272082,
-1.95288623105315));
#30187=CARTESIAN_POINT('Ctrl Pts',(-5.56825045708737,-37.1176115175603,
-3.8731703451746));
#30188=CARTESIAN_POINT('Ctrl Pts',(-5.52703808205162,-38.6333292122955,
-7.48823335805512));
#30189=CARTESIAN_POINT('Ctrl Pts',(-5.56331547728646,-39.7352322893832,
-9.12349227714319));
#30190=CARTESIAN_POINT('Ctrl Pts',(-5.706229372011,-42.4968007058835,-11.877576477626));
#30191=CARTESIAN_POINT('Ctrl Pts',(-5.81933389107478,-44.1330482236679,
-12.9726927515199));
#30192=CARTESIAN_POINT('Ctrl Pts',(-6.0798476762211,-47.7473173225431,-14.4683433355162));
#30193=CARTESIAN_POINT('Ctrl Pts',(-6.23484434202101,-49.6732762742138,
-14.8498038985338));
#30194=CARTESIAN_POINT('Ctrl Pts',(-6.38655415380882,-51.6164365682428,
-14.8500516281495));
#30195=CARTESIAN_POINT('Ctrl Pts',(-6.69072942383177,-37.2674545852877,
1.59674356901149));
#30196=CARTESIAN_POINT('Ctrl Pts',(-6.64746300420088,-37.2500843961327,
1.1530141884774));
#30197=CARTESIAN_POINT('Ctrl Pts',(-6.5978259600943,-37.2201031407487,0.635579075465374));
#30198=CARTESIAN_POINT('Ctrl Pts',(-6.42958094132981,-37.2433987309931,
-1.86860431108287));
#30199=CARTESIAN_POINT('Ctrl Pts',(-6.36241763448362,-37.6244130859999,
-3.70979114469557));
#30200=CARTESIAN_POINT('Ctrl Pts',(-6.31281405858778,-39.0756147439297,
-7.17014261469985));
#30201=CARTESIAN_POINT('Ctrl Pts',(-6.34207586063706,-40.1327706007388,
-8.73670574475346));
#30202=CARTESIAN_POINT('Ctrl Pts',(-6.4684871627056,-42.7777495753881,-11.3734544105114));
#30203=CARTESIAN_POINT('Ctrl Pts',(-6.57133776973947,-44.3467269792784,
-12.4221714958233));
#30204=CARTESIAN_POINT('Ctrl Pts',(-6.81059345675164,-47.8069886032824,
-13.8545909095622));
#30205=CARTESIAN_POINT('Ctrl Pts',(-6.95362708074765,-49.6547753637202,
-14.2195188100007));
#30206=CARTESIAN_POINT('Ctrl Pts',(-7.09370444218534,-51.5147699841784,
-14.2201291128083));
#30207=CARTESIAN_POINT('Ctrl Pts',(-4.19818497005538,-37.5648924257372,
0.));
#30208=CARTESIAN_POINT('Ctrl Pts',(-4.0728295363398,-37.5835818541808,-1.86858636184043));
#30209=CARTESIAN_POINT('Ctrl Pts',(-4.00528018448063,-37.9619119569937,
-3.71029995868706));
#30210=CARTESIAN_POINT('Ctrl Pts',(-3.95610755721523,-39.4161093304728,
-7.16936247494803));
#30211=CARTESIAN_POINT('Ctrl Pts',(-3.98510500544276,-40.4714275735321,
-8.73699595771102));
#30212=CARTESIAN_POINT('Ctrl Pts',(-4.05479285274714,-41.9288128067802,
-10.1890856763498));
#30213=CARTESIAN_POINT('Ctrl Pts',(-4.06163542615445,-42.0659125600699,
-10.3203928635166));
#30214=CARTESIAN_POINT('Ctrl Pts',(-4.06886253049728,-42.2054617208604,
-10.4488603765996));
#30215=CARTESIAN_POINT('Ctrl Pts',(-6.55512420987408,-37.2260157227862,
1.16573417585641E-15));
#30216=CARTESIAN_POINT('Ctrl Pts',(-6.42958094132981,-37.2433987309931,
-1.86860431108287));
#30217=CARTESIAN_POINT('Ctrl Pts',(-6.36241763448362,-37.6244130859999,
-3.70979114469557));
#30218=CARTESIAN_POINT('Ctrl Pts',(-6.31281405858778,-39.0756147439297,
-7.17014261469985));
#30219=CARTESIAN_POINT('Ctrl Pts',(-6.34207586063706,-40.1327706007388,
-8.73670574475346));
#30220=CARTESIAN_POINT('Ctrl Pts',(-6.41206653251623,-41.5972271209447,
-10.1966053555719));
#30221=CARTESIAN_POINT('Ctrl Pts',(-6.4193084084792,-41.7420345975441,-10.3350231942278));
#30222=CARTESIAN_POINT('Ctrl Pts',(-6.4269788511404,-41.8895769551535,-10.4702558451001));
#30223=CARTESIAN_POINT('Ctrl Pts',(-3.0407109084869,-44.5001944306519,1.24689076028081));
#30224=CARTESIAN_POINT('Ctrl Pts',(-2.99365083345024,-44.4813012009514,
0.764254616149155));
#30225=CARTESIAN_POINT('Ctrl Pts',(-2.94950053245697,-44.4621525981,0.332948654549386));
#30226=CARTESIAN_POINT('Ctrl Pts',(-2.78663561818149,-44.4881576285441,
-0.978870002610901));
#30227=CARTESIAN_POINT('Ctrl Pts',(-2.68728492515961,-44.7004709588365,
-1.98783577089445));
#30228=CARTESIAN_POINT('Ctrl Pts',(-2.55131209325869,-45.4859946801644,
-3.80852727283077));
#30229=CARTESIAN_POINT('Ctrl Pts',(-2.50516810165338,-46.0614183982294,
-4.65544360721816));
#30230=CARTESIAN_POINT('Ctrl Pts',(-2.45787394353332,-47.4791272455671,
-6.04997283343549));
#30231=CARTESIAN_POINT('Ctrl Pts',(-2.45168870249929,-48.3324696724382,
-6.61832169902995));
#30232=CARTESIAN_POINT('Ctrl Pts',(-2.46744610983318,-50.1733013631149,
-7.36768403078693));
#30233=CARTESIAN_POINT('Ctrl Pts',(-2.4837595942785,-51.1917533012822,-7.5713864867327));
#30234=CARTESIAN_POINT('Ctrl Pts',(-2.50107414862773,-52.1751568070597,
-7.56962581969452));
#30235=CARTESIAN_POINT('Ctrl Pts',(-3.92365461890846,-42.3018453782487,
1.354893140661));
#30236=CARTESIAN_POINT('Ctrl Pts',(-3.8777644710901,-42.2834218397599,0.884255472099668));
#30237=CARTESIAN_POINT('Ctrl Pts',(-3.83192350390373,-42.2609432865998,
0.426396927819385));
#30238=CARTESIAN_POINT('Ctrl Pts',(-3.66742334693191,-42.2862930185953,
-1.25360819497148));
#30239=CARTESIAN_POINT('Ctrl Pts',(-3.57797177381454,-42.5504213117472,
-2.51960912779949));
#30240=CARTESIAN_POINT('Ctrl Pts',(-3.46871344469187,-43.5418092681725,
-4.84647586782144));
#30241=CARTESIAN_POINT('Ctrl Pts',(-3.44582654101365,-44.2657961681601,
-5.91572199046669));
#30242=CARTESIAN_POINT('Ctrl Pts',(-3.4521805883684,-46.0625411381476,-7.69376028692055));
#30243=CARTESIAN_POINT('Ctrl Pts',(-3.47964820282461,-47.136751069223,-8.41063186557174));
#30244=CARTESIAN_POINT('Ctrl Pts',(-3.56443746807183,-49.4777703293325,
-9.37059840619463));
#30245=CARTESIAN_POINT('Ctrl Pts',(-3.61985039974772,-50.7522326212068,
-9.62435378618528));
#30246=CARTESIAN_POINT('Ctrl Pts',(-3.67509457152176,-52.0063376889004,
-9.62320046360557));
#30247=CARTESIAN_POINT('Ctrl Pts',(-4.36024590432551,-39.9738746787523,
1.4729318543386));
#30248=CARTESIAN_POINT('Ctrl Pts',(-4.31563179084644,-39.9559634303431,
1.01538086897134));
#30249=CARTESIAN_POINT('Ctrl Pts',(-4.26794984367694,-39.9298762050481,
0.528580691603471));
#30250=CARTESIAN_POINT('Ctrl Pts',(-4.10171804395032,-39.9549022371289,
-1.55402875458448));
#30251=CARTESIAN_POINT('Ctrl Pts',(-4.0230044735796,-40.2750875547349,-3.10121432123278));
#30252=CARTESIAN_POINT('Ctrl Pts',(-3.9430549975307,-41.4922590552058,-5.98129145451134));
#30253=CARTESIAN_POINT('Ctrl Pts',(-3.94554026237701,-42.3782865653845,
-7.29389406576502));
#30254=CARTESIAN_POINT('Ctrl Pts',(-4.01057973632053,-44.5896542676493,
-9.49113593804167));
#30255=CARTESIAN_POINT('Ctrl Pts',(-4.0748114520217,-45.9051375482353,-10.3708286017178));
#30256=CARTESIAN_POINT('Ctrl Pts',(-4.23512580634915,-48.7933811184272,
-11.5604045561244));
#30257=CARTESIAN_POINT('Ctrl Pts',(-4.3332969012096,-50.3476002080508,-11.8694761541095));
#30258=CARTESIAN_POINT('Ctrl Pts',(-4.42999533819651,-51.8977769668582,
-11.8687142284813));
#30259=CARTESIAN_POINT('Ctrl Pts',(-4.33370633274479,-37.6057474666452,
1.59647061166203));
#30260=CARTESIAN_POINT('Ctrl Pts',(-4.29042532205909,-37.58837141962,1.15259158901579));
#30261=CARTESIAN_POINT('Ctrl Pts',(-4.24082283094062,-37.5585354835099,
0.635572970286848));
#30262=CARTESIAN_POINT('Ctrl Pts',(-4.0728295363398,-37.5835818541808,-1.86858636184043));
#30263=CARTESIAN_POINT('Ctrl Pts',(-4.00528018448063,-37.9619119569937,
-3.71029995868706));
#30264=CARTESIAN_POINT('Ctrl Pts',(-3.95610755721523,-39.4161093304728,
-7.16936247494803));
#30265=CARTESIAN_POINT('Ctrl Pts',(-3.98510500544276,-40.4714275735321,
-8.73699595771102));
#30266=CARTESIAN_POINT('Ctrl Pts',(-4.11161181537858,-43.1170704486883,
-11.3730256982087));
#30267=CARTESIAN_POINT('Ctrl Pts',(-4.21430601439535,-44.6849606627836,
-12.423580519233));
#30268=CARTESIAN_POINT('Ctrl Pts',(-4.45373622019711,-48.1464351665928,
-13.8529470821493));
#30269=CARTESIAN_POINT('Ctrl Pts',(-4.59667050421633,-49.9934079386698,
-14.2204718556168));
#30270=CARTESIAN_POINT('Ctrl Pts',(-4.73676521641171,-51.8536466863969,
-14.2198708430667));
#30271=CARTESIAN_POINT('Ctrl Pts',(-6.69072942383177,-37.2674545852877,
1.59674356901149));
#30272=CARTESIAN_POINT('Ctrl Pts',(-6.64746300420088,-37.2500843961327,
1.1530141884774));
#30273=CARTESIAN_POINT('Ctrl Pts',(-6.5978259600943,-37.2201031407487,0.635579075465374));
#30274=CARTESIAN_POINT('Ctrl Pts',(-6.42958094132981,-37.2433987309931,
-1.86860431108287));
#30275=CARTESIAN_POINT('Ctrl Pts',(-6.36241763448362,-37.6244130859999,
-3.70979114469557));
#30276=CARTESIAN_POINT('Ctrl Pts',(-6.31281405858778,-39.0756147439297,
-7.17014261469985));
#30277=CARTESIAN_POINT('Ctrl Pts',(-6.34207586063706,-40.1327706007388,
-8.73670574475346));
#30278=CARTESIAN_POINT('Ctrl Pts',(-6.4684871627056,-42.7777495753881,-11.3734544105114));
#30279=CARTESIAN_POINT('Ctrl Pts',(-6.57133776973947,-44.3467269792784,
-12.4221714958233));
#30280=CARTESIAN_POINT('Ctrl Pts',(-6.81059345675164,-47.8069886032824,
-13.8545909095622));
#30281=CARTESIAN_POINT('Ctrl Pts',(-6.95362708074765,-49.6547753637202,
-14.2195188100007));
#30282=CARTESIAN_POINT('Ctrl Pts',(-7.09370444218534,-51.5147699841784,
-14.2201291128083));
#30283=CARTESIAN_POINT('Ctrl Pts',(-7.33134203123344,-39.5474466673499,
1.4732759250127));
#30284=CARTESIAN_POINT('Ctrl Pts',(-7.28674631020376,-39.5295428029629,
1.01591356787765));
#30285=CARTESIAN_POINT('Ctrl Pts',(-7.2390208079874,-39.5032723984918,0.528588387358482));
#30286=CARTESIAN_POINT('Ctrl Pts',(-7.07247170263556,-39.5260915209495,
-1.55405138012636));
#30287=CARTESIAN_POINT('Ctrl Pts',(-6.99424475322478,-39.8496604164817,
-3.10057294640376));
#30288=CARTESIAN_POINT('Ctrl Pts',(-6.91375205390094,-41.0630557304083,
-5.98227484334893));
#30289=CARTESIAN_POINT('Ctrl Pts',(-6.91657054442394,-41.9513996061453,
-7.29352824389797));
#30290=CARTESIAN_POINT('Ctrl Pts',(-6.98148962792371,-44.161930442516,-9.4916763423596));
#30291=CARTESIAN_POINT('Ctrl Pts',(-7.04591850047786,-45.4787841574446,
-10.3690524867544));
#30292=CARTESIAN_POINT('Ctrl Pts',(-7.20601286879719,-48.3654988573867,
-11.5624766483598));
#30293=CARTESIAN_POINT('Ctrl Pts',(-7.30430498990994,-49.9207450076481,
-11.8682745705925));
#30294=CARTESIAN_POINT('Ctrl Pts',(-7.40098575043892,-51.4706130322883,
-11.8690397849987));
#30295=CARTESIAN_POINT('Ctrl Pts',(-8.40509445805894,-41.6586445536368,
1.35541211815635));
#30296=CARTESIAN_POINT('Ctrl Pts',(-8.35923205241047,-41.6402321527941,
0.885058966163931));
#30297=CARTESIAN_POINT('Ctrl Pts',(-8.31332538916123,-41.6174773021374,
0.426408535677771));
#30298=CARTESIAN_POINT('Ctrl Pts',(-8.14834662563531,-41.6394982516602,
-1.25364232210855));
#30299=CARTESIAN_POINT('Ctrl Pts',(-8.05962904511716,-41.9087301497685,
-2.51864171288232));
#30300=CARTESIAN_POINT('Ctrl Pts',(-7.94955134754164,-42.8944223117487,
-4.8479591580715));
#30301=CARTESIAN_POINT('Ctrl Pts',(-7.92716706335529,-43.6219030915812,
-5.91517020465636));
#30302=CARTESIAN_POINT('Ctrl Pts',(-7.93333952031304,-45.4173857785723,
-7.69457540340655));
#30303=CARTESIAN_POINT('Ctrl Pts',(-7.96110451544491,-46.4936627982893,
-8.40795287033041));
#30304=CARTESIAN_POINT('Ctrl Pts',(-8.04556196575892,-48.8323759936388,
-9.37372383745879));
#30305=CARTESIAN_POINT('Ctrl Pts',(-8.10114839964434,-50.1083893187776,
-9.62254086009649));
#30306=CARTESIAN_POINT('Ctrl Pts',(-8.15637495641919,-51.3620268377999,
-9.62369151535369));
#30307=CARTESIAN_POINT('Ctrl Pts',(-9.87072183560191,-43.5199138025265,
1.2476817163332));
#30308=CARTESIAN_POINT('Ctrl Pts',(-9.82370404146966,-43.5010375473475,
0.765479194283311));
#30309=CARTESIAN_POINT('Ctrl Pts',(-9.77945361532658,-43.4814678488086,
0.332966345693859));
#30310=CARTESIAN_POINT('Ctrl Pts',(-9.61585927298705,-43.5023995944572,
-0.978922014626564));
#30311=CARTESIAN_POINT('Ctrl Pts',(-9.51762723326553,-43.7224911564908,
-1.98636136653616));
#30312=CARTESIAN_POINT('Ctrl Pts',(-9.38040562961129,-44.4993341100839,
-3.81078790534053));
#30313=CARTESIAN_POINT('Ctrl Pts',(-9.33502766337921,-45.0800827322847,
-4.654602649119));
#30314=CARTESIAN_POINT('Ctrl Pts',(-9.28745674947336,-46.4958677767967,
-6.05121512491338));
#30315=CARTESIAN_POINT('Ctrl Pts',(-9.28172473627183,-47.3523605835685,
-6.61423873297828));
#30316=CARTESIAN_POINT('Ctrl Pts',(-9.29697643568735,-49.1896776789186,
-7.37244739488559));
#30317=CARTESIAN_POINT('Ctrl Pts',(-9.31353425505142,-50.2104967200013,
-7.56862230187139));
#30318=CARTESIAN_POINT('Ctrl Pts',(-9.33084205690732,-51.1931844250964,
-7.57037421505981));
#30319=CARTESIAN_POINT('Ctrl Pts',(-9.64145132693333,-36.6062244663075,
1.59647068126627));
#30320=CARTESIAN_POINT('Ctrl Pts',(-9.59613798295645,-36.5951848118862,
1.15259163659385));
#30321=CARTESIAN_POINT('Ctrl Pts',(-9.54279427444346,-36.5727117312865,
0.635573001860467));
#30322=CARTESIAN_POINT('Ctrl Pts',(-9.38007537753151,-36.6214111051535,
-1.86858636179946));
#30323=CARTESIAN_POINT('Ctrl Pts',(-9.36705556804196,-37.0055036281524,
-3.71029995871102));
#30324=CARTESIAN_POINT('Ctrl Pts',(-9.52533731124922,-38.4518973636108,
-7.1693624749242));
#30325=CARTESIAN_POINT('Ctrl Pts',(-9.70422705227032,-39.4923472214852,
-8.73699595767225));
#30326=CARTESIAN_POINT('Ctrl Pts',(-10.2059604433558,-42.0930574706308,
-11.3730256982475));
#30327=CARTESIAN_POINT('Ctrl Pts',(-10.5307434056497,-43.6303739147856,
-12.4235805192274));
#30328=CARTESIAN_POINT('Ctrl Pts',(-11.2603557414205,-47.0225411281053,
-13.8529470821549));
#30329=CARTESIAN_POINT('Ctrl Pts',(-11.6646867919259,-48.8303727109964,
-14.2204718556692));
#30330=CARTESIAN_POINT('Ctrl Pts',(-12.0680951184148,-50.6517393542017,
-14.2198708430667));
#30331=CARTESIAN_POINT('Ctrl Pts',(-10.1498171217995,-35.8014489642672,
1.62964612287391));
#30332=CARTESIAN_POINT('Ctrl Pts',(-10.1048818153719,-35.7905014108337,
1.18947024664515));
#30333=CARTESIAN_POINT('Ctrl Pts',(-10.0508712182972,-35.7670704718592,
0.664243958044528));
#30334=CARTESIAN_POINT('Ctrl Pts',(-9.88755379327951,-35.8153925117011,
-1.95287905130714));
#30335=CARTESIAN_POINT('Ctrl Pts',(-9.87991493950544,-36.2151707898814,
-3.87337387079805));
#30336=CARTESIAN_POINT('Ctrl Pts',(-10.0551723244117,-37.7224873536628,
-7.48792130212771));
#30337=CARTESIAN_POINT('Ctrl Pts',(-10.2476883530651,-38.8072993194331,
-9.12360836229508));
#30338=CARTESIAN_POINT('Ctrl Pts',(-10.7822353606272,-41.5206776037571,
-11.8774049927361));
#30339=CARTESIAN_POINT('Ctrl Pts',(-11.1269271238186,-43.1237524839686,
-12.9732563608868));
#30340=CARTESIAN_POINT('Ctrl Pts',(-11.8992915178841,-46.6646288366181,
-14.467685804548));
#30341=CARTESIAN_POINT('Ctrl Pts',(-12.3267171394702,-48.5486094635654,
-14.8501851005342));
#30342=CARTESIAN_POINT('Ctrl Pts',(-12.7534443437025,-50.4504961875092,
-14.8499483202528));
#30343=CARTESIAN_POINT('Ctrl Pts',(-11.0637722809463,-35.5333334012202,
1.6297553058137));
#30344=CARTESIAN_POINT('Ctrl Pts',(-11.0188430850024,-35.5223873364666,
1.18963928643661));
#30345=CARTESIAN_POINT('Ctrl Pts',(-10.9648105349745,-35.4989008284127,
0.664246400116173));
#30346=CARTESIAN_POINT('Ctrl Pts',(-10.8012937803563,-35.5465440138953,
-1.95288623100444));
#30347=CARTESIAN_POINT('Ctrl Pts',(-10.7939605763972,-35.9473630882332,
-3.87317034520098));
#30348=CARTESIAN_POINT('Ctrl Pts',(-10.9688768025169,-37.4535180947868,
-7.48823335802893));
#30349=CARTESIAN_POINT('Ctrl Pts',(-11.1616021042806,-38.539042575736,-9.12349227712832));
#30350=CARTESIAN_POINT('Ctrl Pts',(-11.6960735043977,-41.252163439798,-11.8775764776409));
#30351=CARTESIAN_POINT('Ctrl Pts',(-12.0408890832862,-42.8556598658169,
-12.9726927515287));
#30352=CARTESIAN_POINT('Ctrl Pts',(-12.8131153360569,-46.3960659393468,
-14.4683433355075));
#30353=CARTESIAN_POINT('Ctrl Pts',(-13.2406268960767,-48.2803630804993,
-14.8498038985338));
#30354=CARTESIAN_POINT('Ctrl Pts',(-13.6673330636265,-50.1821542472109,
-14.8500516281495));
#30355=CARTESIAN_POINT('Ctrl Pts',(-11.9263392248003,-35.9359355586899,
1.59674363861575));
#30356=CARTESIAN_POINT('Ctrl Pts',(-11.8810411570285,-35.9248996259805,
1.15301423607239));
#30357=CARTESIAN_POINT('Ctrl Pts',(-11.8276425661371,-35.9022876226733,
0.635579107039569));
#30358=CARTESIAN_POINT('Ctrl Pts',(-11.6644253452223,-35.9492898606295,
-1.8686043110427));
#30359=CARTESIAN_POINT('Ctrl Pts',(-11.6521696602714,-36.3359843740415,
-3.70979114471714));
#30360=CARTESIAN_POINT('Ctrl Pts',(-11.8095985065123,-37.7794742164111,
-7.17014261467843));
#30361=CARTESIAN_POINT('Ctrl Pts',(-11.989011430306,-38.8217053622615,-8.73670574475537));
#30362=CARTESIAN_POINT('Ctrl Pts',(-12.490555802785,-41.4217720607139,-11.3734544105096));
#30363=CARTESIAN_POINT('Ctrl Pts',(-12.8156483043172,-42.960142369416,-12.4221714958418));
#30364=CARTESIAN_POINT('Ctrl Pts',(-13.5449152868542,-46.3511338849175,
-13.8545909095439));
#30365=CARTESIAN_POINT('Ctrl Pts',(-13.9494605088193,-48.1597570333837,
-14.2195188100007));
#30366=CARTESIAN_POINT('Ctrl Pts',(-14.352816918225,-49.980884503456,-14.2201291128083));
#30367=CARTESIAN_POINT('Ctrl Pts',(-9.50149509066523,-36.5850719698905,
3.46944695195361E-15));
#30368=CARTESIAN_POINT('Ctrl Pts',(-9.3800753775315,-36.6214111051535,-1.86858636179946));
#30369=CARTESIAN_POINT('Ctrl Pts',(-9.36705556804075,-37.0055036281572,
-3.71029995871102));
#30370=CARTESIAN_POINT('Ctrl Pts',(-9.52533731125042,-38.451897363606,-7.1693624749242));
#30371=CARTESIAN_POINT('Ctrl Pts',(-9.70422705227151,-39.49234722149,-8.73699595767225));
#30372=CARTESIAN_POINT('Ctrl Pts',(-9.98061312163023,-40.9249807596884,
-10.1890856763525));
#30373=CARTESIAN_POINT('Ctrl Pts',(-10.0068973767291,-41.0597112354399,
-10.3203928635211));
#30374=CARTESIAN_POINT('Ctrl Pts',(-10.0339108358238,-41.1968114627984,
-10.4488603766053));
#30375=CARTESIAN_POINT('Ctrl Pts',(-11.7862169042733,-35.914217116421,1.16573417585641E-15));
#30376=CARTESIAN_POINT('Ctrl Pts',(-11.6644253452223,-35.9492898606295,
-1.8686043110427));
#30377=CARTESIAN_POINT('Ctrl Pts',(-11.6521696602714,-36.3359843740415,
-3.70979114471714));
#30378=CARTESIAN_POINT('Ctrl Pts',(-11.8095985065123,-37.7794742164111,
-7.17014261467843));
#30379=CARTESIAN_POINT('Ctrl Pts',(-11.989011430306,-38.8217053622615,-8.73670574475537));
#30380=CARTESIAN_POINT('Ctrl Pts',(-12.2667035909955,-40.2612951155294,
-10.1966053555699));
#30381=CARTESIAN_POINT('Ctrl Pts',(-12.2944800077231,-40.4035980344053,
-10.335023194224));
#30382=CARTESIAN_POINT('Ctrl Pts',(-12.3230698431047,-40.5485470057454,
-10.4702558450949));
#30383=CARTESIAN_POINT('Ctrl Pts',(-9.34279883641492,-43.6145083358836,
1.24689082988532));
#30384=CARTESIAN_POINT('Ctrl Pts',(-9.29352897570114,-43.6025047584042,
0.764254661714488));
#30385=CARTESIAN_POINT('Ctrl Pts',(-9.24710292814764,-43.589834301908,0.332948671112318));
#30386=CARTESIAN_POINT('Ctrl Pts',(-9.08959664352382,-43.638752733162,-0.978870002656774));
#30387=CARTESIAN_POINT('Ctrl Pts',(-9.02147253461304,-43.8630440977154,
-1.98783577088714));
#30388=CARTESIAN_POINT('Ctrl Pts',(-8.99867539144458,-44.6599232717705,
-3.80852727283793));
#30389=CARTESIAN_POINT('Ctrl Pts',(-9.03489241259897,-45.2360569808236,
-4.65544360716999));
#30390=CARTESIAN_POINT('Ctrl Pts',(-9.18984064597521,-46.6460662566439,
-6.04997283348356));
#30391=CARTESIAN_POINT('Ctrl Pts',(-9.30516165135279,-47.491603139623,-6.61832169899598));
#30392=CARTESIAN_POINT('Ctrl Pts',(-9.58273633530685,-49.3114553051195,
-7.36768403082088));
#30393=CARTESIAN_POINT('Ctrl Pts',(-9.74382459483866,-50.3172192201122,
-7.57138648681379));
#30394=CARTESIAN_POINT('Ctrl Pts',(-9.90091582292576,-51.2881489781561,
-7.56962581969457));
#30395=CARTESIAN_POINT('Ctrl Pts',(-9.90389776310323,-41.3128793157233,
1.35489321026542));
#30396=CARTESIAN_POINT('Ctrl Pts',(-9.8558527655289,-41.301174150679,0.884255518290098));
#30397=CARTESIAN_POINT('Ctrl Pts',(-9.80727935893592,-41.2854482448494,
0.426396949017563));
#30398=CARTESIAN_POINT('Ctrl Pts',(-9.648061217345,-41.3339507669544,-1.2536081949907));
#30399=CARTESIAN_POINT('Ctrl Pts',(-9.59710950760655,-41.6081209010958,
-2.51960912779942));
#30400=CARTESIAN_POINT('Ctrl Pts',(-9.63005248742419,-42.6049670390315,
-4.84647586782148));
#30401=CARTESIAN_POINT('Ctrl Pts',(-9.71043261803931,-43.3248419422994,
-5.91572199043044));
#30402=CARTESIAN_POINT('Ctrl Pts',(-9.97242546011253,-45.1023943639113,
-7.69376028695677));
#30403=CARTESIAN_POINT('Ctrl Pts',(-10.1524895065122,-46.161761337687,-8.41063186554247));
#30404=CARTESIAN_POINT('Ctrl Pts',(-10.5695775166737,-48.4668856266306,
-9.37059840622391));
#30405=CARTESIAN_POINT('Ctrl Pts',(-10.8058013195489,-49.7204896475899,
-9.62435378622341));
#30406=CARTESIAN_POINT('Ctrl Pts',(-11.0389609452142,-50.9539676685889,
-9.62320046360561));
#30407=CARTESIAN_POINT('Ctrl Pts',(-10.0047404051437,-38.9464705831155,
1.47293192394294));
#30408=CARTESIAN_POINT('Ctrl Pts',(-9.95803136026999,-38.9350908951825,
1.01538091584094));
#30409=CARTESIAN_POINT('Ctrl Pts',(-9.90712214456661,-38.91605504704,0.52858071787014));
#30410=CARTESIAN_POINT('Ctrl Pts',(-9.74614391855838,-38.9644836024863,
-1.55402875457437));
#30411=CARTESIAN_POINT('Ctrl Pts',(-9.71379866052385,-39.2926120042886,
-3.10121432124472));
#30412=CARTESIAN_POINT('Ctrl Pts',(-9.80788452010917,-40.5087724506344,
-5.98129145449945));
#30413=CARTESIAN_POINT('Ctrl Pts',(-9.93643935033497,-41.3854277882792,
-7.29389406573111));
#30414=CARTESIAN_POINT('Ctrl Pts',(-10.3155272531674,-43.5650308735925,
-9.49113593807561));
#30415=CARTESIAN_POINT('Ctrl Pts',(-10.5663179729168,-44.8579833049588,
-10.3708286017124));
#30416=CARTESIAN_POINT('Ctrl Pts',(-11.1360404748697,-47.6940136086793,
-11.5604045561299));
#30417=CARTESIAN_POINT('Ctrl Pts',(-11.454400767937,-49.2184417854932,-11.8694761541429));
#30418=CARTESIAN_POINT('Ctrl Pts',(-11.770728108961,-50.7390783576438,-11.8687142284813));
#30419=CARTESIAN_POINT('Ctrl Pts',(-9.64145132693333,-36.6062244663075,
1.59647068126627));
#30420=CARTESIAN_POINT('Ctrl Pts',(-9.59613798295645,-36.5951848118862,
1.15259163659386));
#30421=CARTESIAN_POINT('Ctrl Pts',(-9.54279427444346,-36.5727117312865,
0.635573001860467));
#30422=CARTESIAN_POINT('Ctrl Pts',(-9.3800753775315,-36.6214111051535,-1.86858636179946));
#30423=CARTESIAN_POINT('Ctrl Pts',(-9.36705556804075,-37.0055036281572,
-3.71029995871102));
#30424=CARTESIAN_POINT('Ctrl Pts',(-9.52533731125042,-38.451897363606,-7.1693624749242));
#30425=CARTESIAN_POINT('Ctrl Pts',(-9.70422705227151,-39.49234722149,-8.73699595767225));
#30426=CARTESIAN_POINT('Ctrl Pts',(-10.2059604433546,-42.093057470626,-11.3730256982475));
#30427=CARTESIAN_POINT('Ctrl Pts',(-10.5307434056497,-43.6303739147808,
-12.4235805192275));
#30428=CARTESIAN_POINT('Ctrl Pts',(-11.2603557414205,-47.0225411281101,
-13.8529470821549));
#30429=CARTESIAN_POINT('Ctrl Pts',(-11.6646867919251,-48.830372710993,-14.2204718556692));
#30430=CARTESIAN_POINT('Ctrl Pts',(-12.0680951184148,-50.6517393542017,
-14.2198708430668));
#30431=CARTESIAN_POINT('Ctrl Pts',(-11.9263392248003,-35.9359355586899,
1.59674363861575));
#30432=CARTESIAN_POINT('Ctrl Pts',(-11.8810411570285,-35.9248996259805,
1.15301423607239));
#30433=CARTESIAN_POINT('Ctrl Pts',(-11.8276425661371,-35.9022876226733,
0.635579107039569));
#30434=CARTESIAN_POINT('Ctrl Pts',(-11.6644253452223,-35.9492898606295,
-1.8686043110427));
#30435=CARTESIAN_POINT('Ctrl Pts',(-11.6521696602714,-36.3359843740415,
-3.70979114471595));
#30436=CARTESIAN_POINT('Ctrl Pts',(-11.8095985065123,-37.7794742164111,
-7.17014261467964));
#30437=CARTESIAN_POINT('Ctrl Pts',(-11.9890114303072,-38.8217053622615,
-8.73670574475537));
#30438=CARTESIAN_POINT('Ctrl Pts',(-12.4905558027838,-41.4217720607139,
-11.3734544105096));
#30439=CARTESIAN_POINT('Ctrl Pts',(-12.8156483043172,-42.9601423694208,
-12.422171495837));
#30440=CARTESIAN_POINT('Ctrl Pts',(-13.5449152868542,-46.3511338849126,
-13.8545909095487));
#30441=CARTESIAN_POINT('Ctrl Pts',(-13.94946050882,-48.1597570333872,-14.2195188100007));
#30442=CARTESIAN_POINT('Ctrl Pts',(-14.352816918225,-49.980884503456,-14.2201291128083));
#30443=CARTESIAN_POINT('Ctrl Pts',(-12.8849080239687,-38.1015519292156,
1.47327599461705));
#30444=CARTESIAN_POINT('Ctrl Pts',(-12.8382182351927,-38.0901769326068,
1.01591361476925));
#30445=CARTESIAN_POINT('Ctrl Pts',(-12.7872398386582,-38.0709659683553,
0.528588413625886));
#30446=CARTESIAN_POINT('Ctrl Pts',(-12.6256334607596,-38.1172552346473,
-1.55405138011728));
#30447=CARTESIAN_POINT('Ctrl Pts',(-12.5942514039184,-38.4486635210123,
-3.10057294641332));
#30448=CARTESIAN_POINT('Ctrl Pts',(-12.687262162083,-39.6611635256934,-5.98227484333945));
#30449=CARTESIAN_POINT('Ctrl Pts',(-12.8164764794026,-40.5400642286176,
-7.29352824390953));
#30450=CARTESIAN_POINT('Ctrl Pts',(-13.1953261187877,-42.718856099577,-9.49167634234811));
#30451=CARTESIAN_POINT('Ctrl Pts',(-13.4465070217463,-44.0131369578427,
-10.3690524867682));
#30452=CARTESIAN_POINT('Ctrl Pts',(-14.0157941959057,-46.8476852602797,
-11.5624766483461));
#30453=CARTESIAN_POINT('Ctrl Pts',(-14.3344204493215,-48.3731128199053,
-11.8682745705877));
#30454=CARTESIAN_POINT('Ctrl Pts',(-14.6506863563567,-49.8934463159786,
-11.8690397849987));
#30455=CARTESIAN_POINT('Ctrl Pts',(-14.248185985062,-40.038449962147,1.3554121877608));
#30456=CARTESIAN_POINT('Ctrl Pts',(-14.2001700323384,-40.026751873255,0.885059012386578));
#30457=CARTESIAN_POINT('Ctrl Pts',(-14.1514922771424,-40.0107618317946,
0.426408556877058));
#30458=CARTESIAN_POINT('Ctrl Pts',(-13.9913266653939,-40.056037566468,-1.25364232212933));
#30459=CARTESIAN_POINT('Ctrl Pts',(-13.9418277959601,-40.3351549001415,
-2.51864171287987));
#30460=CARTESIAN_POINT('Ctrl Pts',(-13.973149151259,-41.3264798268969,-4.84795915807396));
#30461=CARTESIAN_POINT('Ctrl Pts',(-14.0545240163445,-42.0497415170713,
-5.91517020468713));
#30462=CARTESIAN_POINT('Ctrl Pts',(-14.3161574747883,-43.8260703470498,
-7.69457540337582));
#30463=CARTESIAN_POINT('Ctrl Pts',(-14.4968100523213,-44.8874410477277,
-8.40795287034433));
#30464=CARTESIAN_POINT('Ctrl Pts',(-14.9132414377173,-47.1903299665294,
-9.37372383744494));
#30465=CARTESIAN_POINT('Ctrl Pts',(-15.1498577118458,-48.4454445415184,
-9.62254086005834));
#30466=CARTESIAN_POINT('Ctrl Pts',(-15.382933362694,-49.6784622796992,-9.62369151535366));
#30467=CARTESIAN_POINT('Ctrl Pts',(-15.9637816213004,-41.6721936506077,
1.24768178593774));
#30468=CARTESIAN_POINT('Ctrl Pts',(-15.9145560268668,-41.6602008576382,
0.765479239898045));
#30469=CARTESIAN_POINT('Ctrl Pts',(-15.8679709451303,-41.6471278409701,
0.332966362258481));
#30470=CARTESIAN_POINT('Ctrl Pts',(-15.7090206532774,-41.6911284346186,
-0.978922014674807));
#30471=CARTESIAN_POINT('Ctrl Pts',(-15.6431107691496,-41.9229596586886,
-1.98636136651691));
#30472=CARTESIAN_POINT('Ctrl Pts',(-15.617842162883,-42.7114241414764,-3.81078790535973));
#30473=CARTESIAN_POINT('Ctrl Pts',(-15.6555752252088,-43.2927195379191,
-4.65460264917615));
#30474=CARTESIAN_POINT('Ctrl Pts',(-15.8099757341484,-44.7008639791348,
-6.05121512485625));
#30475=CARTESIAN_POINT('Ctrl Pts',(-15.9261936999267,-45.5494546745318,
-6.61423873299709));
#30476=CARTESIAN_POINT('Ctrl Pts',(-16.2027676442761,-47.3658999879523,
-7.37244739486684));
#30477=CARTESIAN_POINT('Ctrl Pts',(-16.3644346256248,-48.3739721396825,
-7.56862230182844));
#30478=CARTESIAN_POINT('Ctrl Pts',(-16.5214173008833,-49.3441943438431,
-7.57037421505976));
#30479=CARTESIAN_POINT('Ctrl Pts',(-14.7529241788868,-34.861504297702,1.596470776103));
#30480=CARTESIAN_POINT('Ctrl Pts',(-14.7414705295769,-34.8603993451942,
1.48695587718827));
#30481=CARTESIAN_POINT('Ctrl Pts',(-14.7300185573963,-34.8592949433733,
1.37746402257862));
#30482=CARTESIAN_POINT('Ctrl Pts',(-14.6812048800309,-34.8545841497113,
0.910698635110844));
#30483=CARTESIAN_POINT('Ctrl Pts',(-14.641323265537,-34.8466226370302,0.486448413024372));
#30484=CARTESIAN_POINT('Ctrl Pts',(-14.4963699338215,-34.913734033555,-1.86858636180693));
#30485=CARTESIAN_POINT('Ctrl Pts',(-14.5381447125539,-35.2957699605276,
-3.71029995869199));
#30486=CARTESIAN_POINT('Ctrl Pts',(-14.9006586664723,-36.7049156525157,
-7.1693624749433));
#30487=CARTESIAN_POINT('Ctrl Pts',(-15.2257990212174,-37.7093165664316,
-8.73699595772034));
#30488=CARTESIAN_POINT('Ctrl Pts',(-16.092545148042,-40.2121512289274,-11.3730256981995));
#30489=CARTESIAN_POINT('Ctrl Pts',(-16.6328052292483,-41.6875985735071,
-12.423580519199));
#30490=CARTESIAN_POINT('Ctrl Pts',(-17.8377468920061,-44.9414037540446,
-13.8529470821835));
#30491=CARTESIAN_POINT('Ctrl Pts',(-18.4952436947709,-46.6732919100445,
-14.2204718557262));
#30492=CARTESIAN_POINT('Ctrl Pts',(-19.1537534053194,-48.4187086763094,
-14.2198708430667));
#30493=CARTESIAN_POINT('Ctrl Pts',(-15.1415840475452,-33.992572254002,1.62964621771061));
#30494=CARTESIAN_POINT('Ctrl Pts',(-15.1301302752945,-33.9914672896339,
1.52013014329387));
#30495=CARTESIAN_POINT('Ctrl Pts',(-15.1186784705795,-33.9903629797955,
1.41064104114018));
#30496=CARTESIAN_POINT('Ctrl Pts',(-15.069864603448,-33.9856518446506,0.943868932653774));
#30497=CARTESIAN_POINT('Ctrl Pts',(-15.0295355352549,-33.9768575865842,
0.508392298453448));
#30498=CARTESIAN_POINT('Ctrl Pts',(-14.8839745452192,-34.043697838521,-1.95287905130899));
#30499=CARTESIAN_POINT('Ctrl Pts',(-14.9333078250241,-34.4404940724738,
-3.87337387078378));
#30500=CARTESIAN_POINT('Ctrl Pts',(-15.3212948555725,-35.9075266005405,
-7.48792130214209));
#30501=CARTESIAN_POINT('Ctrl Pts',(-15.6662361882241,-36.9538988571314,
-9.12360836231688));
#30502=CARTESIAN_POINT('Ctrl Pts',(-16.5814962693528,-39.5635848921456,
-11.8774049927144));
#30503=CARTESIAN_POINT('Ctrl Pts',(-17.1508209097751,-41.1012880289292,
-12.9732563608727));
#30504=CARTESIAN_POINT('Ctrl Pts',(-18.4192429936803,-44.4962044519299,
-14.4676858045622));
#30505=CARTESIAN_POINT('Ctrl Pts',(-19.110436436978,-46.3001798643399,-14.8501851005532));
#30506=CARTESIAN_POINT('Ctrl Pts',(-19.8034868749641,-48.1219785107276,
-14.8499483202528));
#30507=CARTESIAN_POINT('Ctrl Pts',(-16.0080796379928,-33.5971163401331,
1.62975540065039));
#30508=CARTESIAN_POINT('Ctrl Pts',(-15.9966258648996,-33.5960113756864,
1.52023931818491));
#30509=CARTESIAN_POINT('Ctrl Pts',(-15.9851740659136,-33.5949070766362,
1.41075023429581));
#30510=CARTESIAN_POINT('Ctrl Pts',(-15.9363601779558,-33.5901958958465,
0.94397808226918));
#30511=CARTESIAN_POINT('Ctrl Pts',(-15.8959902453789,-33.5813120719023,
0.508394167540087));
#30512=CARTESIAN_POINT('Ctrl Pts',(-15.7501528462318,-33.6475470722586,
-1.95288623100104));
#30513=CARTESIAN_POINT('Ctrl Pts',(-15.7999367855235,-34.0453300100855,
-3.87317034519272));
#30514=CARTESIAN_POINT('Ctrl Pts',(-16.1874208229716,-35.5112613558745,
-7.48823335803731));
#30515=CARTESIAN_POINT('Ctrl Pts',(-16.5326707001234,-36.5583090926344,
-9.12349227711425));
#30516=CARTESIAN_POINT('Ctrl Pts',(-17.4478193086362,-39.1677510875279,
-11.8775764776552));
#30517=CARTESIAN_POINT('Ctrl Pts',(-18.0173264967234,-40.7058538586162,
-12.9726927515386));
#30518=CARTESIAN_POINT('Ctrl Pts',(-19.2855449177196,-44.1003244488304,
-14.4683433354976));
#30519=CARTESIAN_POINT('Ctrl Pts',(-19.9768684693679,-45.9046009234682,
-14.8498038985385));
#30520=CARTESIAN_POINT('Ctrl Pts',(-20.6698844856026,-47.7263079790887,
-14.8500516281495));
#30521=CARTESIAN_POINT('Ctrl Pts',(-16.9191631550059,-33.8728645130297,
1.59674373345244));
#30522=CARTESIAN_POINT('Ctrl Pts',(-16.9077095035903,-33.8717595603218,
1.48722881441586));
#30523=CARTESIAN_POINT('Ctrl Pts',(-16.8962575457316,-33.8706551854743,
1.37773700546765));
#30524=CARTESIAN_POINT('Ctrl Pts',(-16.8474438163005,-33.8659442777035,
0.910971509149462));
#30525=CARTESIAN_POINT('Ctrl Pts',(-16.8074600408464,-33.8577588503261,
0.486453085740971));
#30526=CARTESIAN_POINT('Ctrl Pts',(-16.6618156863547,-33.9233571178964,
-1.86860431103707));
#30527=CARTESIAN_POINT('Ctrl Pts',(-16.7047171138001,-34.3078598045567,
-3.70979114471372));
#30528=CARTESIAN_POINT('Ctrl Pts',(-17.0659735849724,-35.7142525408506,
-7.17014261468198));
#30529=CARTESIAN_POINT('Ctrl Pts',(-17.3918853009681,-36.7203421551653,
-8.73670574471736));
#30530=CARTESIAN_POINT('Ctrl Pts',(-18.2583527462481,-39.222566717407,-11.3734544105477));
#30531=CARTESIAN_POINT('Ctrl Pts',(-18.7990691966108,-40.699013147727,-12.422171495866));
#30532=CARTESIAN_POINT('Ctrl Pts',(-20.0035017021128,-43.9517037462935,
-13.8545909095196));
#30533=CARTESIAN_POINT('Ctrl Pts',(-20.6613231478877,-45.6843449310519,
-14.2195188099912));
#30534=CARTESIAN_POINT('Ctrl Pts',(-21.3197474319156,-47.429532347212,-14.2201291128083));
#30535=CARTESIAN_POINT('Ctrl Pts',(-14.6113821712783,-34.8604849513723,
1.04083408558608E-14));
#30536=CARTESIAN_POINT('Ctrl Pts',(-14.4963699338215,-34.913734033555,-1.86858636180693));
#30537=CARTESIAN_POINT('Ctrl Pts',(-14.5381447125539,-35.2957699605276,
-3.71029995869199));
#30538=CARTESIAN_POINT('Ctrl Pts',(-14.9006586664723,-36.7049156525157,
-7.1693624749433));
#30539=CARTESIAN_POINT('Ctrl Pts',(-15.2257990212174,-37.7093165664316,
-8.73699595772034));
#30540=CARTESIAN_POINT('Ctrl Pts',(-15.7032568890462,-39.0880341222414,
-10.1890856763482));
#30541=CARTESIAN_POINT('Ctrl Pts',(-15.7484477541819,-39.2176525965103,
-10.3203928635132));
#30542=CARTESIAN_POINT('Ctrl Pts',(-15.7946976518867,-39.3495129251816,
-10.4488603765943));
#30543=CARTESIAN_POINT('Ctrl Pts',(-16.7773762106051,-33.871308617679,-4.87765735985715E-9));
#30544=CARTESIAN_POINT('Ctrl Pts',(-16.6618156862293,-33.923357118505,-1.8686043142631));
#30545=CARTESIAN_POINT('Ctrl Pts',(-16.7047171137966,-34.307859805123,-3.70979114625147));
#30546=CARTESIAN_POINT('Ctrl Pts',(-16.8853453492638,-35.0110561726707,
-5.43996687972834));
#30547=CARTESIAN_POINT('Ctrl Pts',(-17.0659735848888,-35.7142525408324,
-7.17014261471563));
#30548=CARTESIAN_POINT('Ctrl Pts',(-17.3918853009222,-36.7203421551587,
-8.73670574474088));
#30549=CARTESIAN_POINT('Ctrl Pts',(-17.8251190235969,-37.9714544362847,
-10.0550800776385));
#30550=CARTESIAN_POINT('Ctrl Pts',(-17.871625938579,-38.1057592455506,-10.1966053555787));
#30551=CARTESIAN_POINT('Ctrl Pts',(-17.9193714483085,-38.2426607296452,
-10.335023194235));
#30552=CARTESIAN_POINT('Ctrl Pts',(-17.9682986697938,-38.3820655716606,
-10.4702558451073));
#30553=CARTESIAN_POINT('Ctrl Pts',(-15.4546943255721,-41.8409566234848,
1.2468909247223));
#30554=CARTESIAN_POINT('Ctrl Pts',(-15.4432419692989,-41.8398517957208,
1.13738838925849));
#30555=CARTESIAN_POINT('Ctrl Pts',(-15.431788261189,-41.8387464827955,1.02786758221435));
#30556=CARTESIAN_POINT('Ctrl Pts',(-15.3829764714434,-41.8340390406225,
0.561172897424349));
#30557=CARTESIAN_POINT('Ctrl Pts',(-15.3475914064577,-41.8343710194632,
0.254828874437198));
#30558=CARTESIAN_POINT('Ctrl Pts',(-15.2075196936098,-41.9009886759871,
-0.978870002694615));
#30559=CARTESIAN_POINT('Ctrl Pts',(-15.1720089791053,-42.132692149374,-1.98783577086012));
#30560=CARTESIAN_POINT('Ctrl Pts',(-15.2628516086326,-42.9247046141117,
-3.8085272728648));
#30561=CARTESIAN_POINT('Ctrl Pts',(-15.3806923682557,-43.4898198932175,
-4.65544360728965));
#30562=CARTESIAN_POINT('Ctrl Pts',(-15.7347286944236,-44.8634258749694,
-6.04997283336378));
#30563=CARTESIAN_POINT('Ctrl Pts',(-15.969208342928,-45.6839445214029,-6.61832169892421));
#30564=CARTESIAN_POINT('Ctrl Pts',(-16.5029496832502,-47.4457702195624,
-7.36768403089269));
#30565=CARTESIAN_POINT('Ctrl Pts',(-16.8055334255118,-48.4183716585711,
-7.57138648693262));
#30566=CARTESIAN_POINT('Ctrl Pts',(-17.0992034029526,-49.3570623388654,
-7.5696258196945));
#30567=CARTESIAN_POINT('Ctrl Pts',(-15.6825261124555,-39.4829021650677,
1.35489330510232));
#30568=CARTESIAN_POINT('Ctrl Pts',(-15.6710733564743,-39.4817972987419,
1.24538694781336));
#30569=CARTESIAN_POINT('Ctrl Pts',(-15.6596201873397,-39.4806922726919,
1.1358750903288));
#30570=CARTESIAN_POINT('Ctrl Pts',(-15.6108078040333,-39.4759837722005,
0.669158551001817));
#30571=CARTESIAN_POINT('Ctrl Pts',(-15.5740132903121,-39.473708863974,0.326351368866041));
#30572=CARTESIAN_POINT('Ctrl Pts',(-15.4322923841624,-39.540168475028,-1.25360819501648));
#30573=CARTESIAN_POINT('Ctrl Pts',(-15.4208777676315,-39.8187991368524,
-2.51960912778186));
#30574=CARTESIAN_POINT('Ctrl Pts',(-15.5953514322613,-40.8008105435132,
-4.84647586783895));
#30575=CARTESIAN_POINT('Ctrl Pts',(-15.7773622894425,-41.5019188729544,
-5.91572199050949));
#30576=CARTESIAN_POINT('Ctrl Pts',(-16.2896605076835,-43.2240929050568,
-7.69376028687766));
#30577=CARTESIAN_POINT('Ctrl Pts',(-16.6186554012328,-44.2470512648665,
-8.41063186549471));
#30578=CARTESIAN_POINT('Ctrl Pts',(-17.359551447157,-46.4693548995032,-9.3705984062717));
#30579=CARTESIAN_POINT('Ctrl Pts',(-17.7717772858575,-47.6765808868262,
-9.624353786328));
#30580=CARTESIAN_POINT('Ctrl Pts',(-18.1781059077967,-48.8643218056539,
-9.62320046360555));
#30581=CARTESIAN_POINT('Ctrl Pts',(-15.4455672457337,-37.1262286569852,
1.47293201877975));
#30582=CARTESIAN_POINT('Ctrl Pts',(-15.4341140531475,-37.1251237485394,
1.36342148686276));
#30583=CARTESIAN_POINT('Ctrl Pts',(-15.4226614701642,-37.1240190301311,
1.25391940542253));
#30584=CARTESIAN_POINT('Ctrl Pts',(-15.3738484494875,-37.1193093979792,
0.787178992714135));
#30585=CARTESIAN_POINT('Ctrl Pts',(-15.3355356362474,-37.1142341193451,
0.40455974469035));
#30586=CARTESIAN_POINT('Ctrl Pts',(-15.1921664085198,-37.1808604460558,
-1.55402875458989));
#30587=CARTESIAN_POINT('Ctrl Pts',(-15.206847919016,-37.510252183997,-3.10121432122704));
#30588=CARTESIAN_POINT('Ctrl Pts',(-15.4730537974676,-38.7006440565956,
-5.98129145451713));
#30589=CARTESIAN_POINT('Ctrl Pts',(-15.725061187509,-39.5500810470411,-7.29389406578391));
#30590=CARTESIAN_POINT('Ctrl Pts',(-16.4104803825999,-41.6535490822059,
-9.49113593802281));
#30591=CARTESIAN_POINT('Ctrl Pts',(-16.8427247306082,-42.8976498813535,
-10.370828601679));
#30592=CARTESIAN_POINT('Ctrl Pts',(-17.8102574730307,-45.6237335200178,
-11.5604045561632));
#30593=CARTESIAN_POINT('Ctrl Pts',(-18.3423260668094,-47.0873378224416,
-11.8694761541809));
#30594=CARTESIAN_POINT('Ctrl Pts',(-18.8718427994038,-48.5474784324871,
-11.8687142284813));
#30595=CARTESIAN_POINT('Ctrl Pts',(-14.7529241788868,-34.861504297702,1.596470776103));
#30596=CARTESIAN_POINT('Ctrl Pts',(-14.7414705295769,-34.8603993451942,
1.48695587718829));
#30597=CARTESIAN_POINT('Ctrl Pts',(-14.7300185573963,-34.8592949433733,
1.37746402257859));
#30598=CARTESIAN_POINT('Ctrl Pts',(-14.6812048800309,-34.8545841497113,
0.910698635110924));
#30599=CARTESIAN_POINT('Ctrl Pts',(-14.641323265537,-34.8466226370302,0.486448413024372));
#30600=CARTESIAN_POINT('Ctrl Pts',(-14.4963699338215,-34.913734033555,-1.86858636180693));
#30601=CARTESIAN_POINT('Ctrl Pts',(-14.5381447125539,-35.2957699605276,
-3.71029995869199));
#30602=CARTESIAN_POINT('Ctrl Pts',(-14.9006586664723,-36.7049156525157,
-7.1693624749433));
#30603=CARTESIAN_POINT('Ctrl Pts',(-15.2257990212174,-37.7093165664316,
-8.73699595772034));
#30604=CARTESIAN_POINT('Ctrl Pts',(-16.092545148042,-40.2121512289274,-11.3730256981995));
#30605=CARTESIAN_POINT('Ctrl Pts',(-16.6328052292483,-41.6875985735071,
-12.423580519199));
#30606=CARTESIAN_POINT('Ctrl Pts',(-17.8377468920061,-44.9414037540446,
-13.8529470821835));
#30607=CARTESIAN_POINT('Ctrl Pts',(-18.495243694773,-46.6732919100438,-14.2204718557215));
#30608=CARTESIAN_POINT('Ctrl Pts',(-19.1537534053194,-48.4187086763094,
-14.2198708430667));
#30609=CARTESIAN_POINT('Ctrl Pts',(-16.9191631550059,-33.8728645130297,
1.59674373345244));
#30610=CARTESIAN_POINT('Ctrl Pts',(-16.9077095035903,-33.8717595603218,
1.48722881441586));
#30611=CARTESIAN_POINT('Ctrl Pts',(-16.8962575457316,-33.8706551854743,
1.37773700546765));
#30612=CARTESIAN_POINT('Ctrl Pts',(-16.8474438163005,-33.8659442777035,
0.910971509149462));
#30613=CARTESIAN_POINT('Ctrl Pts',(-16.8074600408464,-33.8577588503261,
0.486453085740971));
#30614=CARTESIAN_POINT('Ctrl Pts',(-16.6618156863547,-33.9233571178964,
-1.86860431103707));
#30615=CARTESIAN_POINT('Ctrl Pts',(-16.7047171138049,-34.3078598045567,
-3.70979114471372));
#30616=CARTESIAN_POINT('Ctrl Pts',(-17.0659735849676,-35.7142525408506,
-7.17014261468198));
#30617=CARTESIAN_POINT('Ctrl Pts',(-17.3918853009681,-36.7203421551653,
-8.73670574471736));
#30618=CARTESIAN_POINT('Ctrl Pts',(-18.2583527462481,-39.222566717407,-11.3734544105478));
#30619=CARTESIAN_POINT('Ctrl Pts',(-18.7990691966084,-40.6990131477271,
-12.422171495866));
#30620=CARTESIAN_POINT('Ctrl Pts',(-20.0035017021152,-43.9517037462935,
-13.8545909095196));
#30621=CARTESIAN_POINT('Ctrl Pts',(-20.6613231478854,-45.6843449310521,
-14.2195188099864));
#30622=CARTESIAN_POINT('Ctrl Pts',(-21.3197474319156,-47.429532347212,-14.2201291128083));
#30623=CARTESIAN_POINT('Ctrl Pts',(-18.176174449474,-35.8800194678371,1.4732760894538));
#30624=CARTESIAN_POINT('Ctrl Pts',(-18.1647212542338,-35.8789145591356,
1.36376553217263));
#30625=CARTESIAN_POINT('Ctrl Pts',(-18.1532686893032,-35.8778098747321,
1.25426350829));
#30626=CARTESIAN_POINT('Ctrl Pts',(-18.1044556029969,-35.8731000987406,
0.787522958372421));
#30627=CARTESIAN_POINT('Ctrl Pts',(-18.0660140128963,-35.867742569121,0.404565634785468));
#30628=CARTESIAN_POINT('Ctrl Pts',(-17.9217737308695,-35.9324615528111,
-1.55405138011628));
#30629=CARTESIAN_POINT('Ctrl Pts',(-17.9378754148266,-36.2649627130452,
-3.10057294641604));
#30630=CARTESIAN_POINT('Ctrl Pts',(-18.2024961997114,-37.4518844049459,
-5.98227484333679));
#30631=CARTESIAN_POINT('Ctrl Pts',(-18.4554759130357,-38.3034500513459,
-7.29352824386188));
#30632=CARTESIAN_POINT('Ctrl Pts',(-19.1405438219426,-40.4061490373993,
-9.49167634239581));
#30633=CARTESIAN_POINT('Ctrl Pts',(-19.5733634365382,-41.6515092131651,
-10.3690524868116));
#30634=CARTESIAN_POINT('Ctrl Pts',(-20.5402543714365,-44.3761878888615,
-11.5624766483027));
#30635=CARTESIAN_POINT('Ctrl Pts',(-21.0727284454552,-45.8407435516478,
-11.8682745705592));
#30636=CARTESIAN_POINT('Ctrl Pts',(-21.6021412371496,-47.3005929134933,
-11.8690397849987));
#30637=CARTESIAN_POINT('Ctrl Pts',(-19.8012255369163,-37.6031879890151,
1.35541228259761));
#30638=CARTESIAN_POINT('Ctrl Pts',(-19.7897727769317,-37.6020831223045,
1.24590588705071));
#30639=CARTESIAN_POINT('Ctrl Pts',(-19.7783196350267,-37.6009781475451,
1.13639411638292));
#30640=CARTESIAN_POINT('Ctrl Pts',(-19.7295071527293,-37.5962694300918,
0.66967737009692));
#30641=CARTESIAN_POINT('Ctrl Pts',(-19.6925183989934,-37.5935687898309,
0.326360253165228));
#30642=CARTESIAN_POINT('Ctrl Pts',(-19.5494836419035,-37.6571514683751,
-1.25364232213017));
#30643=CARTESIAN_POINT('Ctrl Pts',(-19.5402111377933,-37.9404722137081,
-2.51864171289113));
#30644=CARTESIAN_POINT('Ctrl Pts',(-19.7122939334867,-38.9172493885169,
-4.84795915806269));
#30645=CARTESIAN_POINT('Ctrl Pts',(-19.895771390238,-39.6215684668484,-5.91517020461549));
#30646=CARTESIAN_POINT('Ctrl Pts',(-20.4075397474893,-41.3425825070781,
-7.69457540344745));
#30647=CARTESIAN_POINT('Ctrl Pts',(-20.7374023418787,-42.3674404421053,
-8.40795287041159));
#30648=CARTESIAN_POINT('Ctrl Pts',(-21.4773303202423,-44.5876249069951,
-9.37372383737758));
#30649=CARTESIAN_POINT('Ctrl Pts',(-21.8901596096273,-45.7962902185076,
-9.62254086002985));
#30650=CARTESIAN_POINT('Ctrl Pts',(-22.296339606421,-46.9835874904388,-9.6236915153537));
#30651=CARTESIAN_POINT('Ctrl Pts',(-21.7318648520657,-38.9761478068777,
1.24768188077458));
#30652=CARTESIAN_POINT('Ctrl Pts',(-21.7204124896908,-38.9750429785251,
1.13817928700318));
#30653=CARTESIAN_POINT('Ctrl Pts',(-21.7089588230812,-38.9739377437724,
1.02865861227348));
#30654=CARTESIAN_POINT('Ctrl Pts',(-21.6601468824655,-38.9692299709343,
0.561963612064401));
#30655=CARTESIAN_POINT('Ctrl Pts',(-21.6244657828418,-38.9689131059758,
0.254842414697181));
#30656=CARTESIAN_POINT('Ctrl Pts',(-21.4823916742034,-39.0311461269472,
-0.97892201467465));
#30657=CARTESIAN_POINT('Ctrl Pts',(-21.450145680808,-39.2699975980215,-1.98636136654028));
#30658=CARTESIAN_POINT('Ctrl Pts',(-21.5373444678282,-40.054032746971,-3.8107879053363));
#30659=CARTESIAN_POINT('Ctrl Pts',(-21.6574204222689,-40.6240414198954,
-4.65460264907096));
#30660=CARTESIAN_POINT('Ctrl Pts',(-22.0106492052165,-41.9958794972643,
-6.05121512496137));
#30661=CARTESIAN_POINT('Ctrl Pts',(-22.2464512872363,-42.8192932220575,
-6.61423873309305));
#30662=CARTESIAN_POINT('Ctrl Pts',(-22.7787172285155,-44.5778891652519,
-7.37244739477071));
#30663=CARTESIAN_POINT('Ctrl Pts',(-23.0822022983039,-45.5526929856245,
-7.56862230174279));
#30664=CARTESIAN_POINT('Ctrl Pts',(-23.3756641324465,-46.490698762655,-7.57037421505983));
#30665=CARTESIAN_POINT('Ctrl Pts',(-19.5640700378121,-32.4071044310925,
1.59647086199751));
#30666=CARTESIAN_POINT('Ctrl Pts',(-19.5174819665884,-32.4092782047833,
1.15259176011195));
#30667=CARTESIAN_POINT('Ctrl Pts',(-19.4599676462981,-32.4027440988463,
0.635573083870355));
#30668=CARTESIAN_POINT('Ctrl Pts',(-19.3175602025801,-32.4953140196741,
-1.86858636177345));
#30669=CARTESIAN_POINT('Ctrl Pts',(-19.4132791553027,-32.8675162010731,
-3.7102999586904));
#30670=CARTESIAN_POINT('Ctrl Pts',(-19.9726455811605,-34.2107277069995,
-7.16936247494489));
#30671=CARTESIAN_POINT('Ctrl Pts',(-20.4374176294115,-35.1586329709599,
-8.73699595768469));
#30672=CARTESIAN_POINT('Ctrl Pts',(-21.6515320408422,-37.5126415502852,
-11.3730256982353));
#30673=CARTESIAN_POINT('Ctrl Pts',(-22.3962711037445,-38.8961839421996,
-12.423580519285));
#30674=CARTESIAN_POINT('Ctrl Pts',(-24.0520129553695,-41.9453890000367,
-13.8529470820976));
#30675=CARTESIAN_POINT('Ctrl Pts',(-24.9492907716223,-43.5660774805332,
-14.220471855655));
#30676=CARTESIAN_POINT('Ctrl Pts',(-25.8494965077556,-45.2000127177928,
-14.2198708430668));
#30677=CARTESIAN_POINT('Ctrl Pts',(-19.8251119861392,-31.4917047963494,
1.62964630360508));
#30678=CARTESIAN_POINT('Ctrl Pts',(-19.7789125871832,-31.4938604347953,
1.18947037066722));
#30679=CARTESIAN_POINT('Ctrl Pts',(-19.7204885320786,-31.4865951547092,
0.664244043748249));
#30680=CARTESIAN_POINT('Ctrl Pts',(-19.5774004975844,-31.5789716510579,
-1.95287905126329));
#30681=CARTESIAN_POINT('Ctrl Pts',(-19.6827016273729,-31.9647082139024,
-3.8733738707834));
#30682=CARTESIAN_POINT('Ctrl Pts',(-20.2755200063962,-33.3615921546183,
-7.48792130214242));
#30683=CARTESIAN_POINT('Ctrl Pts',(-20.7658646319509,-34.348223580536,-9.1236083623051));
#30684=CARTESIAN_POINT('Ctrl Pts',(-22.0432057314562,-36.8010916838934,
-11.8774049927262));
#30685=CARTESIAN_POINT('Ctrl Pts',(-22.8255734412877,-38.242119875778,-12.9732563609107));
#30686=CARTESIAN_POINT('Ctrl Pts',(-24.5642317984401,-41.421965661227,-14.4676858045243));
#30687=CARTESIAN_POINT('Ctrl Pts',(-25.5051223583005,-43.1092121218843,
-14.8501851005247));
#30688=CARTESIAN_POINT('Ctrl Pts',(-26.4503875219921,-44.8138361237938,
-14.8499483202528));
#30689=CARTESIAN_POINT('Ctrl Pts',(-20.6265086564331,-30.9769588736644,
1.62975548654484));
#30690=CARTESIAN_POINT('Ctrl Pts',(-20.5803155398565,-30.9791142189677,
1.18963941047879));
#30691=CARTESIAN_POINT('Ctrl Pts',(-20.5218547654337,-30.9718018056147,
0.664246485816634));
#30692=CARTESIAN_POINT('Ctrl Pts',(-20.3783842202168,-31.0635831036134,
-1.95288623095009));
#30693=CARTESIAN_POINT('Ctrl Pts',(-20.4842718449966,-31.4502321915287,
-3.8731703451935));
#30694=CARTESIAN_POINT('Ctrl Pts',(-21.0764356360931,-32.8460977418056,
-7.48823335803642));
#30695=CARTESIAN_POINT('Ctrl Pts',(-21.5671817964434,-33.8333538619715,
-9.12349227713591));
#30696=CARTESIAN_POINT('Ctrl Pts',(-22.8443778274613,-36.285996273475,-11.8775764776334));
#30697=CARTESIAN_POINT('Ctrl Pts',(-23.6269831007732,-37.727394052712,-12.9726927515238));
#30698=CARTESIAN_POINT('Ctrl Pts',(-25.36537641937,-40.9068275275002,-14.4683433355123));
#30699=CARTESIAN_POINT('Ctrl Pts',(-26.3064386089277,-42.5943534697001,
-14.8498038985575));
#30700=CARTESIAN_POINT('Ctrl Pts',(-27.2516566664768,-44.2988917118188,
-14.8500516281494));
#30701=CARTESIAN_POINT('Ctrl Pts',(-21.5675617135469,-31.1202396243798,
1.59674381934691));
#30702=CARTESIAN_POINT('Ctrl Pts',(-21.5209893482663,-31.122412665213,1.15301435964159));
#30703=CARTESIAN_POINT('Ctrl Pts',(-21.4633832296834,-31.1157607261045,
0.635579189041325));
#30704=CARTESIAN_POINT('Ctrl Pts',(-21.3200195091683,-31.2068426510793,
-1.86860431099046));
#30705=CARTESIAN_POINT('Ctrl Pts',(-21.4172046993669,-31.5813261451459,
-3.70979114471806));
#30706=CARTESIAN_POINT('Ctrl Pts',(-21.9749346553982,-32.9219916749607,
-7.17014261467751));
#30707=CARTESIAN_POINT('Ctrl Pts',(-22.4407105406403,-33.8714586745724,
-8.7367057447581));
#30708=CARTESIAN_POINT('Ctrl Pts',(-23.6544622808573,-36.2249030242154,
-11.3734544105068));
#30709=CARTESIAN_POINT('Ctrl Pts',(-24.399795252463,-37.6093693845273,-12.4221714958032));
#30710=CARTESIAN_POINT('Ctrl Pts',(-26.0548745076895,-40.6575436657269,
-13.8545909095822));
#30711=CARTESIAN_POINT('Ctrl Pts',(-26.9525808297975,-42.2789313088314,
-14.2195188100006));
#30712=CARTESIAN_POINT('Ctrl Pts',(-27.8526693689673,-43.9126516878552,
-14.2201291128082));
#30713=CARTESIAN_POINT('Ctrl Pts',(-19.4238236466309,-32.4262389885812,
0.));
#30714=CARTESIAN_POINT('Ctrl Pts',(-19.3175602025801,-32.4953140196741,
-1.86858636177345));
#30715=CARTESIAN_POINT('Ctrl Pts',(-19.4132791553027,-32.8675162010731,
-3.7102999586904));
#30716=CARTESIAN_POINT('Ctrl Pts',(-19.9726455811605,-34.2107277069995,
-7.1693624749449));
#30717=CARTESIAN_POINT('Ctrl Pts',(-20.4374176294115,-35.1586329709647,
-8.73699595768469));
#30718=CARTESIAN_POINT('Ctrl Pts',(-21.1062276306812,-36.4553678306274,
-10.1890856763522));
#30719=CARTESIAN_POINT('Ctrl Pts',(-21.1694051501835,-36.5772356450483,
-10.3203928635213));
#30720=CARTESIAN_POINT('Ctrl Pts',(-21.2339499719768,-36.7011717789787,
-10.4488603766065));
#30721=CARTESIAN_POINT('Ctrl Pts',(-21.4269965203142,-31.1388779521429,
1.60982338570648E-15));
#30722=CARTESIAN_POINT('Ctrl Pts',(-21.3200195091683,-31.2068426510793,
-1.86860431099046));
#30723=CARTESIAN_POINT('Ctrl Pts',(-21.4172046993669,-31.5813261451459,
-3.70979114471806));
#30724=CARTESIAN_POINT('Ctrl Pts',(-21.9749346553982,-32.9219916749607,
-7.17014261467751));
#30725=CARTESIAN_POINT('Ctrl Pts',(-22.4407105406403,-33.8714586745724,
-8.7367057447581));
#30726=CARTESIAN_POINT('Ctrl Pts',(-23.1127335196157,-35.1745000052626,
-10.1966053555706));
#30727=CARTESIAN_POINT('Ctrl Pts',(-23.1794761614793,-35.3032131351437,
-10.335023194225));
#30728=CARTESIAN_POINT('Ctrl Pts',(-23.2477447519538,-35.4342359672548,
-10.4702558450959));
#30729=CARTESIAN_POINT('Ctrl Pts',(-21.2519768052526,-39.2156436908076,
1.24689101061708));
#30730=CARTESIAN_POINT('Ctrl Pts',(-21.2013209149673,-39.2180072667115,
0.76425478003098));
#30731=CARTESIAN_POINT('Ctrl Pts',(-21.1532057605615,-39.2189297793998,
0.33294871411375));
#30732=CARTESIAN_POINT('Ctrl Pts',(-21.0158614972049,-39.3102413216955,
-0.978870002760954));
#30733=CARTESIAN_POINT('Ctrl Pts',(-21.0136870732031,-39.5446400894738,
-1.98783577086067));
#30734=CARTESIAN_POINT('Ctrl Pts',(-21.2163201815384,-40.3156627551842,
-3.80852727286451));
#30735=CARTESIAN_POINT('Ctrl Pts',(-21.4133857818753,-40.8582554869495,
-4.65544360718471));
#30736=CARTESIAN_POINT('Ctrl Pts',(-21.9593030415369,-42.1674955178372,
-6.04997283346917));
#30737=CARTESIAN_POINT('Ctrl Pts',(-22.3081680037039,-42.9462925343122,
-6.61832169913048));
#30738=CARTESIAN_POINT('Ctrl Pts',(-23.0872105665505,-44.6142260746701,
-7.36768403068697));
#30739=CARTESIAN_POINT('Ctrl Pts',(-23.5251300588757,-45.5338656769775,
-7.57138648679969));
#30740=CARTESIAN_POINT('Ctrl Pts',(-23.9494005117258,-46.4212082443697,
-7.56962581969477));
#30741=CARTESIAN_POINT('Ctrl Pts',(-21.1419034541628,-36.8491669828397,
1.35489339099702));
#30742=CARTESIAN_POINT('Ctrl Pts',(-21.0925068841194,-36.8514717995378,
0.884255638223336));
#30743=CARTESIAN_POINT('Ctrl Pts',(-21.0414705341173,-36.8500676110308,
0.426397004062705));
#30744=CARTESIAN_POINT('Ctrl Pts',(-20.9023665809131,-36.9414623772438,
-1.2536081950493));
#30745=CARTESIAN_POINT('Ctrl Pts',(-20.9307214264281,-37.2188814500692,
-2.51960912778008));
#30746=CARTESIAN_POINT('Ctrl Pts',(-21.2431739952357,-38.1660672051982,
-4.84647586784088));
#30747=CARTESIAN_POINT('Ctrl Pts',(-21.5231103629228,-38.8341364170915,
-5.91572199044039));
#30748=CARTESIAN_POINT('Ctrl Pts',(-22.275285042685,-40.4658735625616,-7.69376028694706));
#30749=CARTESIAN_POINT('Ctrl Pts',(-22.7465133961109,-41.4315988261922,
-8.41063186564328));
#30750=CARTESIAN_POINT('Ctrl Pts',(-23.7961349711067,-43.5258421132357,
-9.37059840612348));
#30751=CARTESIAN_POINT('Ctrl Pts',(-24.3759711161681,-44.662114427047,-9.62435378624255));
#30752=CARTESIAN_POINT('Ctrl Pts',(-24.947197055425,-45.7799392638235,-9.62320046360572));
#30753=CARTESIAN_POINT('Ctrl Pts',(-20.5719668778721,-34.5502037758217,
1.47293210467435));
#30754=CARTESIAN_POINT('Ctrl Pts',(-20.5239438427388,-34.5524445041313,
1.01538103753069));
#30755=CARTESIAN_POINT('Ctrl Pts',(-20.4697337816482,-34.5485225227141,
0.52858078608683));
#30756=CARTESIAN_POINT('Ctrl Pts',(-20.3289202010286,-34.6403421915222,
-1.55402875458901));
#30757=CARTESIAN_POINT('Ctrl Pts',(-20.3903296068154,-34.9642917998438,
-3.10121432122654));
#30758=CARTESIAN_POINT('Ctrl Pts',(-20.8232363201018,-36.1046821530358,
-5.9812914545177));
#30759=CARTESIAN_POINT('Ctrl Pts',(-21.1935661261691,-36.9096087088301,
-7.29389406574109));
#30760=CARTESIAN_POINT('Ctrl Pts',(-22.1713634554283,-38.8941211502923,
-9.49113593806581));
#30761=CARTESIAN_POINT('Ctrl Pts',(-22.7762621832877,-40.0640440126673,
-10.3708286017747));
#30762=CARTESIAN_POINT('Ctrl Pts',(-24.1219089894863,-42.6246857849748,
-11.5604045560678));
#30763=CARTESIAN_POINT('Ctrl Pts',(-24.8568545017496,-43.9976714499935,
-11.8694761541382));
#30764=CARTESIAN_POINT('Ctrl Pts',(-25.5887811923514,-45.3675918458117,
-11.8687142284814));
#30765=CARTESIAN_POINT('Ctrl Pts',(-19.5640700378121,-32.4071044310925,
1.59647086199751));
#30766=CARTESIAN_POINT('Ctrl Pts',(-19.5174819665884,-32.4092782047833,
1.15259176011195));
#30767=CARTESIAN_POINT('Ctrl Pts',(-19.4599676462981,-32.4027440988463,
0.635573083870355));
#30768=CARTESIAN_POINT('Ctrl Pts',(-19.3175602025801,-32.4953140196741,
-1.86858636177345));
#30769=CARTESIAN_POINT('Ctrl Pts',(-19.4132791553027,-32.8675162010731,
-3.7102999586904));
#30770=CARTESIAN_POINT('Ctrl Pts',(-19.9726455811605,-34.2107277069995,
-7.1693624749449));
#30771=CARTESIAN_POINT('Ctrl Pts',(-20.4374176294115,-35.1586329709647,
-8.73699595768469));
#30772=CARTESIAN_POINT('Ctrl Pts',(-21.6515320408422,-37.5126415502804,
-11.3730256982353));
#30773=CARTESIAN_POINT('Ctrl Pts',(-22.3962711037445,-38.8961839422044,
-12.423580519285));
#30774=CARTESIAN_POINT('Ctrl Pts',(-24.0520129553695,-41.9453890000319,
-13.8529470820976));
#30775=CARTESIAN_POINT('Ctrl Pts',(-24.9492907716337,-43.5660774805306,
-14.2204718556692));
#30776=CARTESIAN_POINT('Ctrl Pts',(-25.8494965077556,-45.2000127177928,
-14.2198708430668));
#30777=CARTESIAN_POINT('Ctrl Pts',(-21.5675617135469,-31.1202396243798,
1.59674381934691));
#30778=CARTESIAN_POINT('Ctrl Pts',(-21.5209893482663,-31.122412665213,1.15301435964159));
#30779=CARTESIAN_POINT('Ctrl Pts',(-21.4633832296834,-31.1157607261045,
0.635579189041325));
#30780=CARTESIAN_POINT('Ctrl Pts',(-21.3200195091683,-31.2068426510793,
-1.86860431099046));
#30781=CARTESIAN_POINT('Ctrl Pts',(-21.4172046993669,-31.5813261451459,
-3.70979114471806));
#30782=CARTESIAN_POINT('Ctrl Pts',(-21.9749346553982,-32.9219916749607,
-7.17014261467751));
#30783=CARTESIAN_POINT('Ctrl Pts',(-22.4407105406403,-33.8714586745724,
-8.7367057447581));
#30784=CARTESIAN_POINT('Ctrl Pts',(-23.6544622808573,-36.2249030242154,
-11.3734544105068));
#30785=CARTESIAN_POINT('Ctrl Pts',(-24.399795252463,-37.6093693845273,-12.4221714958032));
#30786=CARTESIAN_POINT('Ctrl Pts',(-26.0548745076895,-40.6575436657269,
-13.8545909095822));
#30787=CARTESIAN_POINT('Ctrl Pts',(-26.9525808297975,-42.2789313088314,
-14.2195188100006));
#30788=CARTESIAN_POINT('Ctrl Pts',(-27.8526693689673,-43.9126516878552,
-14.2201291128082));
#30789=CARTESIAN_POINT('Ctrl Pts',(-23.0974263782807,-32.9280732767459,
1.47327617534837));
#30790=CARTESIAN_POINT('Ctrl Pts',(-23.0494231409448,-32.9303130812748,
1.01591373652303));
#30791=CARTESIAN_POINT('Ctrl Pts',(-22.9950973654386,-32.9262425677154,
0.528588481832317));
#30792=CARTESIAN_POINT('Ctrl Pts',(-22.8530783701147,-33.0161865744793,
-1.55405138009885));
#30793=CARTESIAN_POINT('Ctrl Pts',(-22.9163360108656,-33.3430118437433,
-3.10057294642025));
#30794=CARTESIAN_POINT('Ctrl Pts',(-23.3471799063629,-34.4801929200436,
-5.98227484333246));
#30795=CARTESIAN_POINT('Ctrl Pts',(-23.7187750781387,-35.2870880890182,
-7.29352824390976));
#30796=CARTESIAN_POINT('Ctrl Pts',(-24.6961152497918,-37.270889302571,-9.4916763423477));
#30797=CARTESIAN_POINT('Ctrl Pts',(-25.3017626168359,-38.4419768539591,
-10.3690524867152));
#30798=CARTESIAN_POINT('Ctrl Pts',(-26.6465742010127,-41.0013193023666,
-11.5624766483988));
#30799=CARTESIAN_POINT('Ctrl Pts',(-27.3820564590795,-42.3751889385656,
-11.8682745706114));
#30800=CARTESIAN_POINT('Ctrl Pts',(-28.1138388177854,-43.7448358429353,
-11.8690397849985));
#30801=CARTESIAN_POINT('Ctrl Pts',(-24.9511692381919,-34.4024335442871,
1.35541236849225));
#30802=CARTESIAN_POINT('Ctrl Pts',(-24.9018025300712,-34.4047369675988,
0.885059132416527));
#30803=CARTESIAN_POINT('Ctrl Pts',(-24.8505916427358,-34.4031087412849,
0.42640861190673));
#30804=CARTESIAN_POINT('Ctrl Pts',(-24.7096695075361,-34.4916743608874,
-1.25364232213804));
#30805=CARTESIAN_POINT('Ctrl Pts',(-24.7408121301759,-34.7734309242996,
-2.51864171290121));
#30806=CARTESIAN_POINT('Ctrl Pts',(-25.0501532567909,-35.715775980658,-4.84795915805251));
#30807=CARTESIAN_POINT('Ctrl Pts',(-25.3319982333056,-36.3868145416348,
-5.91517020468245));
#30808=CARTESIAN_POINT('Ctrl Pts',(-26.0834833614037,-38.0174789095995,
-7.6945754033802));
#30809=CARTESIAN_POINT('Ctrl Pts',(-26.5558409214639,-38.9849609268016,
-8.40795287026731));
#30810=CARTESIAN_POINT('Ctrl Pts',(-27.604202692975,-41.0772443843362,-9.37372383752152));
#30811=CARTESIAN_POINT('Ctrl Pts',(-28.184840983779,-42.2148554923143,-9.62254086005825));
#30812=CARTESIAN_POINT('Ctrl Pts',(-28.7558566730951,-43.3322623493511,
-9.62369151535353));
#30813=CARTESIAN_POINT('Ctrl Pts',(-27.0575499832998,-35.4866599889491,
1.24768196666929));
#30814=CARTESIAN_POINT('Ctrl Pts',(-27.0069396045581,-35.489021441235,0.765479358362176));
#30815=CARTESIAN_POINT('Ctrl Pts',(-26.9585584437084,-35.489602505485,0.332966405236331));
#30816=CARTESIAN_POINT('Ctrl Pts',(-26.8184431506468,-35.5766022410826,
-0.978922014702958));
#30817=CARTESIAN_POINT('Ctrl Pts',(-26.8205174834931,-35.8176116315986,
-1.98636136655743));
#30818=CARTESIAN_POINT('Ctrl Pts',(-27.0184085480051,-36.5812567520118,
-3.81078790531902));
#30819=CARTESIAN_POINT('Ctrl Pts',(-27.2183829945192,-37.1283749683008,
-4.65460264917133));
#30820=CARTESIAN_POINT('Ctrl Pts',(-27.7632493317924,-38.4359800152694,
-6.05121512486059));
#30821=CARTESIAN_POINT('Ctrl Pts',(-28.1138352796158,-39.217454440471,-6.61423873286722));
#30822=CARTESIAN_POINT('Ctrl Pts',(-28.8909578185681,-40.8824010709202,
-7.37244739499603));
#30823=CARTESIAN_POINT('Ctrl Pts',(-29.3300828959493,-41.8040923655683,
-7.56862230180927));
#30824=CARTESIAN_POINT('Ctrl Pts',(-29.7540498521217,-42.6907866227636,
-7.57037421505956));
#30825=CARTESIAN_POINT('Ctrl Pts',(-23.9769478445537,-29.2929893708798,
1.59647090706393));
#30826=CARTESIAN_POINT('Ctrl Pts',(-23.9311433315013,-29.3017711927832,
1.15259179089974));
#30827=CARTESIAN_POINT('Ctrl Pts',(-23.8732845217115,-29.3034887354924,
0.635573104333306));
#30828=CARTESIAN_POINT('Ctrl Pts',(-23.7455006526456,-29.4153831213402,
-1.86858636180619));
#30829=CARTESIAN_POINT('Ctrl Pts',(-23.8932152178165,-29.7701745937408,
-3.71029995872295));
#30830=CARTESIAN_POINT('Ctrl Pts',(-24.6380470280763,-31.0201080010757,
-7.16936247491227));
#30831=CARTESIAN_POINT('Ctrl Pts',(-25.2329893514594,-31.8922209971881,
-8.73699595769179));
#30832=CARTESIAN_POINT('Ctrl Pts',(-26.769756179009,-34.049482667342,-11.373025698228));
#30833=CARTESIAN_POINT('Ctrl Pts',(-27.7038134837039,-35.3129551734355,
-12.4235805192132));
#30834=CARTESIAN_POINT('Ctrl Pts',(-29.7766493956151,-38.0954870862277,
-13.8529470821691));
#30835=CARTESIAN_POINT('Ctrl Pts',(-30.8954422365109,-39.5719833475712,
-14.2204718557357));
#30836=CARTESIAN_POINT('Ctrl Pts',(-32.0190184050856,-41.0611748464153,
-14.2198708430667));
#30837=CARTESIAN_POINT('Ctrl Pts',(-24.1050578112643,-28.3497570418624,
1.62964634867152));
#30838=CARTESIAN_POINT('Ctrl Pts',(-24.0596354334582,-28.3584655992883,
1.18947040157868));
#30839=CARTESIAN_POINT('Ctrl Pts',(-24.0007720917085,-28.3595888789067,
0.664244065133585));
#30840=CARTESIAN_POINT('Ctrl Pts',(-23.8722870320922,-28.4713886672088,
-1.95287905129543));
#30841=CARTESIAN_POINT('Ctrl Pts',(-24.0314123849458,-28.8382130746034,
-3.87337387080275));
#30842=CARTESIAN_POINT('Ctrl Pts',(-24.8169940395268,-30.1365118994154,
-7.48792130212306));
#30843=CARTESIAN_POINT('Ctrl Pts',(-25.442759955772,-31.043317523795,-9.1236083623051));
#30844=CARTESIAN_POINT('Ctrl Pts',(-27.0561790920293,-33.2894343746864,
-11.8774049927261));
#30845=CARTESIAN_POINT('Ctrl Pts',(-28.0356631205829,-34.6044524433959,
-12.9732563608822));
#30846=CARTESIAN_POINT('Ctrl Pts',(-30.2091636816484,-37.5044951004748,
-14.4676858045526));
#30847=CARTESIAN_POINT('Ctrl Pts',(-31.3805975394681,-39.0406651371313,
-14.8501851005579));
#30848=CARTESIAN_POINT('Ctrl Pts',(-32.5588345556906,-40.5934132658116,
-14.8499483202528));
#30849=CARTESIAN_POINT('Ctrl Pts',(-24.8250414362345,-27.7261998529423,
1.62975553161129));
#30850=CARTESIAN_POINT('Ctrl Pts',(-24.7796252351427,-27.7349072261465,
1.18963944139595));
#30851=CARTESIAN_POINT('Ctrl Pts',(-24.7207188400697,-27.7359890779444,
0.664246507200263));
#30852=CARTESIAN_POINT('Ctrl Pts',(-24.5917704575631,-27.8472541630956,
-1.95288623097697));
#30853=CARTESIAN_POINT('Ctrl Pts',(-24.7516062016228,-28.2148983404681,
-3.87317034519611));
#30854=CARTESIAN_POINT('Ctrl Pts',(-25.5363949989286,-29.512282298103,-7.48823335803388));
#30855=CARTESIAN_POINT('Ctrl Pts',(-26.1626472662077,-30.4196491139262,
-9.12349227712643));
#30856=CARTESIAN_POINT('Ctrl Pts',(-27.7758906912596,-32.6655632155557,
-11.8775764776429));
#30857=CARTESIAN_POINT('Ctrl Pts',(-28.7556624629977,-33.9809133009309,
-12.9726927515337));
#30858=CARTESIAN_POINT('Ctrl Pts',(-30.9288420053122,-36.8805855630443,
-14.4683433355025));
#30859=CARTESIAN_POINT('Ctrl Pts',(-32.1004855202296,-38.4170078110375,
-14.8498038985243));
#30860=CARTESIAN_POINT('Ctrl Pts',(-33.2786637049092,-39.9696777567513,
-14.8500516281495));
#30861=CARTESIAN_POINT('Ctrl Pts',(-25.7769069069791,-27.7340963985796,
1.59674386441336));
#30862=CARTESIAN_POINT('Ctrl Pts',(-25.7311178357117,-27.7428752599244,
1.15301439044302));
#30863=CARTESIAN_POINT('Ctrl Pts',(-25.6731513926139,-27.7444892330898,
0.635579209500005));
#30864=CARTESIAN_POINT('Ctrl Pts',(-25.5442092163241,-27.8550468610477,
-1.86860431101006));
#30865=CARTESIAN_POINT('Ctrl Pts',(-25.693699759515,-28.2118877583881,-3.70979114470276));
#30866=CARTESIAN_POINT('Ctrl Pts',(-26.4365494265749,-29.4595339978089,
-7.17014261469294));
#30867=CARTESIAN_POINT('Ctrl Pts',(-27.0327076275534,-30.3330499725233,
-8.73670574474391));
#30868=CARTESIAN_POINT('Ctrl Pts',(-28.56903517708,-32.4898047695082,-11.3734544105212));
#30869=CARTESIAN_POINT('Ctrl Pts',(-29.5038118397362,-33.7541073172778,
-12.4221714958516));
#30870=CARTESIAN_POINT('Ctrl Pts',(-31.5758452047796,-36.5357132426467,
-13.8545909095341));
#30871=CARTESIAN_POINT('Ctrl Pts',(-32.695161691107,-38.0128405673125,-14.2195188099342));
#30872=CARTESIAN_POINT('Ctrl Pts',(-33.818591278132,-39.5018360737644,-14.2201291128083));
#30873=CARTESIAN_POINT('Ctrl Pts',(-23.84085208622,-29.3318883095341,0.));
#30874=CARTESIAN_POINT('Ctrl Pts',(-23.7455006526456,-29.4153831213402,
-1.86858636180619));
#30875=CARTESIAN_POINT('Ctrl Pts',(-23.8932152178166,-29.7701745937408,
-3.71029995872415));
#30876=CARTESIAN_POINT('Ctrl Pts',(-24.6380470280763,-31.0201080010757,
-7.16936247491107));
#30877=CARTESIAN_POINT('Ctrl Pts',(-25.2329893514618,-31.8922209971881,
-8.7369959576894));
#30878=CARTESIAN_POINT('Ctrl Pts',(-26.079536443074,-33.0805753785961,-10.1890856763512));
#30879=CARTESIAN_POINT('Ctrl Pts',(-26.1594145048188,-33.1922116559192,
-10.3203928635188));
#30880=CARTESIAN_POINT('Ctrl Pts',(-26.2409403042445,-33.3057006128373,
-10.4488603766022));
#30881=CARTESIAN_POINT('Ctrl Pts',(-25.6404249706859,-27.7725495286737,
1.99840144432528E-15));
#30882=CARTESIAN_POINT('Ctrl Pts',(-25.5442092163241,-27.8550468610477,
-1.86860431101006));
#30883=CARTESIAN_POINT('Ctrl Pts',(-25.693699759515,-28.2118877583881,-3.70979114470276));
#30884=CARTESIAN_POINT('Ctrl Pts',(-26.4365494265749,-29.4595339978089,
-7.17014261469294));
#30885=CARTESIAN_POINT('Ctrl Pts',(-27.0327076275534,-30.3330499725233,
-8.73670574474391));
#30886=CARTESIAN_POINT('Ctrl Pts',(-27.8833324977841,-31.5271893797546,
-10.1966053555717));
#30887=CARTESIAN_POINT('Ctrl Pts',(-27.9677135840461,-31.6450939272826,
-10.3350231942274));
#30888=CARTESIAN_POINT('Ctrl Pts',(-28.0539337918609,-31.7650675024727,
-10.4702558450997));
#30889=CARTESIAN_POINT('Ctrl Pts',(-26.6166303184857,-35.7920133394054,
1.24689105568337));
#30890=CARTESIAN_POINT('Ctrl Pts',(-26.5668264024408,-35.8015619426292,
0.764254809540774));
#30891=CARTESIAN_POINT('Ctrl Pts',(-26.5193322761002,-35.8093225655935,
0.332948724830941));
#30892=CARTESIAN_POINT('Ctrl Pts',(-26.396380965813,-35.9192508155956,-0.978870002770901));
#30893=CARTESIAN_POINT('Ctrl Pts',(-26.4275870967871,-36.1515731946737,
-1.98783577092234));
#30894=CARTESIAN_POINT('Ctrl Pts',(-26.7378856585374,-36.8859102633355,
-3.80852727280253));
#30895=CARTESIAN_POINT('Ctrl Pts',(-27.0101644118782,-37.3949348243987,
-4.6554436072131));
#30896=CARTESIAN_POINT('Ctrl Pts',(-27.73684930433,-38.6131565530251,-6.0499728334401));
#30897=CARTESIAN_POINT('Ctrl Pts',(-28.1929976957773,-39.3343778781062,
-6.61832169896238));
#30898=CARTESIAN_POINT('Ctrl Pts',(-29.2014824203258,-40.8744649436983,
-7.36768403085421));
#30899=CARTESIAN_POINT('Ctrl Pts',(-29.7658228849728,-41.7224214992554,
-7.57138648700874));
#30900=CARTESIAN_POINT('Ctrl Pts',(-30.3120568904485,-42.5403522177284,
-7.56962581969447));
#30901=CARTESIAN_POINT('Ctrl Pts',(-26.1708926054254,-33.4652890233054,
1.35489343606335));
#30902=CARTESIAN_POINT('Ctrl Pts',(-26.1223268292952,-33.4746002454545,
0.884255668130519));
#30903=CARTESIAN_POINT('Ctrl Pts',(-26.0716101167996,-33.4804735791548,
0.4263970177884));
#30904=CARTESIAN_POINT('Ctrl Pts',(-25.94692887169,-33.5907346359716,-1.25360819506359));
#30905=CARTESIAN_POINT('Ctrl Pts',(-26.014475956126,-33.8612946673281,-2.51960912782488));
#30906=CARTESIAN_POINT('Ctrl Pts',(-26.4585467959957,-34.7543728004604,
-4.84647586779589));
#30907=CARTESIAN_POINT('Ctrl Pts',(-26.8307099768485,-35.3758029321247,
-5.91572199045934));
#30908=CARTESIAN_POINT('Ctrl Pts',(-27.8074490109262,-36.8838857283296,
-7.69376028692768));
#30909=CARTESIAN_POINT('Ctrl Pts',(-28.4113179739206,-37.7727185143413,
-8.41063186552333));
#30910=CARTESIAN_POINT('Ctrl Pts',(-29.7482978092831,-39.6962686996464,
-9.37059840624287));
#30911=CARTESIAN_POINT('Ctrl Pts',(-30.4839404690738,-40.7384561125312,
-9.62435378637076));
#30912=CARTESIAN_POINT('Ctrl Pts',(-31.2084352127804,-41.7636091770246,
-9.62320046360554));
#30913=CARTESIAN_POINT('Ctrl Pts',(-25.2795805846978,-31.2708363785845,
1.47293214974073));
#30914=CARTESIAN_POINT('Ctrl Pts',(-25.232365242191,-31.2798886902734,1.01538106786938));
#30915=CARTESIAN_POINT('Ctrl Pts',(-25.1781488031009,-31.2837215247365,
0.528580803103268));
#30916=CARTESIAN_POINT('Ctrl Pts',(-25.0518358019867,-31.394646464622,-1.554028754611));
#30917=CARTESIAN_POINT('Ctrl Pts',(-25.1587229846876,-31.7065592632734,
-3.10121432126163));
#30918=CARTESIAN_POINT('Ctrl Pts',(-25.7495178005009,-32.7737330382101,
-5.98129145448249));
#30919=CARTESIAN_POINT('Ctrl Pts',(-26.2306311757314,-33.5177631757313,
-7.29389406574815));
#30920=CARTESIAN_POINT('Ctrl Pts',(-27.4809015052032,-35.3429210732409,
-9.49113593805845));
#30921=CARTESIAN_POINT('Ctrl Pts',(-28.2461406191133,-36.4148497431898,
-10.3708286016981));
#30922=CARTESIAN_POINT('Ctrl Pts',(-29.9425080008753,-38.7579223666493,
-11.560404556144));
#30923=CARTESIAN_POINT('Ctrl Pts',(-30.8653690604188,-40.0123393656214,
-11.8694761542094));
#30924=CARTESIAN_POINT('Ctrl Pts',(-31.784805792174,-41.2641519184871,-11.8687142284813));
#30925=CARTESIAN_POINT('Ctrl Pts',(-23.9769478445537,-29.2929893708798,
1.59647090706393));
#30926=CARTESIAN_POINT('Ctrl Pts',(-23.9311433315013,-29.3017711927832,
1.15259179089975));
#30927=CARTESIAN_POINT('Ctrl Pts',(-23.8732845217115,-29.3034887354924,
0.635573104333306));
#30928=CARTESIAN_POINT('Ctrl Pts',(-23.7455006526456,-29.4153831213402,
-1.86858636180619));
#30929=CARTESIAN_POINT('Ctrl Pts',(-23.8932152178166,-29.7701745937408,
-3.71029995872415));
#30930=CARTESIAN_POINT('Ctrl Pts',(-24.6380470280763,-31.0201080010757,
-7.16936247491107));
#30931=CARTESIAN_POINT('Ctrl Pts',(-25.2329893514618,-31.8922209971881,
-8.7369959576894));
#30932=CARTESIAN_POINT('Ctrl Pts',(-26.7697561790066,-34.049482667342,-11.3730256982303));
#30933=CARTESIAN_POINT('Ctrl Pts',(-27.7038134837062,-35.3129551734307,
-12.423580519218));
#30934=CARTESIAN_POINT('Ctrl Pts',(-29.7766493956127,-38.0954870862325,
-13.8529470821643));
#30935=CARTESIAN_POINT('Ctrl Pts',(-30.8954422365098,-39.5719833475698,
-14.2204718557357));
#30936=CARTESIAN_POINT('Ctrl Pts',(-32.0190184050856,-41.0611748464153,
-14.2198708430667));
#30937=CARTESIAN_POINT('Ctrl Pts',(-25.7769069069791,-27.7340963985796,
1.59674386441336));
#30938=CARTESIAN_POINT('Ctrl Pts',(-25.7311178357117,-27.7428752599244,
1.15301439044302));
#30939=CARTESIAN_POINT('Ctrl Pts',(-25.6731513926139,-27.7444892330898,
0.635579209500005));
#30940=CARTESIAN_POINT('Ctrl Pts',(-25.5442092163241,-27.8550468610477,
-1.86860431101006));
#30941=CARTESIAN_POINT('Ctrl Pts',(-25.693699759515,-28.2118877583881,-3.70979114470396));
#30942=CARTESIAN_POINT('Ctrl Pts',(-26.4365494265749,-29.4595339978089,
-7.17014261469174));
#30943=CARTESIAN_POINT('Ctrl Pts',(-27.0327076275534,-30.3330499725233,
-8.73670574474391));
#30944=CARTESIAN_POINT('Ctrl Pts',(-28.56903517708,-32.4898047695081,-11.3734544105212));
#30945=CARTESIAN_POINT('Ctrl Pts',(-29.5038118397362,-33.7541073172778,
-12.4221714958564));
#30946=CARTESIAN_POINT('Ctrl Pts',(-31.5758452047796,-36.5357132426467,
-13.8545909095293));
#30947=CARTESIAN_POINT('Ctrl Pts',(-32.6951616911162,-38.0128405673056,
-14.2195188099294));
#30948=CARTESIAN_POINT('Ctrl Pts',(-33.818591278132,-39.5018360737644,-14.2201291128083));
#30949=CARTESIAN_POINT('Ctrl Pts',(-27.54848130917,-29.3058064687039,1.47327622041477));
#30950=CARTESIAN_POINT('Ctrl Pts',(-27.5012854314845,-29.3148550485271,
1.01591376687878));
#30951=CARTESIAN_POINT('Ctrl Pts',(-27.4469333174786,-29.3185573305633,
0.528588498843375));
#30952=CARTESIAN_POINT('Ctrl Pts',(-27.3191602364347,-29.4277972482744,
-1.55405138010428));
#30953=CARTESIAN_POINT('Ctrl Pts',(-27.428286091058,-29.7422934066342,-3.10057294639553));
#30954=CARTESIAN_POINT('Ctrl Pts',(-28.0165823577485,-30.8065841399291,
-5.98227484335734));
#30955=CARTESIAN_POINT('Ctrl Pts',(-28.4992283820293,-31.5523827727592,
-7.29352824389559));
#30956=CARTESIAN_POINT('Ctrl Pts',(-29.7489449887903,-33.3769017419095,
-9.49167634236217));
#30957=CARTESIAN_POINT('Ctrl Pts',(-30.5150908743223,-34.449876703528,-10.3690524867828));
#30958=CARTESIAN_POINT('Ctrl Pts',(-32.2104466224207,-36.7917820929022,
-11.5624766483316));
#30959=CARTESIAN_POINT('Ctrl Pts',(-33.1339647666498,-38.0469976785157,
-11.8682745705117));
#30960=CARTESIAN_POINT('Ctrl Pts',(-34.0532197137071,-39.2985600643047,
-11.8690397849987));
#30961=CARTESIAN_POINT('Ctrl Pts',(-29.5931790826754,-30.5013447592651,
1.35541241355862));
#30962=CARTESIAN_POINT('Ctrl Pts',(-29.5446426662248,-30.5106503524655,
0.885059162349651));
#30963=CARTESIAN_POINT('Ctrl Pts',(-29.4937213090619,-30.5163267679905,
0.426408625624299));
#30964=CARTESIAN_POINT('Ctrl Pts',(-29.3668377587822,-30.6240462289814,
-1.25364232212737));
#30965=CARTESIAN_POINT('Ctrl Pts',(-29.4377615342147,-30.8985028596602,
-2.5186417128575));
#30966=CARTESIAN_POINT('Ctrl Pts',(-29.8780636984474,-31.7872323695308,
-4.84795915809644));
#30967=CARTESIAN_POINT('Ctrl Pts',(-30.2525386437904,-32.4113300033621,
-5.91517020466357));
#30968=CARTESIAN_POINT('Ctrl Pts',(-31.2284424726378,-33.918449074776,-7.69457540339954));
#30969=CARTESIAN_POINT('Ctrl Pts',(-31.8336791606395,-34.8088600302412,
-8.40795287037808));
#30970=CARTESIAN_POINT('Ctrl Pts',(-33.1691331027958,-36.7306496231332,
-9.3737238374113));
#30971=CARTESIAN_POINT('Ctrl Pts',(-33.9057602738009,-37.7740480458484,
-9.6225408599538));
#30972=CARTESIAN_POINT('Ctrl Pts',(-34.6299874229479,-38.7988173067562,
-9.62369151535372));
#30973=CARTESIAN_POINT('Ctrl Pts',(-31.8324214200721,-31.2747661069639,
1.24768201173563));
#30974=CARTESIAN_POINT('Ctrl Pts',(-31.7826622501122,-31.2843061312878,
0.765479387912171));
#30975=CARTESIAN_POINT('Ctrl Pts',(-31.7348562317659,-31.2917666379301,
0.33296641594115));
#30976=CARTESIAN_POINT('Ctrl Pts',(-31.6085484626271,-31.3978213276697,
-0.978922014674862));
#30977=CARTESIAN_POINT('Ctrl Pts',(-31.6449008941757,-31.6360823820121,
-1.98636136648275));
#30978=CARTESIAN_POINT('Ctrl Pts',(-31.9494557448252,-32.3637918610199,
-3.81078790539403));
#30979=CARTESIAN_POINT('Ctrl Pts',(-32.2252577802593,-32.8768818719414,
-4.65460264913821));
#30980=CARTESIAN_POINT('Ctrl Pts',(-32.9506697646498,-34.0936348201774,
-6.05121512489441));
#30981=CARTESIAN_POINT('Ctrl Pts',(-33.4089026595357,-34.8172613799685,
-6.61423873304044));
#30982=CARTESIAN_POINT('Ctrl Pts',(-34.4150618218505,-36.3546651862003,
-7.37244739482366));
#30983=CARTESIAN_POINT('Ctrl Pts',(-34.9808875865548,-37.2044809779807,
-7.56862230162397));
#30984=CARTESIAN_POINT('Ctrl Pts',(-35.5267289204024,-38.021813177295,-7.57037421505986));
#30985=CARTESIAN_POINT('Ctrl Pts',(-27.9017241322579,-25.5825535213024,
1.59647090706389));
#30986=CARTESIAN_POINT('Ctrl Pts',(-27.8576356266559,-25.5977646187898,
1.15259179090242));
#30987=CARTESIAN_POINT('Ctrl Pts',(-27.8006101679571,-25.6076988465251,
0.635573104329219));
#30988=CARTESIAN_POINT('Ctrl Pts',(-27.6900511858225,-25.7366398496109,
-1.86858636179435));
#30989=CARTESIAN_POINT('Ctrl Pts',(-27.8867543207323,-26.0667980818921,
-3.71029995871567));
#30990=CARTESIAN_POINT('Ctrl Pts',(-28.8018888878676,-27.1980083507359,
-7.1693624749194));
#30991=CARTESIAN_POINT('Ctrl Pts',(-29.5148901762754,-27.9765753734451,
-8.73699595772763));
#30992=CARTESIAN_POINT('Ctrl Pts',(-31.3430252789425,-29.89317450793,-11.373025698192));
#30993=CARTESIAN_POINT('Ctrl Pts',(-32.4473861124854,-31.0108564714034,
-12.4235805192132));
#30994=CARTESIAN_POINT('Ctrl Pts',(-34.8951191227831,-33.4700709137458,
-13.852947082169));
#30995=CARTESIAN_POINT('Ctrl Pts',(-36.2126515924275,-34.7723177498595,
-14.2204718557594));
#30996=CARTESIAN_POINT('Ctrl Pts',(-37.5367254229125,-36.0864498658149,
-14.2198708430666));
#30997=CARTESIAN_POINT('Ctrl Pts',(-27.8942941678685,-24.6306899881721,
1.62964634867148));
#30998=CARTESIAN_POINT('Ctrl Pts',(-27.8505734813071,-24.6457741833911,
1.18947040157796));
#30999=CARTESIAN_POINT('Ctrl Pts',(-27.7924691428838,-24.655263156583,0.664244065133));
#31000=CARTESIAN_POINT('Ctrl Pts',(-27.6812026446472,-24.7842103148066,
-1.95287905129388));
#31001=CARTESIAN_POINT('Ctrl Pts',(-27.8909128870847,-25.1246550797521,
-3.87337387080265));
#31002=CARTESIAN_POINT('Ctrl Pts',(-28.8532656404615,-26.2979391683561,
-7.48792130212299));
#31003=CARTESIAN_POINT('Ctrl Pts',(-29.6017140577926,-27.1064590437618,
-9.12360836233377));
#31004=CARTESIAN_POINT('Ctrl Pts',(-31.518366669829,-29.1001001804546,-11.8774049926974));
#31005=CARTESIAN_POINT('Ctrl Pts',(-32.6750275470923,-30.2623381501783,
-12.9732563608822));
#31006=CARTESIAN_POINT('Ctrl Pts',(-35.23912410816,-32.8235411735974,-14.4676858045526));
#31007=CARTESIAN_POINT('Ctrl Pts',(-36.6172542487524,-34.1773627942107,
-14.8501851005579));
#31008=CARTESIAN_POINT('Ctrl Pts',(-38.0044776097608,-35.5466255754746,
-14.8499483202528));
#31009=CARTESIAN_POINT('Ctrl Pts',(-28.5182079571718,-23.9110153591929,
1.62975553161125));
#31010=CARTESIAN_POINT('Ctrl Pts',(-28.4744932159222,-23.9260975032042,
1.18963944139177));
#31011=CARTESIAN_POINT('Ctrl Pts',(-28.4163403666074,-23.9355515973836,
0.664246507203993));
#31012=CARTESIAN_POINT('Ctrl Pts',(-28.3045391652295,-24.0640354326691,
-1.95288623098812));
#31013=CARTESIAN_POINT('Ctrl Pts',(-28.5150692335544,-24.4051905243133,
-3.87317034520081));
#31014=CARTESIAN_POINT('Ctrl Pts',(-29.4765070006364,-25.577681893135,-7.48823335802902));
#31015=CARTESIAN_POINT('Ctrl Pts',(-30.225516684522,-26.3866880329016,-9.12349227713835));
#31016=CARTESIAN_POINT('Ctrl Pts',(-32.1419665195937,-28.3801534903166,
-11.877576477631));
#31017=CARTESIAN_POINT('Ctrl Pts',(-33.2989594621267,-29.5426791471387,
-12.9726927515433));
#31018=CARTESIAN_POINT('Ctrl Pts',(-35.8626855592739,-32.1035612314167,
-14.4683433354929));
#31019=CARTESIAN_POINT('Ctrl Pts',(-37.2410591163492,-33.4576026589017,
-14.849803898491));
#31020=CARTESIAN_POINT('Ctrl Pts',(-38.628213118051,-34.8267964255887,-14.8500516281495));
#31021=CARTESIAN_POINT('Ctrl Pts',(-29.4615086055162,-23.7833669488545,
1.5967438644133));
#31022=CARTESIAN_POINT('Ctrl Pts',(-29.4174349631938,-23.7985729183137,
1.15301439043676));
#31023=CARTESIAN_POINT('Ctrl Pts',(-29.3602882272664,-23.8084199485298,
0.635579209506715));
#31024=CARTESIAN_POINT('Ctrl Pts',(-29.248392487277,-23.9362026442577,-1.86860431102996));
#31025=CARTESIAN_POINT('Ctrl Pts',(-29.4471451869125,-24.2681366932806,
-3.70979114471347));
#31026=CARTESIAN_POINT('Ctrl Pts',(-30.3599922882989,-25.3973651626973,
-7.17014261468209));
#31027=CARTESIAN_POINT('Ctrl Pts',(-31.0743967431037,-26.1771478462935,
-8.73670574474148));
#31028=CARTESIAN_POINT('Ctrl Pts',(-32.9020249033495,-28.0933077825863,
-11.3734544105236));
#31029=CARTESIAN_POINT('Ctrl Pts',(-34.0072159000762,-29.2117089638021,
-12.4221714958708));
#31030=CARTESIAN_POINT('Ctrl Pts',(-36.454022750563,-31.6701210582965,-13.854590909515));
#31031=CARTESIAN_POINT('Ctrl Pts',(-37.7721633453332,-32.9729180118679,
-14.2195188098961));
#31032=CARTESIAN_POINT('Ctrl Pts',(-39.096064193638,-34.2868769911002,-14.2201291128084));
#31033=CARTESIAN_POINT('Ctrl Pts',(-27.7725495286738,-25.6404249706858,
0.));
#31034=CARTESIAN_POINT('Ctrl Pts',(-27.6900511858225,-25.7366398496109,
-1.86858636179435));
#31035=CARTESIAN_POINT('Ctrl Pts',(-27.8867543207323,-26.0667980818921,
-3.71029995871567));
#31036=CARTESIAN_POINT('Ctrl Pts',(-28.8018888878676,-27.1980083507359,
-7.1693624749194));
#31037=CARTESIAN_POINT('Ctrl Pts',(-29.5148901762754,-27.9765753734451,
-8.73699595772763));
#31038=CARTESIAN_POINT('Ctrl Pts',(-30.5219411006572,-29.0323578083627,
-10.1890856763484));
#31039=CARTESIAN_POINT('Ctrl Pts',(-30.6168936176569,-29.1314899559173,
-10.3203928635139));
#31040=CARTESIAN_POINT('Ctrl Pts',(-30.7137407645416,-29.2322214279374,
-10.4488603765957));
#31041=CARTESIAN_POINT('Ctrl Pts',(-29.3318883095342,-23.8408520862199,
1.11022302462516E-15));
#31042=CARTESIAN_POINT('Ctrl Pts',(-29.248392487277,-23.9362026442577,-1.86860431102996));
#31043=CARTESIAN_POINT('Ctrl Pts',(-29.4471451869125,-24.2681366932806,
-3.70979114471347));
#31044=CARTESIAN_POINT('Ctrl Pts',(-30.3599922882989,-25.3973651626973,
-7.17014261468209));
#31045=CARTESIAN_POINT('Ctrl Pts',(-31.0743967431037,-26.1771478462935,
-8.73670574474148));
#31046=CARTESIAN_POINT('Ctrl Pts',(-32.0863072351854,-27.2380760953858,
-10.1966053555729));
#31047=CARTESIAN_POINT('Ctrl Pts',(-32.1866090102636,-27.342771863985,-10.3350231942299));
#31048=CARTESIAN_POINT('Ctrl Pts',(-32.2890256406274,-27.4492538662409,
-10.4702558451036));
#31049=CARTESIAN_POINT('Ctrl Pts',(-31.4394459897279,-31.6397608122767,
1.24689105568322));
#31050=CARTESIAN_POINT('Ctrl Pts',(-31.3915079136553,-31.656300060737,0.764254809555862));
#31051=CARTESIAN_POINT('Ctrl Pts',(-31.3456016608202,-31.6707408106673,
0.332948724813886));
#31052=CARTESIAN_POINT('Ctrl Pts',(-31.2395462388184,-31.7970479454233,
-0.978870002720858));
#31053=CARTESIAN_POINT('Ctrl Pts',(-31.3034976581266,-32.0225645221647,
-1.9878357708888));
#31054=CARTESIAN_POINT('Ctrl Pts',(-31.7151448890446,-32.7052670087001,
-3.80852727283614));
#31055=CARTESIAN_POINT('Ctrl Pts',(-32.0570939852818,-33.1703611269164,
-4.65544360725139));
#31056=CARTESIAN_POINT('Ctrl Pts',(-32.9497533018099,-34.2727650719354,
-6.04997283340185));
#31057=CARTESIAN_POINT('Ctrl Pts',(-33.5038992565468,-34.9217287192801,
-6.61832169894314));
#31058=CARTESIAN_POINT('Ctrl Pts',(-34.7212963022536,-36.302617578697,-7.36768403087334));
#31059=CARTESIAN_POINT('Ctrl Pts',(-35.4005693948026,-37.0616291372609,
-7.57138648705137));
#31060=CARTESIAN_POINT('Ctrl Pts',(-36.0576472036355,-37.7934972961798,
-7.56962581969424));
#31061=CARTESIAN_POINT('Ctrl Pts',(-30.6671178491336,-29.4001542854017,
1.35489343606322));
#31062=CARTESIAN_POINT('Ctrl Pts',(-30.6203715276488,-29.4162823633143,
0.884255668139903));
#31063=CARTESIAN_POINT('Ctrl Pts',(-30.5710069006851,-29.4293136556735,
0.426397017777568));
#31064=CARTESIAN_POINT('Ctrl Pts',(-30.4632865153969,-29.5561964051703,
-1.25360819503185));
#31065=CARTESIAN_POINT('Ctrl Pts',(-30.5686507749895,-29.8143895731036,
-2.51960912780089));
#31066=CARTESIAN_POINT('Ctrl Pts',(-31.1352998840585,-30.6351795888068,
-4.84647586781987));
#31067=CARTESIAN_POINT('Ctrl Pts',(-31.5921137090052,-31.1973201148342,
-5.91572199048803));
#31068=CARTESIAN_POINT('Ctrl Pts',(-32.7735335073842,-32.5510483450287,
-7.69376028689897));
#31069=CARTESIAN_POINT('Ctrl Pts',(-33.4977500492304,-33.344894581048,-8.41063186551369));
#31070=CARTESIAN_POINT('Ctrl Pts',(-35.0948710910953,-35.0585937299339,
-9.37059840625243));
#31071=CARTESIAN_POINT('Ctrl Pts',(-35.9713447024848,-35.9854803115381,
-9.62435378641347));
#31072=CARTESIAN_POINT('Ctrl Pts',(-36.834359626899,-36.8970924436851,-9.62320046360538));
#31073=CARTESIAN_POINT('Ctrl Pts',(-29.4725749263794,-27.3548849305455,
1.47293214974064));
#31074=CARTESIAN_POINT('Ctrl Pts',(-29.4271284462447,-27.3705645465865,
1.01538106787477));
#31075=CARTESIAN_POINT('Ctrl Pts',(-29.3740093215551,-27.3820741720689,
0.528580803096812));
#31076=CARTESIAN_POINT('Ctrl Pts',(-29.2647682695533,-27.5098462703849,
-1.55402875459216));
#31077=CARTESIAN_POINT('Ctrl Pts',(-29.4149573143427,-27.8033726143276,
-3.101214321246));
#31078=CARTESIAN_POINT('Ctrl Pts',(-30.151613353974,-28.7756052303093,-5.98129145449804));
#31079=CARTESIAN_POINT('Ctrl Pts',(-30.7337162174556,-29.4435926415972,
-7.29389406578162));
#31080=CARTESIAN_POINT('Ctrl Pts',(-32.2310076487022,-31.0722410437307,
-9.49113593802495));
#31081=CARTESIAN_POINT('Ctrl Pts',(-33.1410090871408,-32.024354144657,-10.3708286016932));
#31082=CARTESIAN_POINT('Ctrl Pts',(-35.1535638963654,-34.102159417596,-11.5604045561488));
#31083=CARTESIAN_POINT('Ctrl Pts',(-36.2455537133794,-35.2124714378061,
-11.8694761542426));
#31084=CARTESIAN_POINT('Ctrl Pts',(-37.3337834058788,-36.3206928540898,
-11.8687142284811));
#31085=CARTESIAN_POINT('Ctrl Pts',(-27.9017241322579,-25.5825535213024,
1.59647090706389));
#31086=CARTESIAN_POINT('Ctrl Pts',(-27.8576356266559,-25.5977646187898,
1.15259179090242));
#31087=CARTESIAN_POINT('Ctrl Pts',(-27.8006101679571,-25.6076988465251,
0.635573104329223));
#31088=CARTESIAN_POINT('Ctrl Pts',(-27.6900511858225,-25.7366398496109,
-1.86858636179435));
#31089=CARTESIAN_POINT('Ctrl Pts',(-27.8867543207323,-26.0667980818921,
-3.71029995871567));
#31090=CARTESIAN_POINT('Ctrl Pts',(-28.8018888878676,-27.1980083507359,
-7.1693624749194));
#31091=CARTESIAN_POINT('Ctrl Pts',(-29.5148901762754,-27.9765753734451,
-8.73699595772763));
#31092=CARTESIAN_POINT('Ctrl Pts',(-31.3430252789425,-29.89317450793,-11.373025698192));
#31093=CARTESIAN_POINT('Ctrl Pts',(-32.4473861124854,-31.0108564714034,
-12.4235805192132));
#31094=CARTESIAN_POINT('Ctrl Pts',(-34.8951191227831,-33.4700709137458,
-13.852947082169));
#31095=CARTESIAN_POINT('Ctrl Pts',(-36.2126515924275,-34.7723177498594,
-14.2204718557404));
#31096=CARTESIAN_POINT('Ctrl Pts',(-37.5367254229125,-36.0864498658149,
-14.2198708430666));
#31097=CARTESIAN_POINT('Ctrl Pts',(-29.4615086055162,-23.7833669488545,
1.5967438644133));
#31098=CARTESIAN_POINT('Ctrl Pts',(-29.4174349631938,-23.7985729183137,
1.15301439043676));
#31099=CARTESIAN_POINT('Ctrl Pts',(-29.3602882272664,-23.8084199485298,
0.635579209506715));
#31100=CARTESIAN_POINT('Ctrl Pts',(-29.248392487277,-23.9362026442577,-1.86860431102996));
#31101=CARTESIAN_POINT('Ctrl Pts',(-29.4471451869125,-24.268136693283,-3.70979114471227));
#31102=CARTESIAN_POINT('Ctrl Pts',(-30.3599922882989,-25.3973651626949,
-7.17014261468329));
#31103=CARTESIAN_POINT('Ctrl Pts',(-31.0743967431037,-26.1771478462935,
-8.73670574474149));
#31104=CARTESIAN_POINT('Ctrl Pts',(-32.9020249033495,-28.0933077825863,
-11.3734544105236));
#31105=CARTESIAN_POINT('Ctrl Pts',(-34.0072159000762,-29.2117089638045,
-12.4221714958708));
#31106=CARTESIAN_POINT('Ctrl Pts',(-36.454022750563,-31.6701210582941,-13.854590909515));
#31107=CARTESIAN_POINT('Ctrl Pts',(-37.7721633453175,-32.9729180118855,
-14.2195188099009));
#31108=CARTESIAN_POINT('Ctrl Pts',(-39.096064193638,-34.2868769911001,-14.2201291128084));
#31109=CARTESIAN_POINT('Ctrl Pts',(-31.4387285991344,-25.0869579521469,
1.47327622041467));
#31110=CARTESIAN_POINT('Ctrl Pts',(-31.3933008545932,-25.1026311041689,
1.01591376687352));
#31111=CARTESIAN_POINT('Ctrl Pts',(-31.3400288564346,-25.1140308146317,
0.528588498850527));
#31112=CARTESIAN_POINT('Ctrl Pts',(-31.2291027822934,-25.2403428328586,
-1.55405138012545));
#31113=CARTESIAN_POINT('Ctrl Pts',(-31.3818753630052,-25.5361076454293,
-3.10057294640389));
#31114=CARTESIAN_POINT('Ctrl Pts',(-32.1156479855591,-26.5058421456065,
-5.98227484334892));
#31115=CARTESIAN_POINT('Ctrl Pts',(-32.6995195810811,-27.1753619327956,
-7.29352824387644));
#31116=CARTESIAN_POINT('Ctrl Pts',(-34.1961719966593,-28.8034567128286,
-9.49167634238131));
#31117=CARTESIAN_POINT('Ctrl Pts',(-35.1072198799242,-29.7564764086336,
-10.3690524868068));
#31118=CARTESIAN_POINT('Ctrl Pts',(-37.1186072377929,-31.8332702987844,
-11.5624766483077));
#31119=CARTESIAN_POINT('Ctrl Pts',(-38.2113611019678,-32.9442792642464,
-11.8682745704737));
#31120=CARTESIAN_POINT('Ctrl Pts',(-39.2993752576342,-34.0522789304537,
-11.8690397849988));
#31121=CARTESIAN_POINT('Ctrl Pts',(-33.632757135987,-25.9793365537799,1.35541241355846));
#31122=CARTESIAN_POINT('Ctrl Pts',(-33.5860390742569,-25.9954548817124,
0.885059162342653));
#31123=CARTESIAN_POINT('Ctrl Pts',(-33.5364438612593,-26.0083203842374,
0.426408625633996));
#31124=CARTESIAN_POINT('Ctrl Pts',(-33.4261818802089,-26.133000828325,-1.25364232215596));
#31125=CARTESIAN_POINT('Ctrl Pts',(-33.5354430048895,-26.3945703806125,
-2.51864171286469));
#31126=CARTESIAN_POINT('Ctrl Pts',(-34.0977429244459,-27.211592374279,-4.84795915808926));
#31127=CARTESIAN_POINT('Ctrl Pts',(-34.5572246086141,-27.7760442527838,
-5.91517020462051));
#31128=CARTESIAN_POINT('Ctrl Pts',(-35.7376805505111,-29.1289374295152,
-7.69457540344261));
#31129=CARTESIAN_POINT('Ctrl Pts',(-36.463475492835,-29.9241511239475,-8.40795287040691));
#31130=CARTESIAN_POINT('Ctrl Pts',(-38.0588356145443,-31.636324758031,-9.3737238373826));
#31131=CARTESIAN_POINT('Ctrl Pts',(-38.9364560608509,-32.5642699125021,
-9.62254085988727));
#31132=CARTESIAN_POINT('Ctrl Pts',(-39.7991514935067,-33.4755402303455,
-9.62369151535387));
#31133=CARTESIAN_POINT('Ctrl Pts',(-35.9592765491246,-26.4262081762393,
1.24768201173543));
#31134=CARTESIAN_POINT('Ctrl Pts',(-35.9113815427857,-26.4427325650909,
0.765479387902019));
#31135=CARTESIAN_POINT('Ctrl Pts',(-35.8651238615775,-26.4569206403349,
0.332966415955371));
#31136=CARTESIAN_POINT('Ctrl Pts',(-35.7551948794087,-26.5798713158822,
-0.978922014716766));
#31137=CARTESIAN_POINT('Ctrl Pts',(-35.8250853790451,-26.8105337258487,
-1.98636136649238));
#31138=CARTESIAN_POINT('Ctrl Pts',(-36.2301041572687,-27.4874934974146,
-3.81078790538449));
#31139=CARTESIAN_POINT('Ctrl Pts',(-36.5761192475516,-27.9561102697828,
-4.65460264906168));
#31140=CARTESIAN_POINT('Ctrl Pts',(-37.4673095829948,-29.0572415380562,
-6.05121512497099));
#31141=CARTESIAN_POINT('Ctrl Pts',(-38.0238611245252,-29.7082892825274,
-6.61423873306931));
#31142=CARTESIAN_POINT('Ctrl Pts',(-39.2385744113842,-31.08685315642,-7.37244739479499));
#31143=CARTESIAN_POINT('Ctrl Pts',(-39.9195822825557,-31.8474936465318,
-7.56862230155737));
#31144=CARTESIAN_POINT('Ctrl Pts',(-40.5761862384897,-32.5788252613915,
-7.57037421506009));
#31145=CARTESIAN_POINT('Ctrl Pts',(-31.2585017743464,-21.3513306581893,
1.5964708619975));
#31146=CARTESIAN_POINT('Ctrl Pts',(-31.2170267923822,-21.3726613764954,
1.15259176010419));
#31147=CARTESIAN_POINT('Ctrl Pts',(-31.1619955607693,-21.3906100567219,
0.635573083876073));
#31148=CARTESIAN_POINT('Ctrl Pts',(-31.0709121283971,-21.5339728088745,
-1.86858636179032));
#31149=CARTESIAN_POINT('Ctrl Pts',(-31.3125995244277,-21.8327767315655,
-3.71029995869747));
#31150=CARTESIAN_POINT('Ctrl Pts',(-32.3794073476997,-22.8222356829231,
-7.16936247493759));
#31151=CARTESIAN_POINT('Ctrl Pts',(-33.1959529508923,-23.4914073530275,
-8.73699595768452));
#31152=CARTESIAN_POINT('Ctrl Pts',(-35.2782407701427,-25.1283275201853,
-11.3730256982351));
#31153=CARTESIAN_POINT('Ctrl Pts',(-36.5304235306209,-26.0774661593507,
-12.4235805192512));
#31154=CARTESIAN_POINT('Ctrl Pts',(-39.3032248537559,-28.1633006173621,
-13.852947082131));
#31155=CARTESIAN_POINT('Ctrl Pts',(-40.7926757902182,-29.2647880382123,
-14.220471855574));
#31156=CARTESIAN_POINT('Ctrl Pts',(-42.2902929581064,-30.3771088306743,
-14.2198708430667));
#31157=CARTESIAN_POINT('Ctrl Pts',(-31.1156831315056,-20.4102131175329,
1.62964630360509));
#31158=CARTESIAN_POINT('Ctrl Pts',(-31.0745541646235,-20.4313658791528,
1.18947037065693));
#31159=CARTESIAN_POINT('Ctrl Pts',(-31.0183916684119,-20.4490273774703,
0.664244043755391));
#31160=CARTESIAN_POINT('Ctrl Pts',(-30.9266087973868,-20.5924969121563,
-1.95287905128436));
#31161=CARTESIAN_POINT('Ctrl Pts',(-31.1826348335827,-20.8996315610389,
-3.8733738707857));
#31162=CARTESIAN_POINT('Ctrl Pts',(-32.3021679589144,-21.9240162327835,
-7.48792130213993));
#31163=CARTESIAN_POINT('Ctrl Pts',(-33.1580626257291,-22.6177912263194,
-9.12360836230261));
#31164=CARTESIAN_POINT('Ctrl Pts',(-35.3389311938565,-24.3183718641586,
-11.8774049927285));
#31165=CARTESIAN_POINT('Ctrl Pts',(-36.649222639852,-25.3041699213976,-12.9732563608962));
#31166=CARTESIAN_POINT('Ctrl Pts',(-39.5517175889612,-27.4743946039037,
-14.4676858045385));
#31167=CARTESIAN_POINT('Ctrl Pts',(-41.1084892565552,-28.618307904635,-14.8501851004628));
#31168=CARTESIAN_POINT('Ctrl Pts',(-42.6764590955598,-29.776211096424,-14.8499483202528));
#31169=CARTESIAN_POINT('Ctrl Pts',(-31.6308259996107,-19.6090715485704,
1.62975548654487));
#31170=CARTESIAN_POINT('Ctrl Pts',(-31.5897026256008,-19.6302214337556,
1.18963941046845));
#31171=CARTESIAN_POINT('Ctrl Pts',(-31.5334871484746,-19.6478553118982,
0.664246485824284));
#31172=CARTESIAN_POINT('Ctrl Pts',(-31.4411090790738,-19.7909423357851,
-1.95288623097265));
#31173=CARTESIAN_POINT('Ctrl Pts',(-31.6980476865419,-20.0986634078754,
-3.87317034519465));
#31174=CARTESIAN_POINT('Ctrl Pts',(-32.8165623230563,-21.1223936447321,
-7.48823335803519));
#31175=CARTESIAN_POINT('Ctrl Pts',(-33.6730817461571,-21.8165700765847,
-9.12349227712632));
#31176=CARTESIAN_POINT('Ctrl Pts',(-35.8537245995411,-23.5170056814859,
-11.8775764776429));
#31177=CARTESIAN_POINT('Ctrl Pts',(-37.1643856730156,-24.5030412397768,
-12.9726927515238));
#31178=CARTESIAN_POINT('Ctrl Pts',(-40.0664682545546,-26.6730009723283,
-14.4683433355124));
#31179=CARTESIAN_POINT('Ctrl Pts',(-41.6235121428231,-27.8170972008458,
-14.8498038985385));
#31180=CARTESIAN_POINT('Ctrl Pts',(-43.1914035066775,-28.9749419513884,
-14.8500516281495));
#31181=CARTESIAN_POINT('Ctrl Pts',(-32.546358944609,-19.3484767357832,1.59674381934694));
#31182=CARTESIAN_POINT('Ctrl Pts',(-32.5048979448244,-19.3698002629962,
1.15301435963279));
#31183=CARTESIAN_POINT('Ctrl Pts',(-32.4497342609268,-19.3876798927917,
0.635579189048305));
#31184=CARTESIAN_POINT('Ctrl Pts',(-32.3571628326124,-19.5300863679464,
-1.86860431101105));
#31185=CARTESIAN_POINT('Ctrl Pts',(-32.6011316568376,-19.8303563486603,
-3.70979114471446));
#31186=CARTESIAN_POINT('Ctrl Pts',(-33.6653932580424,-20.818179212791,-7.17014261468111));
#31187=CARTESIAN_POINT('Ctrl Pts',(-34.4835007519621,-21.4883544786787,
-8.73670574475098));
#31188=CARTESIAN_POINT('Ctrl Pts',(-36.5652242843543,-23.1249120635156,
-11.373454410514));
#31189=CARTESIAN_POINT('Ctrl Pts',(-37.8183311135274,-24.0746444552904,
-12.4221714958225));
#31190=CARTESIAN_POINT('Ctrl Pts',(-40.5901015177415,-26.1598165384319,
-13.8545909095632));
#31191=CARTESIAN_POINT('Ctrl Pts',(-42.0802326794301,-27.2617619321623,
-14.219518810015));
#31192=CARTESIAN_POINT('Ctrl Pts',(-43.5776539859008,-28.3739359680852,
-14.2201291128084));
#31193=CARTESIAN_POINT('Ctrl Pts',(-31.1388779521429,-21.4269965203141,
0.));
#31194=CARTESIAN_POINT('Ctrl Pts',(-31.0709121283971,-21.5339728088745,
-1.86858636179032));
#31195=CARTESIAN_POINT('Ctrl Pts',(-31.3125995244325,-21.8327767315655,
-3.71029995869628));
#31196=CARTESIAN_POINT('Ctrl Pts',(-32.3794073476949,-22.8222356829231,
-7.1693624749388));
#31197=CARTESIAN_POINT('Ctrl Pts',(-33.1959529508875,-23.4914073530251,
-8.73699595768692));
#31198=CARTESIAN_POINT('Ctrl Pts',(-34.3430070554517,-24.3931251555404,
-10.1890856763507));
#31199=CARTESIAN_POINT('Ctrl Pts',(-34.4511010682896,-24.4777351286599,
-10.3203928635182));
#31200=CARTESIAN_POINT('Ctrl Pts',(-34.561298034014,-24.5636585134826,-10.4488603766016));
#31201=CARTESIAN_POINT('Ctrl Pts',(-32.4262389885813,-19.4238236466308,
5.55111512312578E-17));
#31202=CARTESIAN_POINT('Ctrl Pts',(-32.3571628326124,-19.5300863679464,
-1.86860431101105));
#31203=CARTESIAN_POINT('Ctrl Pts',(-32.6011316568376,-19.8303563486603,
-3.70979114471446));
#31204=CARTESIAN_POINT('Ctrl Pts',(-33.6653932580424,-20.818179212791,-7.17014261468111));
#31205=CARTESIAN_POINT('Ctrl Pts',(-34.4835007519621,-21.4883544786787,
-8.73670574475098));
#31206=CARTESIAN_POINT('Ctrl Pts',(-35.6360972865638,-22.3944741298273,
-10.1966053555709));
#31207=CARTESIAN_POINT('Ctrl Pts',(-35.7502778955778,-22.4838298155547,
-10.3350231942257));
#31208=CARTESIAN_POINT('Ctrl Pts',(-35.8668060412531,-22.5746525783681,
-10.4702558450969));
#31209=CARTESIAN_POINT('Ctrl Pts',(-35.622245200284,-26.8434139987114,1.24689101061694));
#31210=CARTESIAN_POINT('Ctrl Pts',(-35.5771488466483,-26.8666072002778,
0.76425478004101));
#31211=CARTESIAN_POINT('Ctrl Pts',(-35.5337649882637,-26.8874341048637,
0.332948714107228));
#31212=CARTESIAN_POINT('Ctrl Pts',(-35.4467644378207,-27.0275488741708,
-0.978870002741806));
#31213=CARTESIAN_POINT('Ctrl Pts',(-35.5421592790146,-27.2416687814337,
-1.98783577087493));
#31214=CARTESIAN_POINT('Ctrl Pts',(-36.0467752285009,-27.8588388319703,
-3.80852727285));
#31215=CARTESIAN_POINT('Ctrl Pts',(-36.4514335703522,-28.2705345323084,
-4.65544360719879));
#31216=CARTESIAN_POINT('Ctrl Pts',(-37.4918953411247,-29.2346789284782,
-6.04997283345455));
#31217=CARTESIAN_POINT('Ctrl Pts',(-38.1327580455326,-29.7981738697285,
-6.61832169905812));
#31218=CARTESIAN_POINT('Ctrl Pts',(-39.5342847196047,-30.9917536078482,
-7.36768403075847));
#31219=CARTESIAN_POINT('Ctrl Pts',(-40.3146623987948,-31.6463688825735,
-7.57138648661831));
#31220=CARTESIAN_POINT('Ctrl Pts',(-41.069207801424,-32.2772757571273,-7.56962581969434));
#31221=CARTESIAN_POINT('Ctrl Pts',(-34.5390490058877,-24.7365171914566,
1.35489339099692));
#31222=CARTESIAN_POINT('Ctrl Pts',(-34.495073760779,-24.7591338032465,0.884255638227479));
#31223=CARTESIAN_POINT('Ctrl Pts',(-34.4480661428486,-24.7790577744534,
0.426397004060221));
#31224=CARTESIAN_POINT('Ctrl Pts',(-34.3594994945276,-24.9199792485703,
-1.25360819504204));
#31225=CARTESIAN_POINT('Ctrl Pts',(-34.5005360167971,-25.1605494847803,
-2.51960912779196));
#31226=CARTESIAN_POINT('Ctrl Pts',(-35.1782280532587,-25.8923424652779,
-4.8464758678288));
#31227=CARTESIAN_POINT('Ctrl Pts',(-35.7103931102495,-26.383749825687,-5.91572199044976));
#31228=CARTESIAN_POINT('Ctrl Pts',(-37.0724433726275,-27.5555654868557,
-7.6937602869373));
#31229=CARTESIAN_POINT('Ctrl Pts',(-37.9022645329764,-28.2382647528049,
-8.41063186559025));
#31230=CARTESIAN_POINT('Ctrl Pts',(-39.7270140028392,-29.7072268925306,
-9.37059840617594));
#31231=CARTESIAN_POINT('Ctrl Pts',(-40.726476090564,-30.4999439048389,-9.62435378608523));
#31232=CARTESIAN_POINT('Ctrl Pts',(-41.7104427005355,-31.2794573106203,
-9.62320046360545));
#31233=CARTESIAN_POINT('Ctrl Pts',(-33.0655926302367,-22.8820669124603,
1.4729321046743));
#31234=CARTESIAN_POINT('Ctrl Pts',(-33.0228401731413,-22.9040546403855,
1.01538103752956));
#31235=CARTESIAN_POINT('Ctrl Pts',(-32.97189971713,-22.9230067538041,0.528580786088482));
#31236=CARTESIAN_POINT('Ctrl Pts',(-32.8819544477915,-23.0650249379137,
-1.55402875459391));
#31237=CARTESIAN_POINT('Ctrl Pts',(-33.0723879388088,-23.3341894772883,
-3.10121432123244));
#31238=CARTESIAN_POINT('Ctrl Pts',(-33.9399090096342,-24.1916890818838,
-5.98129145451161));
#31239=CARTESIAN_POINT('Ctrl Pts',(-34.6111514256777,-24.770035469683,-7.29389406574571));
#31240=CARTESIAN_POINT('Ctrl Pts',(-36.3249834230578,-26.1690197914205,
-9.49113593806087));
#31241=CARTESIAN_POINT('Ctrl Pts',(-37.3612221809205,-26.98193504625,-10.370828601741));
#31242=CARTESIAN_POINT('Ctrl Pts',(-39.6489946054446,-28.7521748454075,
-11.5604045561011));
#31243=CARTESIAN_POINT('Ctrl Pts',(-40.8878834161069,-29.6957791360099,
-11.8694761540333));
#31244=CARTESIAN_POINT('Ctrl Pts',(-42.1227528511809,-30.6378492234121,
-11.8687142284812));
#31245=CARTESIAN_POINT('Ctrl Pts',(-31.2585017743464,-21.3513306581893,
1.5964708619975));
#31246=CARTESIAN_POINT('Ctrl Pts',(-31.2170267923791,-21.3726613764954,
1.15259176010449));
#31247=CARTESIAN_POINT('Ctrl Pts',(-31.1619955607693,-21.3906100567219,
0.635573083876073));
#31248=CARTESIAN_POINT('Ctrl Pts',(-31.0709121283971,-21.5339728088745,
-1.86858636179032));
#31249=CARTESIAN_POINT('Ctrl Pts',(-31.3125995244325,-21.8327767315655,
-3.71029995869628));
#31250=CARTESIAN_POINT('Ctrl Pts',(-32.3794073476949,-22.8222356829231,
-7.1693624749388));
#31251=CARTESIAN_POINT('Ctrl Pts',(-33.1959529508875,-23.4914073530251,
-8.73699595768692));
#31252=CARTESIAN_POINT('Ctrl Pts',(-35.2782407701475,-25.1283275201876,
-11.3730256982327));
#31253=CARTESIAN_POINT('Ctrl Pts',(-36.5304235306209,-26.0774661593532,
-12.4235805192512));
#31254=CARTESIAN_POINT('Ctrl Pts',(-39.3032248537558,-28.1633006173597,
-13.852947082131));
#31255=CARTESIAN_POINT('Ctrl Pts',(-40.792675790223,-29.2647880382077,-14.220471855574));
#31256=CARTESIAN_POINT('Ctrl Pts',(-42.2902929581064,-30.3771088306743,
-14.2198708430667));
#31257=CARTESIAN_POINT('Ctrl Pts',(-32.546358944609,-19.3484767357832,1.59674381934694));
#31258=CARTESIAN_POINT('Ctrl Pts',(-32.5048979448244,-19.3698002629962,
1.15301435963279));
#31259=CARTESIAN_POINT('Ctrl Pts',(-32.4497342609268,-19.3876798927917,
0.635579189048305));
#31260=CARTESIAN_POINT('Ctrl Pts',(-32.3571628326124,-19.5300863679464,
-1.86860431101105));
#31261=CARTESIAN_POINT('Ctrl Pts',(-32.6011316568376,-19.8303563486603,
-3.70979114471446));
#31262=CARTESIAN_POINT('Ctrl Pts',(-33.6653932580424,-20.818179212791,-7.17014261468111));
#31263=CARTESIAN_POINT('Ctrl Pts',(-34.4835007519573,-21.4883544786811,
-8.73670574474859));
#31264=CARTESIAN_POINT('Ctrl Pts',(-36.5652242843591,-23.1249120635132,
-11.3734544105164));
#31265=CARTESIAN_POINT('Ctrl Pts',(-37.8183311135274,-24.0746444552904,
-12.4221714958225));
#31266=CARTESIAN_POINT('Ctrl Pts',(-40.5901015177415,-26.1598165384319,
-13.8545909095632));
#31267=CARTESIAN_POINT('Ctrl Pts',(-42.0802326794284,-27.2617619321646,
-14.219518810015));
#31268=CARTESIAN_POINT('Ctrl Pts',(-43.5776539859008,-28.3739359680852,
-14.2201291128084));
#31269=CARTESIAN_POINT('Ctrl Pts',(-34.688974032416,-20.3574113186625,1.47327617534836));
#31270=CARTESIAN_POINT('Ctrl Pts',(-34.6462392002796,-20.3793899820083,
1.01591373651933));
#31271=CARTESIAN_POINT('Ctrl Pts',(-34.5951317842973,-20.3982550553481,
0.528588481835565));
#31272=CARTESIAN_POINT('Ctrl Pts',(-34.5033108528189,-20.5390678245049,
-1.55405138010844));
#31273=CARTESIAN_POINT('Ctrl Pts',(-34.6966201503934,-20.8100803726322,
-3.1005729464179));
#31274=CARTESIAN_POINT('Ctrl Pts',(-35.5609316342885,-21.6655176417209,
-5.98227484333492));
#31275=CARTESIAN_POINT('Ctrl Pts',(-36.2341428589936,-22.2451290911801,
-7.29352824390031));
#31276=CARTESIAN_POINT('Ctrl Pts',(-37.9472635563893,-23.6436563673571,
-9.4916763423574));
#31277=CARTESIAN_POINT('Ctrl Pts',(-38.9846671297029,-24.4573200646131,
-10.3690524867489));
#31278=CARTESIAN_POINT('Ctrl Pts',(-41.2711400509577,-26.2267249209926,
-11.5624766483654));
#31279=CARTESIAN_POINT('Ctrl Pts',(-42.5108843176328,-27.1709103277457,
-11.8682745706116));
#31280=CARTESIAN_POINT('Ctrl Pts',(-43.7455088513557,-28.112791596242,-11.8690397849987));
#31281=CARTESIAN_POINT('Ctrl Pts',(-36.9876692386613,-20.9284639764453,
1.35541236849222));
#31282=CARTESIAN_POINT('Ctrl Pts',(-36.9437205780641,-20.9510669157128,
0.885059132418801));
#31283=CARTESIAN_POINT('Ctrl Pts',(-36.8964611268098,-20.9708596004016,
0.42640861190665));
#31284=CARTESIAN_POINT('Ctrl Pts',(-36.8050653317125,-21.1099628921499,
-1.25364232213785));
#31285=CARTESIAN_POINT('Ctrl Pts',(-36.9504395642135,-21.3533205642746,
-2.51864171289894));
#31286=CARTESIAN_POINT('Ctrl Pts',(-37.6232904342764,-22.0820028300357,
-4.84795915805504));
#31287=CARTESIAN_POINT('Ctrl Pts',(-38.1584251351866,-22.5753183406665,
-5.91517020467311));
#31288=CARTESIAN_POINT('Ctrl Pts',(-39.5194025113629,-23.746444619158,-7.69457540339));
#31289=CARTESIAN_POINT('Ctrl Pts',(-40.3509806159836,-24.4302727949682,
-8.40795287031555));
#31290=CARTESIAN_POINT('Ctrl Pts',(-42.1737699857923,-25.89797555241,-9.37372383747387));
#31291=CARTESIAN_POINT('Ctrl Pts',(-43.1745178860502,-26.6915771512951,
-9.62254086014419));
#31292=CARTESIAN_POINT('Ctrl Pts',(-44.158119610933,-27.4707976903314,-9.6236915153538));
#31293=CARTESIAN_POINT('Ctrl Pts',(-39.3541045014164,-21.0396888561034,
1.24768196666925));
#31294=CARTESIAN_POINT('Ctrl Pts',(-39.3090486643439,-21.062861219838,0.765479358368067));
#31295=CARTESIAN_POINT('Ctrl Pts',(-39.2652809953009,-21.0834880350827,
0.332966405233472));
#31296=CARTESIAN_POINT('Ctrl Pts',(-39.1739686379048,-21.2208317741238,
-0.978922014694586));
#31297=CARTESIAN_POINT('Ctrl Pts',(-39.2759744366033,-21.4391999182154,
-1.98636136654806));
#31298=CARTESIAN_POINT('Ctrl Pts',(-39.7732121280719,-22.0516290335938,
-3.81078790532884));
#31299=CARTESIAN_POINT('Ctrl Pts',(-40.1823964038188,-22.4662328811704,
-4.65460264915733));
#31300=CARTESIAN_POINT('Ctrl Pts',(-41.2212230249915,-23.4293266125112,
-6.05121512487531));
#31301=CARTESIAN_POINT('Ctrl Pts',(-41.8647634287622,-23.9945420871117,
-6.6142387329492));
#31302=CARTESIAN_POINT('Ctrl Pts',(-43.2633027806245,-25.1862024432709,
-7.37244739491497));
#31303=CARTESIAN_POINT('Ctrl Pts',(-44.0456294021901,-25.8421831847813,
-7.56862230193347));
#31304=CARTESIAN_POINT('Ctrl Pts',(-44.7996294168197,-26.4726264127402,
-7.57037421505999));
#31305=CARTESIAN_POINT('Ctrl Pts',(-33.9789464595043,-16.6854562787124,
1.5964707761032));
#31306=CARTESIAN_POINT('Ctrl Pts',(-33.9409293131115,-16.712472384756,1.15259170140102));
#31307=CARTESIAN_POINT('Ctrl Pts',(-33.8890125875502,-16.7380701329957,
0.635573044902023));
#31308=CARTESIAN_POINT('Ctrl Pts',(-33.8192589011655,-16.8929361804564,
-1.86858636180863));
#31309=CARTESIAN_POINT('Ctrl Pts',(-34.1010104999369,-17.1543030074678,
-3.71029995871351));
#31310=CARTESIAN_POINT('Ctrl Pts',(-35.2977744483822,-17.9818681105444,
-7.16936247492166));
#31311=CARTESIAN_POINT('Ctrl Pts',(-36.2012418527657,-18.52802202229,-8.73699595772984));
#31312=CARTESIAN_POINT('Ctrl Pts',(-38.4952930131949,-19.8519402484793,
-11.3730256981899));
#31313=CARTESIAN_POINT('Ctrl Pts',(-39.8698068706361,-20.6132138376926,
-12.4235805192373));
#31314=CARTESIAN_POINT('Ctrl Pts',(-42.9112302679262,-22.2832067364649,
-13.852947082145));
#31315=CARTESIAN_POINT('Ctrl Pts',(-44.542278745562,-23.1615116346327,-14.220471855593));
#31316=CARTESIAN_POINT('Ctrl Pts',(-46.1829520838074,-24.0493774600892,
-14.2198708430667));
#31317=CARTESIAN_POINT('Ctrl Pts',(-33.7036465139254,-15.7742431696986,
1.62964621771081));
#31318=CARTESIAN_POINT('Ctrl Pts',(-33.6659465347885,-15.8010338873349,
1.18947031171706));
#31319=CARTESIAN_POINT('Ctrl Pts',(-33.6128691890195,-15.8265083724895,
0.664244003023023));
#31320=CARTESIAN_POINT('Ctrl Pts',(-33.5424383800422,-15.9815796560817,
-1.95287905130295));
#31321=CARTESIAN_POINT('Ctrl Pts',(-33.8395682582167,-16.2491518132483,
-3.8733738708029));
#31322=CARTESIAN_POINT('Ctrl Pts',(-35.0934912894295,-17.1037835504083,
-7.48792130212284));
#31323=CARTESIAN_POINT('Ctrl Pts',(-36.039408658731,-17.6686904035875,-9.12360836232398));
#31324=CARTESIAN_POINT('Ctrl Pts',(-38.4400969876706,-19.0415916253474,
-11.8774049927072));
#31325=CARTESIAN_POINT('Ctrl Pts',(-39.8773452471794,-19.8308817644304,
-12.9732563608919));
#31326=CARTESIAN_POINT('Ctrl Pts',(-43.0591521575018,-21.5659485894734,
-14.4676858045429));
#31327=CARTESIAN_POINT('Ctrl Pts',(-44.7628739705109,-22.4766667942929,
-14.8501851005009));
#31328=CARTESIAN_POINT('Ctrl Pts',(-46.4796709429185,-23.3996388269523,
-14.8499483202528));
#31329=CARTESIAN_POINT('Ctrl Pts',(-34.0995316375869,-14.9079435927954,
1.62975540065056));
#31330=CARTESIAN_POINT('Ctrl Pts',(-34.0618367850434,-14.9347306673279,
1.18963935152099));
#31331=CARTESIAN_POINT('Ctrl Pts',(-34.0087030668448,-14.9601853534011,
0.664246445090203));
#31332=CARTESIAN_POINT('Ctrl Pts',(-33.9376286808235,-15.1149627251836,
-1.95288623098664));
#31333=CARTESIAN_POINT('Ctrl Pts',(-34.2357452983146,-15.3829854641729,
-3.87317034520824));
#31334=CARTESIAN_POINT('Ctrl Pts',(-35.4885670716678,-16.237114373715,-7.48823335802167));
#31335=CARTESIAN_POINT('Ctrl Pts',(-36.4351599687878,-16.8023296670664,
-9.12349227711899));
#31336=CARTESIAN_POINT('Ctrl Pts',(-38.8356042400472,-18.1751194546594,
-11.8775764776503));
#31337=CARTESIAN_POINT('Ctrl Pts',(-40.273252164705,-18.9645920738991,-12.9726927515338));
#31338=CARTESIAN_POINT('Ctrl Pts',(-43.4546131984608,-20.6994553318364,
-14.4683433355024));
#31339=CARTESIAN_POINT('Ctrl Pts',(-45.1586304946511,-21.610315861468,-14.8498038985814));
#31340=CARTESIAN_POINT('Ctrl Pts',(-46.8753414736305,-22.5332412158905,
-14.8500516281495));
#31341=CARTESIAN_POINT('Ctrl Pts',(-34.9686592686579,-14.5197073364544,
1.59674373345257));
#31342=CARTESIAN_POINT('Ctrl Pts',(-34.9306549387506,-14.5467143347365,
1.15301430091077));
#31343=CARTESIAN_POINT('Ctrl Pts',(-34.8785972821108,-14.5722625852753,
0.635579150069985));
#31344=CARTESIAN_POINT('Ctrl Pts',(-34.8072346531258,-14.7263938532101,
-1.86860431101787));
#31345=CARTESIAN_POINT('Ctrl Pts',(-35.0914531001935,-14.9888871347756,
-3.70979114472567));
#31346=CARTESIAN_POINT('Ctrl Pts',(-36.2854639039658,-15.8151951688146,
-7.17014261466994));
#31347=CARTESIAN_POINT('Ctrl Pts',(-37.1906201279053,-16.3621201809922,
-8.73670574471494));
#31348=CARTESIAN_POINT('Ctrl Pts',(-39.4840611441388,-17.6857598217545,
-11.3734544105501));
#31349=CARTESIAN_POINT('Ctrl Pts',(-40.8595741644358,-18.4474896113692,
-12.4221714958517));
#31350=CARTESIAN_POINT('Ctrl Pts',(-43.899882870338,-20.1169735923676,-13.854590909534));
#31351=CARTESIAN_POINT('Ctrl Pts',(-45.5316698257921,-20.9956349957552,
-14.2195188101196));
#31352=CARTESIAN_POINT('Ctrl Pts',(-47.1721284105873,-21.8833834324347,
-14.2201291128084));
#31353=CARTESIAN_POINT('Ctrl Pts',(-33.8713086176152,-16.7773762111442,
0.));
#31354=CARTESIAN_POINT('Ctrl Pts',(-33.8192589011655,-16.8929361804564,
-1.86858636180863));
#31355=CARTESIAN_POINT('Ctrl Pts',(-34.1010104999369,-17.1543030074678,
-3.71029995871351));
#31356=CARTESIAN_POINT('Ctrl Pts',(-35.2977744483822,-17.9818681105444,
-7.16936247492166));
#31357=CARTESIAN_POINT('Ctrl Pts',(-36.2012418527657,-18.5280220222852,
-8.73699595772984));
#31358=CARTESIAN_POINT('Ctrl Pts',(-37.4649484236404,-19.2573188185412,
-10.1890856763468));
#31359=CARTESIAN_POINT('Ctrl Pts',(-37.5839834499235,-19.3256842021906,
-10.320392863511));
#31360=CARTESIAN_POINT('Ctrl Pts',(-37.7052869420397,-19.3950503475036,
-10.4488603765919));
#31361=CARTESIAN_POINT('Ctrl Pts',(-34.8604849513723,-14.6113821712782,
6.38378239159465E-15));
#31362=CARTESIAN_POINT('Ctrl Pts',(-34.8072346531258,-14.7263938532101,
-1.86860431101787));
#31363=CARTESIAN_POINT('Ctrl Pts',(-35.0914531001935,-14.9888871347756,
-3.70979114472567));
#31364=CARTESIAN_POINT('Ctrl Pts',(-36.2854639039658,-15.8151951688146,
-7.17014261466994));
#31365=CARTESIAN_POINT('Ctrl Pts',(-37.1906201279053,-16.3621201809922,
-8.73670574471494));
#31366=CARTESIAN_POINT('Ctrl Pts',(-38.4604391631867,-17.0949852513367,
-10.1966053555752));
#31367=CARTESIAN_POINT('Ctrl Pts',(-38.5861742181901,-17.1671818301296,
-10.3350231942337));
#31368=CARTESIAN_POINT('Ctrl Pts',(-38.7144417021566,-17.2404964639767,
-10.4702558451082));
#31369=CARTESIAN_POINT('Ctrl Pts',(-39.0798782217544,-21.5006126898293,
1.24689092472233));
#31370=CARTESIAN_POINT('Ctrl Pts',(-39.0385416232223,-21.5299876965017,
0.764254723795939));
#31371=CARTESIAN_POINT('Ctrl Pts',(-38.9985633313699,-21.5567767789462,
0.332948693683721));
#31372=CARTESIAN_POINT('Ctrl Pts',(-38.9323887326868,-21.7078468489021,
-0.978870002731641));
#31373=CARTESIAN_POINT('Ctrl Pts',(-39.0572850320307,-21.9062112228121,
-1.98783577086975));
#31374=CARTESIAN_POINT('Ctrl Pts',(-39.6445971746952,-22.4452850348649,
-3.80852727285524));
#31375=CARTESIAN_POINT('Ctrl Pts',(-40.1037270849374,-22.7952013801937,
-4.65544360729441));
#31376=CARTESIAN_POINT('Ctrl Pts',(-41.2708105092392,-23.6014590278078,
-6.04997283335897));
#31377=CARTESIAN_POINT('Ctrl Pts',(-41.9853438466739,-24.0680141309499,
-6.61832169900558));
#31378=CARTESIAN_POINT('Ctrl Pts',(-43.5424691073585,-25.0499869064575,
-7.36768403081101));
#31379=CARTESIAN_POINT('Ctrl Pts',(-44.4080651340567,-25.5868798182086,
-7.5713864865375));
#31380=CARTESIAN_POINT('Ctrl Pts',(-45.2447177621909,-26.1039819636367,
-7.56962581969439));
#31381=CARTESIAN_POINT('Ctrl Pts',(-37.707864724394,-19.569315945402,1.35489330510239));
#31382=CARTESIAN_POINT('Ctrl Pts',(-37.6675557657917,-19.5979606808283,
0.884255581219552));
#31383=CARTESIAN_POINT('Ctrl Pts',(-37.6238620982313,-19.6243717351791,
0.426396977907638));
#31384=CARTESIAN_POINT('Ctrl Pts',(-37.5562521484444,-19.7764631777536,
-1.25360819503831));
#31385=CARTESIAN_POINT('Ctrl Pts',(-37.7300898366018,-19.9945131659726,
-2.51960912778906));
#31386=CARTESIAN_POINT('Ctrl Pts',(-38.5050289449581,-20.6224119165131,
-4.84647586783176));
#31387=CARTESIAN_POINT('Ctrl Pts',(-39.1017118879154,-21.0330824745317,
-5.91572199051186));
#31388=CARTESIAN_POINT('Ctrl Pts',(-40.6166651990263,-21.9991307790679,
-7.69376028687524));
#31389=CARTESIAN_POINT('Ctrl Pts',(-41.5351982120125,-22.5567852866265,
-8.41063186556173));
#31390=CARTESIAN_POINT('Ctrl Pts',(-43.550429472657,-23.7511065841626,-9.37059840620446));
#31391=CARTESIAN_POINT('Ctrl Pts',(-44.6525338708919,-24.3935165948524,
-9.62435378606624));
#31392=CARTESIAN_POINT('Ctrl Pts',(-45.7374214437731,-25.0250626292175,
-9.62320046360548));
#31393=CARTESIAN_POINT('Ctrl Pts',(-35.9854902185572,-17.9434360021529,
1.47293201877987));
#31394=CARTESIAN_POINT('Ctrl Pts',(-35.9463021021891,-17.9712842340159,
1.01538097969052));
#31395=CARTESIAN_POINT('Ctrl Pts',(-35.8985773174064,-17.997293023891,0.52858075367214));
#31396=CARTESIAN_POINT('Ctrl Pts',(-35.8297588571567,-18.1506662116799,
-1.55402875459979));
#31397=CARTESIAN_POINT('Ctrl Pts',(-36.0565601177375,-18.3899895327109,
-3.1012143212414));
#31398=CARTESIAN_POINT('Ctrl Pts',(-37.0372859924679,-19.1152999068477,
-5.98129145450272));
#31399=CARTESIAN_POINT('Ctrl Pts',(-37.7840034012004,-19.592231806371,-7.29389406578866));
#31400=CARTESIAN_POINT('Ctrl Pts',(-39.6794872875132,-20.7330727614972,
-9.49113593801798));
#31401=CARTESIAN_POINT('Ctrl Pts',(-40.8208685319662,-21.3902415598682,
-10.3708286017221));
#31402=CARTESIAN_POINT('Ctrl Pts',(-43.3372861226137,-22.8168789077003,
-11.56040455612));
#31403=CARTESIAN_POINT('Ctrl Pts',(-44.6978537235209,-23.5745664065252,
-11.8694761540143));
#31404=CARTESIAN_POINT('Ctrl Pts',(-46.0542245204212,-24.331307334807,-11.8687142284812));
#31405=CARTESIAN_POINT('Ctrl Pts',(-33.9789464595043,-16.6854562787123,
1.5964707761032));
#31406=CARTESIAN_POINT('Ctrl Pts',(-33.9409293131115,-16.712472384756,1.15259170140102));
#31407=CARTESIAN_POINT('Ctrl Pts',(-33.8890125875502,-16.7380701329957,
0.635573044902023));
#31408=CARTESIAN_POINT('Ctrl Pts',(-33.8192589011655,-16.8929361804564,
-1.86858636180863));
#31409=CARTESIAN_POINT('Ctrl Pts',(-34.1010104999369,-17.1543030074678,
-3.71029995871351));
#31410=CARTESIAN_POINT('Ctrl Pts',(-35.2977744483822,-17.9818681105444,
-7.16936247492166));
#31411=CARTESIAN_POINT('Ctrl Pts',(-36.2012418527657,-18.5280220222852,
-8.73699595772984));
#31412=CARTESIAN_POINT('Ctrl Pts',(-38.4952930131949,-19.8519402484841,
-11.3730256981899));
#31413=CARTESIAN_POINT('Ctrl Pts',(-39.8698068706361,-20.6132138376926,
-12.4235805192373));
#31414=CARTESIAN_POINT('Ctrl Pts',(-42.9112302679262,-22.2832067364649,
-13.852947082145));
#31415=CARTESIAN_POINT('Ctrl Pts',(-44.542278745567,-23.1615116346235,-14.2204718555787));
#31416=CARTESIAN_POINT('Ctrl Pts',(-46.1829520838074,-24.0493774600892,
-14.2198708430667));
#31417=CARTESIAN_POINT('Ctrl Pts',(-34.9686592686579,-14.5197073364544,
1.59674373345257));
#31418=CARTESIAN_POINT('Ctrl Pts',(-34.9306549387506,-14.5467143347365,
1.15301430091077));
#31419=CARTESIAN_POINT('Ctrl Pts',(-34.8785972821108,-14.5722625852752,
0.635579150069985));
#31420=CARTESIAN_POINT('Ctrl Pts',(-34.8072346531258,-14.7263938532101,
-1.86860431101787));
#31421=CARTESIAN_POINT('Ctrl Pts',(-35.0914531001935,-14.9888871347744,
-3.70979114472567));
#31422=CARTESIAN_POINT('Ctrl Pts',(-36.2854639039658,-15.8151951688158,
-7.17014261466994));
#31423=CARTESIAN_POINT('Ctrl Pts',(-37.1906201279053,-16.3621201809898,
-8.73670574471733));
#31424=CARTESIAN_POINT('Ctrl Pts',(-39.4840611441388,-17.6857598217569,
-11.3734544105477));
#31425=CARTESIAN_POINT('Ctrl Pts',(-40.8595741644358,-18.4474896113716,
-12.4221714958517));
#31426=CARTESIAN_POINT('Ctrl Pts',(-43.899882870338,-20.1169735923652,-13.854590909534));
#31427=CARTESIAN_POINT('Ctrl Pts',(-45.5316698257919,-20.9956349957574,
-14.2195188101196));
#31428=CARTESIAN_POINT('Ctrl Pts',(-47.1721284105873,-21.8833834324347,
-14.2201291128084));
#31429=CARTESIAN_POINT('Ctrl Pts',(-37.2330519862577,-15.2134465003402,
1.47327608945385));
#31430=CARTESIAN_POINT('Ctrl Pts',(-37.1938800254351,-15.241283251608,1.01591367865882));
#31431=CARTESIAN_POINT('Ctrl Pts',(-37.1459775929371,-15.2672296481901,
0.528588449413829));
#31432=CARTESIAN_POINT('Ctrl Pts',(-37.0751310137706,-15.4196766250222,
-1.55405138009984));
#31433=CARTESIAN_POINT('Ctrl Pts',(-37.3050418083478,-15.6604198747703,
-3.10057294641723));
#31434=CARTESIAN_POINT('Ctrl Pts',(-38.2822972641641,-16.3841456768376,
-5.98227484333557));
#31435=CARTESIAN_POINT('Ctrl Pts',(-39.031143479052,-16.8620495708756,-7.29352824384753));
#31436=CARTESIAN_POINT('Ctrl Pts',(-40.9258582608669,-18.0025393609684,
-9.49167634241016));
#31437=CARTESIAN_POINT('Ctrl Pts',(-42.0684989791458,-18.6602832132111,
-10.369052486778));
#31438=CARTESIAN_POINT('Ctrl Pts',(-44.5835114688962,-20.0862790553914,
-11.5624766483363));
#31439=CARTESIAN_POINT('Ctrl Pts',(-45.945008519911,-20.8444200113532,-11.8682745707305));
#31440=CARTESIAN_POINT('Ctrl Pts',(-47.3011100364938,-21.6010088957271,
-11.8690397849987));
#31441=CARTESIAN_POINT('Ctrl Pts',(-39.5896190563861,-15.4515482289401,
1.35541228259756));
#31442=CARTESIAN_POINT('Ctrl Pts',(-39.5493344659456,-15.4801756476575,
0.885059075375416));
#31443=CARTESIAN_POINT('Ctrl Pts',(-39.5053728442148,-15.506492591361,0.42640858574592));
#31444=CARTESIAN_POINT('Ctrl Pts',(-39.4347037901406,-15.6571869876943,
-1.25364232211228));
#31445=CARTESIAN_POINT('Ctrl Pts',(-39.6132317302865,-15.8773787191765,
-2.51864171288157));
#31446=CARTESIAN_POINT('Ctrl Pts',(-40.3829362474672,-16.5028873873736,
-4.84795915807232));
#31447=CARTESIAN_POINT('Ctrl Pts',(-40.9828301658835,-16.9150240490638,
-5.91517020459162));
#31448=CARTESIAN_POINT('Ctrl Pts',(-42.4966234015636,-17.8805426753577,
-7.69457540347142));
#31449=CARTESIAN_POINT('Ctrl Pts',(-43.4170561364076,-18.4390645629071,
-8.40795287035897));
#31450=CARTESIAN_POINT('Ctrl Pts',(-45.4301680192413,-19.6324182482015,
-9.37372383743044));
#31451=CARTESIAN_POINT('Ctrl Pts',(-46.5336710320569,-20.2755208514245,
-9.62254086027733));
#31452=CARTESIAN_POINT('Ctrl Pts',(-47.618155754582,-20.9068289285809,-9.62369151535378));
#31453=CARTESIAN_POINT('Ctrl Pts',(-41.9477963710448,-15.224862147993,1.24768188077444));
#31454=CARTESIAN_POINT('Ctrl Pts',(-41.9064969112055,-15.2542107628561,
0.76547930207016));
#31455=CARTESIAN_POINT('Ctrl Pts',(-41.8661102394621,-15.2808564144436,
0.332966384797566));
#31456=CARTESIAN_POINT('Ctrl Pts',(-41.795273363368,-15.429797293463,-0.978922014651145));
#31457=CARTESIAN_POINT('Ctrl Pts',(-41.9273179171823,-15.6314258258578,
-1.98636136652118));
#31458=CARTESIAN_POINT('Ctrl Pts',(-42.5066521964273,-16.1668569942327,
-3.81078790535555));
#31459=CARTESIAN_POINT('Ctrl Pts',(-42.9706758457924,-16.519007778584,-4.654602649028));
#31460=CARTESIAN_POINT('Ctrl Pts',(-44.1359912383645,-17.3244581615128,
-6.05121512500453));
#31461=CARTESIAN_POINT('Ctrl Pts',(-44.853419877635,-17.7923352091663,-6.61423873300694));
#31462=CARTESIAN_POINT('Ctrl Pts',(-46.4073150662767,-18.7728332795684,
-7.37244739485722));
#31463=CARTESIAN_POINT('Ctrl Pts',(-47.275034524054,-19.3108003961669,-7.56862230213317));
#31464=CARTESIAN_POINT('Ctrl Pts',(-48.1110813316861,-19.827521231076,-7.57037421505994));
#31465=CARTESIAN_POINT('Ctrl Pts',(-36.007677782744,-11.6799141290249,1.59647068126645));
#31466=CARTESIAN_POINT('Ctrl Pts',(-35.9738923911276,-11.7120656519311,
1.15259163660754));
#31467=CARTESIAN_POINT('Ctrl Pts',(-35.9261470465067,-11.7447913705128,
0.635573001841871));
#31468=CARTESIAN_POINT('Ctrl Pts',(-35.8791430893777,-11.9080080866994,
-1.86858636174462));
#31469=CARTESIAN_POINT('Ctrl Pts',(-36.1952232408322,-12.1266171430312,
-3.71029995867732));
#31470=CARTESIAN_POINT('Ctrl Pts',(-37.4975806517,-12.775441558893,-7.1693624749576));
#31471=CARTESIAN_POINT('Ctrl Pts',(-38.469577866188,-13.1874595938152,-8.73699595771281));
#31472=CARTESIAN_POINT('Ctrl Pts',(-40.9286921018457,-14.17142472135,-11.3730256982067));
#31473=CARTESIAN_POINT('Ctrl Pts',(-42.3975559177885,-14.7293359258714,
-12.4235805192177));
#31474=CARTESIAN_POINT('Ctrl Pts',(-45.6456867796162,-15.9494910259031,
-13.8529470821644));
#31475=CARTESIAN_POINT('Ctrl Pts',(-47.3851293551721,-16.5867336459591,
-14.2204718556976));
#31476=CARTESIAN_POINT('Ctrl Pts',(-49.1354594857179,-17.2320701170946,
-14.2198708430666));
#31477=CARTESIAN_POINT('Ctrl Pts',(-35.6055008474196,-10.8171551228318,
1.62964612287405));
#31478=CARTESIAN_POINT('Ctrl Pts',(-35.5719973186168,-10.8490384138699,
1.18947024666155));
#31479=CARTESIAN_POINT('Ctrl Pts',(-35.5230856250742,-10.8818072974723,
0.664243958022171));
#31480=CARTESIAN_POINT('Ctrl Pts',(-35.47544064564,-11.0453235253696,-1.95287905124124));
#31481=CARTESIAN_POINT('Ctrl Pts',(-35.8076256583572,-11.2678861931963,
-3.87337387076198));
#31482=CARTESIAN_POINT('Ctrl Pts',(-37.1704123385762,-11.9353671582147,
-7.48792130216354));
#31483=CARTESIAN_POINT('Ctrl Pts',(-38.1870962603682,-12.3599059967852,
-9.12360836231895));
#31484=CARTESIAN_POINT('Ctrl Pts',(-40.7587332590465,-13.3771794922095,
-11.8774049927121));
#31485=CARTESIAN_POINT('Ctrl Pts',(-42.2936801020475,-13.9538940422505,
-12.9732563608771));
#31486=CARTESIAN_POINT('Ctrl Pts',(-45.6900265604505,-15.2184820528514,
-14.4676858045575));
#31487=CARTESIAN_POINT('Ctrl Pts',(-47.5060156561304,-15.8774655648083,
-14.8501851005579));
#31488=CARTESIAN_POINT('Ctrl Pts',(-49.3366907261818,-16.5467173899503,
-14.8499483202528));
#31489=CARTESIAN_POINT('Ctrl Pts',(-35.8740691471581,-9.90333289917197,
1.6297553058138));
#31490=CARTESIAN_POINT('Ctrl Pts',(-35.8405701742826,-9.93521185459824,
1.18963928645476));
#31491=CARTESIAN_POINT('Ctrl Pts',(-35.7915998644032,-9.96796916327536,
0.664246400093167));
#31492=CARTESIAN_POINT('Ctrl Pts',(-35.7432760306098,-10.1312860615242,
-1.95288623093664));
#31493=CARTESIAN_POINT('Ctrl Pts',(-36.0765018635479,-10.3541542972557,
-3.87317034516857));
#31494=CARTESIAN_POINT('Ctrl Pts',(-37.4381269352784,-11.0212942780522,
-7.48823335806122));
#31495=CARTESIAN_POINT('Ctrl Pts',(-38.4555234045969,-11.4460422796819,
-9.12349227712835));
#31496=CARTESIAN_POINT('Ctrl Pts',(-41.0269029710421,-12.4632402082154,
-11.877576477641));
#31497=CARTESIAN_POINT('Ctrl Pts',(-42.5622713807909,-13.0400785027476,
-12.9726927515335));
#31498=CARTESIAN_POINT('Ctrl Pts',(-45.9581475304014,-14.3045284731053,
-14.4683433355027));
#31499=CARTESIAN_POINT('Ctrl Pts',(-47.7744493565958,-14.9636108095647,
-14.8498038985338));
#31500=CARTESIAN_POINT('Ctrl Pts',(-49.6050326655023,-15.6328286697391,
-14.8500516281495));
#31501=CARTESIAN_POINT('Ctrl Pts',(-36.6790985320904,-9.39535856987525,
1.59674363861582));
#31502=CARTESIAN_POINT('Ctrl Pts',(-36.6453245303195,-9.42749925374606,
1.15301423608824));
#31503=CARTESIAN_POINT('Ctrl Pts',(-36.5974326448229,-9.46019603501911,
0.635579107019359));
#31504=CARTESIAN_POINT('Ctrl Pts',(-36.5487315518213,-9.62291442708968,
-1.86860431098312));
#31505=CARTESIAN_POINT('Ctrl Pts',(-36.8674137538258,-9.84228740318107,
-3.70979114469078));
#31506=CARTESIAN_POINT('Ctrl Pts',(-38.1668671434388,-10.4902593584854,
-7.17014261470479));
#31507=CARTESIAN_POINT('Ctrl Pts',(-39.1406457267621,-10.902800301061,-8.73670574473392));
#31508=CARTESIAN_POINT('Ctrl Pts',(-41.5991163818324,-11.8865765113604,
-11.3734544105312));
#31509=CARTESIAN_POINT('Ctrl Pts',(-43.0690341146564,-12.4447970771118,
-12.4221714958467));
#31510=CARTESIAN_POINT('Ctrl Pts',(-46.3159892044841,-13.6646070765402,
-13.8545909095391));
#31511=CARTESIAN_POINT('Ctrl Pts',(-48.0562134772108,-14.3020974767622,
-14.2195188099628));
#31512=CARTESIAN_POINT('Ctrl Pts',(-49.8063143340192,-14.9473483165667,
-14.2201291128084));
#31513=CARTESIAN_POINT('Ctrl Pts',(-35.914217116421,-11.7862169042732,0.));
#31514=CARTESIAN_POINT('Ctrl Pts',(-35.8791430893777,-11.9080080866994,
-1.86858636174462));
#31515=CARTESIAN_POINT('Ctrl Pts',(-36.1952232408322,-12.1266171430312,
-3.71029995867732));
#31516=CARTESIAN_POINT('Ctrl Pts',(-37.4975806517,-12.775441558893,-7.1693624749576));
#31517=CARTESIAN_POINT('Ctrl Pts',(-38.469577866188,-13.1874595938152,-8.73699595771042));
#31518=CARTESIAN_POINT('Ctrl Pts',(-39.8242114819221,-13.7294890038935,
-10.1890856763483));
#31519=CARTESIAN_POINT('Ctrl Pts',(-39.9517643117907,-13.7802180759912,
-10.3203928635135));
#31520=CARTESIAN_POINT('Ctrl Pts',(-40.0817049410149,-13.8316148870952,
-10.4488603765949));
#31521=CARTESIAN_POINT('Ctrl Pts',(-36.5850719698905,-9.5014950906651,-3.88578058618805E-16));
#31522=CARTESIAN_POINT('Ctrl Pts',(-36.5487315518213,-9.62291442708968,
-1.86860431098312));
#31523=CARTESIAN_POINT('Ctrl Pts',(-36.8674137538258,-9.84228740318107,
-3.70979114469078));
#31524=CARTESIAN_POINT('Ctrl Pts',(-38.1668671434388,-10.4902593584854,
-7.17014261470479));
#31525=CARTESIAN_POINT('Ctrl Pts',(-39.1406457267621,-10.902800301061,-8.73670574473392));
#31526=CARTESIAN_POINT('Ctrl Pts',(-40.5018374092127,-11.4474917709757,
-10.1966053555729));
#31527=CARTESIAN_POINT('Ctrl Pts',(-40.6365673070899,-11.5010595286717,
-10.3350231942294));
#31528=CARTESIAN_POINT('Ctrl Pts',(-40.7739629732778,-11.5553735590168,
-10.4702558451022));
#31529=CARTESIAN_POINT('Ctrl Pts',(-41.7419576204996,-15.7201209119709,
1.24689082988559));
#31530=CARTESIAN_POINT('Ctrl Pts',(-41.7052222707547,-15.7550797323953,
0.764254661700912));
#31531=CARTESIAN_POINT('Ctrl Pts',(-41.6694633881739,-15.7872856429804,
0.332948671129863));
#31532=CARTESIAN_POINT('Ctrl Pts',(-41.625461864821,-15.9462356620226,-0.978870002708281));
#31533=CARTESIAN_POINT('Ctrl Pts',(-41.777317093697,-16.124806375996,-1.98783577088221));
#31534=CARTESIAN_POINT('Ctrl Pts',(-42.435369447998,-16.574809961301,-3.80852727284257));
#31535=CARTESIAN_POINT('Ctrl Pts',(-42.9396243659164,-16.8558236638087,
-4.65544360725108));
#31536=CARTESIAN_POINT('Ctrl Pts',(-44.2095709903314,-17.4877814824203,
-6.04997283340197));
#31537=CARTESIAN_POINT('Ctrl Pts',(-44.9832291228107,-17.8478990309026,
-6.6183216989813));
#31538=CARTESIAN_POINT('Ctrl Pts',(-46.6642543902183,-18.5982747098319,
-7.36768403083496));
#31539=CARTESIAN_POINT('Ctrl Pts',(-47.5974477252332,-19.0065156676779,
-7.57138648693225));
#31540=CARTESIAN_POINT('Ctrl Pts',(-48.4991757443115,-19.3992863750338,
-7.56962581969416));
#31541=CARTESIAN_POINT('Ctrl Pts',(-40.1090570584212,-14.0037398626876,
1.35489321026565));
#31542=CARTESIAN_POINT('Ctrl Pts',(-40.0732349602028,-14.0378295966248,
0.884255518285778));
#31543=CARTESIAN_POINT('Ctrl Pts',(-40.0337447201299,-14.0701900799496,
0.426396949023618));
#31544=CARTESIAN_POINT('Ctrl Pts',(-39.9884678119751,-14.2303553472505,
-1.2536081950084));
#31545=CARTESIAN_POINT('Ctrl Pts',(-40.1915678319234,-14.4214462185192,
-2.51960912778971));
#31546=CARTESIAN_POINT('Ctrl Pts',(-41.0479784866769,-14.9326685312541,
-4.84647586783093));
#31547=CARTESIAN_POINT('Ctrl Pts',(-41.6970325717046,-15.2542422185918,
-5.91572199048531));
#31548=CARTESIAN_POINT('Ctrl Pts',(-43.3340488506278,-15.994857208877,-7.69376028690158));
#31549=CARTESIAN_POINT('Ctrl Pts',(-44.322595033069,-16.4161147204105,-8.41063186553746));
#31550=CARTESIAN_POINT('Ctrl Pts',(-46.4872837874829,-17.3114822382755,
-9.37059840622849));
#31551=CARTESIAN_POINT('Ctrl Pts',(-47.6695948287912,-17.7905076322675,
-9.624353786323));
#31552=CARTESIAN_POINT('Ctrl Pts',(-48.8333181822473,-18.2612298390049,
-9.62320046360533));
#31553=CARTESIAN_POINT('Ctrl Pts',(-38.1728270004195,-12.6395284821798,
1.47293192394313));
#31554=CARTESIAN_POINT('Ctrl Pts',(-38.1380009815277,-12.6726703073981,
1.01538091584584));
#31555=CARTESIAN_POINT('Ctrl Pts',(-38.0944634070467,-12.7052063084716,
0.528580717863993));
#31556=CARTESIAN_POINT('Ctrl Pts',(-38.0481727007017,-12.8668122636162,
-1.55402875455616));
#31557=CARTESIAN_POINT('Ctrl Pts',(-38.3067247111946,-13.0714224335838,
-3.10121432122184));
#31558=CARTESIAN_POINT('Ctrl Pts',(-39.3806906392157,-13.6497783496959,
-5.98129145452209));
#31559=CARTESIAN_POINT('Ctrl Pts',(-40.1876820275573,-14.0155868029206,
-7.29389406576927));
#31560=CARTESIAN_POINT('Ctrl Pts',(-42.2262312169725,-14.8750601592863,
-9.4911359380372));
#31561=CARTESIAN_POINT('Ctrl Pts',(-43.4495197173534,-15.36310443968,-10.3708286017026));
#31562=CARTESIAN_POINT('Ctrl Pts',(-46.1433554687509,-16.4170971138883,
-11.5604045561393));
#31563=CARTESIAN_POINT('Ctrl Pts',(-47.5979046271491,-16.9734434882789,
-11.8694761541855));
#31564=CARTESIAN_POINT('Ctrl Pts',(-49.0481649878422,-17.5294501945615,
-11.8687142284811));
#31565=CARTESIAN_POINT('Ctrl Pts',(-36.007677782744,-11.6799141290249,1.59647068126645));
#31566=CARTESIAN_POINT('Ctrl Pts',(-35.9738923911276,-11.7120656519311,
1.15259163660754));
#31567=CARTESIAN_POINT('Ctrl Pts',(-35.9261470465067,-11.7447913705128,
0.635573001841871));
#31568=CARTESIAN_POINT('Ctrl Pts',(-35.8791430893777,-11.9080080866994,
-1.86858636174462));
#31569=CARTESIAN_POINT('Ctrl Pts',(-36.1952232408322,-12.1266171430312,
-3.71029995867732));
#31570=CARTESIAN_POINT('Ctrl Pts',(-37.4975806517,-12.775441558893,-7.1693624749576));
#31571=CARTESIAN_POINT('Ctrl Pts',(-38.469577866188,-13.1874595938152,-8.73699595771042));
#31572=CARTESIAN_POINT('Ctrl Pts',(-40.9286921018457,-14.17142472135,-11.3730256982091));
#31573=CARTESIAN_POINT('Ctrl Pts',(-42.3975559177885,-14.7293359258726,
-12.4235805192177));
#31574=CARTESIAN_POINT('Ctrl Pts',(-45.6456867796163,-15.9494910259019,
-13.8529470821644));
#31575=CARTESIAN_POINT('Ctrl Pts',(-47.3851293551747,-16.5867336459529,
-14.2204718556976));
#31576=CARTESIAN_POINT('Ctrl Pts',(-49.1354594857179,-17.2320701170946,
-14.2198708430666));
#31577=CARTESIAN_POINT('Ctrl Pts',(-36.6790985320904,-9.39535856987524,
1.59674363861582));
#31578=CARTESIAN_POINT('Ctrl Pts',(-36.6453245303195,-9.42749925374605,
1.15301423608824));
#31579=CARTESIAN_POINT('Ctrl Pts',(-36.5974326448229,-9.46019603501911,
0.635579107019359));
#31580=CARTESIAN_POINT('Ctrl Pts',(-36.5487315518213,-9.62291442708968,
-1.86860431098312));
#31581=CARTESIAN_POINT('Ctrl Pts',(-36.8674137538258,-9.84228740318107,
-3.70979114469079));
#31582=CARTESIAN_POINT('Ctrl Pts',(-38.1668671434388,-10.4902593584854,
-7.17014261470479));
#31583=CARTESIAN_POINT('Ctrl Pts',(-39.1406457267669,-10.902800301061,-8.73670574473393));
#31584=CARTESIAN_POINT('Ctrl Pts',(-41.5991163818276,-11.8865765113604,
-11.3734544105312));
#31585=CARTESIAN_POINT('Ctrl Pts',(-43.0690341146515,-12.4447970771106,
-12.4221714958515));
#31586=CARTESIAN_POINT('Ctrl Pts',(-46.3159892044889,-13.6646070765414,
-13.8545909095343));
#31587=CARTESIAN_POINT('Ctrl Pts',(-48.0562134772077,-14.3020974767599,
-14.2195188099628));
#31588=CARTESIAN_POINT('Ctrl Pts',(-49.8063143340192,-14.9473483165667,
-14.2201291128085));
#31589=CARTESIAN_POINT('Ctrl Pts',(-39.019172373722,-9.7597797859694,1.47327599461711));
#31590=CARTESIAN_POINT('Ctrl Pts',(-38.9843607120683,-9.79290794827359,
1.01591361477635));
#31591=CARTESIAN_POINT('Ctrl Pts',(-38.940638418548,-9.82540747302369,0.528588413617701));
#31592=CARTESIAN_POINT('Ctrl Pts',(-38.8922084230933,-9.98638527613126,
-1.55405138009309));
#31593=CARTESIAN_POINT('Ctrl Pts',(-39.1540403939526,-10.1919583891645,
-3.10057294640141));
#31594=CARTESIAN_POINT('Ctrl Pts',(-40.2243457187586,-10.7692397539638,
-5.98227484335149));
#31595=CARTESIAN_POINT('Ctrl Pts',(-41.0335825742976,-11.1357073474839,
-7.29352824387615));
#31596=CARTESIAN_POINT('Ctrl Pts',(-43.071320511685,-11.9949425681867,-9.4916763423817));
#31597=CARTESIAN_POINT('Ctrl Pts',(-44.2959375049236,-12.4833768074015,
-10.3690524867827));
#31598=CARTESIAN_POINT('Ctrl Pts',(-46.9882911615408,-13.5369344722681,
-11.5624766483318));
#31599=CARTESIAN_POINT('Ctrl Pts',(-48.4438248432715,-14.0935974137185,
-11.8682745705641));
#31600=CARTESIAN_POINT('Ctrl Pts',(-49.8937970264261,-14.6494919462611,
-11.8690397849988));
#31601=CARTESIAN_POINT('Ctrl Pts',(-41.3856383979639,-9.66008352082097,
1.35541218776083));
#31602=CARTESIAN_POINT('Ctrl Pts',(-41.3498379554194,-9.69415264636012,
0.885059012386286));
#31603=CARTESIAN_POINT('Ctrl Pts',(-41.3100690951961,-9.72645811078408,
0.426408556880046));
#31604=CARTESIAN_POINT('Ctrl Pts',(-41.2615653996735,-9.88567590770738,
-1.25364232213799));
#31605=CARTESIAN_POINT('Ctrl Pts',(-41.4696127334847,-10.0782192299367,
-2.51864171288723));
#31606=CARTESIAN_POINT('Ctrl Pts',(-42.3205019334041,-10.5878207479002,
-4.84795915806691));
#31607=CARTESIAN_POINT('Ctrl Pts',(-42.9729429590492,-10.9103886466196,
-5.91517020462989));
#31608=CARTESIAN_POINT('Ctrl Pts',(-44.6087355895268,-11.6506444460178,
-7.69457540343341));
#31609=CARTESIAN_POINT('Ctrl Pts',(-45.5992855983476,-12.0724901502325,
-8.4079528703733));
#31610=CARTESIAN_POINT('Ctrl Pts',(-47.7617388416023,-12.9672015236625,
-9.37372383741637));
#31611=CARTESIAN_POINT('Ctrl Pts',(-48.9455328277903,-13.446713416981,-9.62254086002058));
#31612=CARTESIAN_POINT('Ctrl Pts',(-50.1088235664895,-13.9172574201605,
-9.62369151535393));
#31613=CARTESIAN_POINT('Ctrl Pts',(-43.6875520748214,-9.100101154168,1.24768178593771));
#31614=CARTESIAN_POINT('Ctrl Pts',(-43.6508497297522,-9.13502856602996,
0.765479239891048));
#31615=CARTESIAN_POINT('Ctrl Pts',(-43.6146662116282,-9.1671506241679,0.332966362271342));
#31616=CARTESIAN_POINT('Ctrl Pts',(-43.5657468507465,-9.32465663564633,
-0.978922014712551));
#31617=CARTESIAN_POINT('Ctrl Pts',(-43.7251421134098,-9.50544098101819,
-1.98636136653877));
#31618=CARTESIAN_POINT('Ctrl Pts',(-44.3747794050838,-9.95297436781101,
-3.81078790533841));
#31619=CARTESIAN_POINT('Ctrl Pts',(-44.8841962446822,-10.2355033142702,
-4.6546026490903));
#31620=CARTESIAN_POINT('Ctrl Pts',(-46.1522779478725,-10.8669137021975,
-6.05121512494264));
#31621=CARTESIAN_POINT('Ctrl Pts',(-46.9289900443881,-11.2279276952588,
-6.61423873304056));
#31622=CARTESIAN_POINT('Ctrl Pts',(-48.6066082448179,-11.9773033666356,
-7.37244739482399));
#31623=CARTESIAN_POINT('Ctrl Pts',(-49.5420562727445,-12.3863053996863,
-7.56862230172892));
#31624=CARTESIAN_POINT('Ctrl Pts',(-50.4431303715412,-12.7787848949965,
-7.57037421506017));
#31625=CARTESIAN_POINT('Ctrl Pts',(-37.3033966274914,-6.43660260973375,
1.59647061166179));
#31626=CARTESIAN_POINT('Ctrl Pts',(-37.2745307626585,-6.47323503721974,
1.15259158903741));
#31627=CARTESIAN_POINT('Ctrl Pts',(-37.2319287549561,-6.51242252436172,
0.635572970257452));
#31628=CARTESIAN_POINT('Ctrl Pts',(-37.2086313911891,-6.68066728817659,
-1.86858636175417));
#31629=CARTESIAN_POINT('Ctrl Pts',(-37.5526056149658,-6.85206832389808,
-3.71029995869313));
#31630=CARTESIAN_POINT('Ctrl Pts',(-38.9340442470254,-7.30894385837246,
-7.16936247494213));
#31631=CARTESIAN_POINT('Ctrl Pts',(-39.9547842113923,-7.57843851744686,
-8.73699595769433));
#31632=CARTESIAN_POINT('Ctrl Pts',(-42.5289010478687,-8.20241985396338,
-11.3730256982255));
#31633=CARTESIAN_POINT('Ctrl Pts',(-44.0622129909323,-8.54561121037124,
-12.4235805192426));
#31634=CARTESIAN_POINT('Ctrl Pts',(-47.4509287397419,-9.2910896727123,-13.8529470821398));
#31635=CARTESIAN_POINT('Ctrl Pts',(-49.2633553782971,-9.67429759299236,
-14.2204718555978));
#31636=CARTESIAN_POINT('Ctrl Pts',(-51.0877106274638,-10.063967519702,-14.2198708430667));
#31637=CARTESIAN_POINT('Ctrl Pts',(-36.7825298650421,-5.63986099173596,
1.62964605326941));
#31638=CARTESIAN_POINT('Ctrl Pts',(-36.7539048206774,-5.67618780432318,
1.18947019889892));
#31639=CARTESIAN_POINT('Ctrl Pts',(-36.7101544788345,-5.7155840058739,0.664243925013534));
#31640=CARTESIAN_POINT('Ctrl Pts',(-36.6862652424053,-5.88421645978634,
-1.95287905125288));
#31641=CARTESIAN_POINT('Ctrl Pts',(-37.0467430607447,-6.05723890421492,
-3.87337387078137));
#31642=CARTESIAN_POINT('Ctrl Pts',(-38.4906509831416,-6.5239811093709,-7.48792130214445));
#31643=CARTESIAN_POINT('Ctrl Pts',(-39.5574047046893,-6.79950954685142,
-9.12360836230283));
#31644=CARTESIAN_POINT('Ctrl Pts',(-42.2476392596962,-7.44044656127135,
-11.8774049927284));
#31645=CARTESIAN_POINT('Ctrl Pts',(-43.8490375949647,-7.79284527693345,
-12.9732563608876));
#31646=CARTESIAN_POINT('Ctrl Pts',(-47.3907837817603,-8.56121110825465,
-14.4676858045473));
#31647=CARTESIAN_POINT('Ctrl Pts',(-49.2820718587483,-8.9550449238883,-14.8501851004961));
#31648=CARTESIAN_POINT('Ctrl Pts',(-51.1893577615276,-9.3569525036808,-14.8499483202528));
#31649=CARTESIAN_POINT('Ctrl Pts',(-36.918314064762,-4.69711890654748,1.62975523620919));
#31650=CARTESIAN_POINT('Ctrl Pts',(-36.8896929129475,-4.73344077927094,
1.18963923868388));
#31651=CARTESIAN_POINT('Ctrl Pts',(-36.8458829040885,-4.77283386569197,
0.664246367084094));
#31652=CARTESIAN_POINT('Ctrl Pts',(-36.8212933554976,-4.94136562989336,
-1.95288623094736));
#31653=CARTESIAN_POINT('Ctrl Pts',(-37.1828448868644,-5.11454240782316,
-3.87317034518908));
#31654=CARTESIAN_POINT('Ctrl Pts',(-38.6255544971456,-5.58111241361319,
-7.48823335804086));
#31655=CARTESIAN_POINT('Ctrl Pts',(-39.6930432805175,-5.85674647908712,
-9.12349227711692));
#31656=CARTESIAN_POINT('Ctrl Pts',(-42.3830122693083,-6.49764533220352,
-11.8775764776524));
#31657=CARTESIAN_POINT('Ctrl Pts',(-43.9848454910638,-6.85010653761332,
-12.9726927515151));
#31658=CARTESIAN_POINT('Ctrl Pts',(-47.5261065109321,-7.61840266566205,
-14.4683433355211));
#31659=CARTESIAN_POINT('Ctrl Pts',(-49.4177181995047,-8.01228979371233,
-14.8498038985148));
#31660=CARTESIAN_POINT('Ctrl Pts',(-51.3249084414063,-8.41417681322632,
-14.8500516281495));
#31661=CARTESIAN_POINT('Ctrl Pts',(-37.6428571267913,-4.07974739676256,
1.59674356901123));
#31662=CARTESIAN_POINT('Ctrl Pts',(-37.6140009933228,-4.11636747458817,
1.15301418850057));
#31663=CARTESIAN_POINT('Ctrl Pts',(-37.5712498180903,-4.15554717390732,
0.635579075433858));
#31664=CARTESIAN_POINT('Ctrl Pts',(-37.5462016739223,-4.32354021344296,
-1.86860431099037));
#31665=CARTESIAN_POINT('Ctrl Pts',(-37.8928601802435,-4.4953270829205,-3.70979114471123));
#31666=CARTESIAN_POINT('Ctrl Pts',(-39.2713030320569,-4.95177211897637,
-7.17014261468437));
#31667=CARTESIAN_POINT('Ctrl Pts',(-40.2938806509817,-5.22153084803759,
-8.73670574472958));
#31668=CARTESIAN_POINT('Ctrl Pts',(-42.8673335718798,-5.84541678129231,
-11.3734544105354));
#31669=CARTESIAN_POINT('Ctrl Pts',(-44.4017327311728,-6.18876436207153,
-12.4221714958137));
#31670=CARTESIAN_POINT('Ctrl Pts',(-47.7892355626787,-6.93406856623023,
-13.8545909095719));
#31671=CARTESIAN_POINT('Ctrl Pts',(-49.6024712046778,-7.31741049752272,
-14.219518810015));
#31672=CARTESIAN_POINT('Ctrl Pts',(-51.4265873271606,-7.70702829356582,
-14.2201291128083));
#31673=CARTESIAN_POINT('Ctrl Pts',(-37.2260157227863,-6.55512420987395,
0.));
#31674=CARTESIAN_POINT('Ctrl Pts',(-37.2086313911891,-6.6806672881766,-1.86858636175417));
#31675=CARTESIAN_POINT('Ctrl Pts',(-37.5526056149658,-6.85206832389809,
-3.71029995869313));
#31676=CARTESIAN_POINT('Ctrl Pts',(-38.9340442470254,-7.30894385837246,
-7.16936247494213));
#31677=CARTESIAN_POINT('Ctrl Pts',(-39.9547842113923,-7.57843851744686,
-8.73699595769433));
#31678=CARTESIAN_POINT('Ctrl Pts',(-41.3727684379707,-7.92216638570902,
-10.1890856763496));
#31679=CARTESIAN_POINT('Ctrl Pts',(-41.5062424636379,-7.95422644864132,
-10.320392863516));
#31680=CARTESIAN_POINT('Ctrl Pts',(-41.6421750134749,-7.98660763468004,
-10.4488603765984));
#31681=CARTESIAN_POINT('Ctrl Pts',(-37.5648924257372,-4.19818497005525,
2.22044604925031E-16));
#31682=CARTESIAN_POINT('Ctrl Pts',(-37.5462016739223,-4.32354021344296,
-1.86860431099037));
#31683=CARTESIAN_POINT('Ctrl Pts',(-37.8928601802435,-4.4953270829205,-3.70979114471123));
#31684=CARTESIAN_POINT('Ctrl Pts',(-39.2713030320569,-4.95177211897637,
-7.17014261468437));
#31685=CARTESIAN_POINT('Ctrl Pts',(-40.2938806509817,-5.22153084803759,
-8.73670574472958));
#31686=CARTESIAN_POINT('Ctrl Pts',(-41.7187350432356,-5.56696037000185,
-10.196605355573));
#31687=CARTESIAN_POINT('Ctrl Pts',(-41.8597170717902,-5.60080882153321,
-10.3350231942292));
#31688=CARTESIAN_POINT('Ctrl Pts',(-42.0034439406492,-5.63501657134766,
-10.4702558451014));
#31689=CARTESIAN_POINT('Ctrl Pts',(-43.5542911395532,-9.61961280540204,
1.24689076028084));
#31690=CARTESIAN_POINT('Ctrl Pts',(-43.5229048631346,-9.65944377882554,
0.764254616128654));
#31691=CARTESIAN_POINT('Ctrl Pts',(-43.4920933360729,-9.69641089756863,
0.332948654576497));
#31692=CARTESIAN_POINT('Ctrl Pts',(-43.4711606313199,-9.86000510219415,
-0.978870002690684));
#31693=CARTESIAN_POINT('Ctrl Pts',(-43.64688345522,-10.0151469714386,-1.98783577088957));
#31694=CARTESIAN_POINT('Ctrl Pts',(-44.3622799727875,-10.3669195547583,
-3.80852727283549));
#31695=CARTESIAN_POINT('Ctrl Pts',(-44.9013947224019,-10.5733099858333,
-4.65544360724204));
#31696=CARTESIAN_POINT('Ctrl Pts',(-46.2483520959889,-11.0181031366258,
-6.04997283341153));
#31697=CARTESIAN_POINT('Ctrl Pts',(-47.0653855748303,-11.2644521757634,
-6.61832169905394));
#31698=CARTESIAN_POINT('Ctrl Pts',(-48.8360900223873,-11.7679552730237,
-7.36768403076297));
#31699=CARTESIAN_POINT('Ctrl Pts',(-49.8178835406428,-12.0392336678774,
-7.57138648670422));
#31700=CARTESIAN_POINT('Ctrl Pts',(-50.7663303683512,-12.2996772587581,
-7.56962581969452));
#31701=CARTESIAN_POINT('Ctrl Pts',(-41.6937446593044,-8.15308801979197,
1.35489314066094));
#31702=CARTESIAN_POINT('Ctrl Pts',(-41.6631386548957,-8.191928783576,0.884255472092365));
#31703=CARTESIAN_POINT('Ctrl Pts',(-41.6286557481926,-8.2295799292397,0.426396927828607));
#31704=CARTESIAN_POINT('Ctrl Pts',(-41.6066335880859,-8.39455851882582,
-1.25360819499871));
#31705=CARTESIAN_POINT('Ctrl Pts',(-41.8348614091216,-8.55480021406848,
-2.51960912779946));
#31706=CARTESIAN_POINT('Ctrl Pts',(-42.755309558977,-8.93893907696394,-4.84647586782143));
#31707=CARTESIAN_POINT('Ctrl Pts',(-43.4435219166218,-9.16486958068287,
-5.91572199047626));
#31708=CARTESIAN_POINT('Ctrl Pts',(-45.1692762327319,-9.66497447127328,
-7.69376028691099));
#31709=CARTESIAN_POINT('Ctrl Pts',(-46.2077116350052,-9.94125939867522,
-8.41063186558134));
#31710=CARTESIAN_POINT('Ctrl Pts',(-48.4777910627081,-10.5194460361869,
-9.37059840618507));
#31711=CARTESIAN_POINT('Ctrl Pts',(-49.7162403037897,-10.8253352376767,
-9.62435378616625));
#31712=CARTESIAN_POINT('Ctrl Pts',(-50.9351093861917,-11.1256510703087,
-9.62320046360557));
#31713=CARTESIAN_POINT('Ctrl Pts',(-39.5830751094923,-7.07831661167196,
1.47293185433845));
#31714=CARTESIAN_POINT('Ctrl Pts',(-39.5533201442369,-7.11607735826761,
1.0153808689781));
#31715=CARTESIAN_POINT('Ctrl Pts',(-39.5148560779746,-7.15447823086432,
0.528580691593616));
#31716=CARTESIAN_POINT('Ctrl Pts',(-39.4920354699321,-7.32102712269281,
-1.55402875455564));
#31717=CARTESIAN_POINT('Ctrl Pts',(-39.7770748570174,-7.48675886860325,
-3.1012143212364));
#31718=CARTESIAN_POINT('Ctrl Pts',(-40.9224179890687,-7.90638666802899,
-5.98129145450779));
#31719=CARTESIAN_POINT('Ctrl Pts',(-41.7732553395368,-8.15362486974972,
-7.29389406576026));
#31720=CARTESIAN_POINT('Ctrl Pts',(-43.9133708492508,-8.71423422839074,
-9.49113593804649));
#31721=CARTESIAN_POINT('Ctrl Pts',(-45.1936639793565,-9.02321881658609,
-10.3708286017322));
#31722=CARTESIAN_POINT('Ctrl Pts',(-48.0100791640002,-9.68311056588415,
-11.5604045561101));
#31723=CARTESIAN_POINT('Ctrl Pts',(-49.5289994534967,-10.0267902081586,
-11.8694761540715));
#31724=CARTESIAN_POINT('Ctrl Pts',(-51.0436262593385,-10.3707439991146,
-11.8687142284813));
#31725=CARTESIAN_POINT('Ctrl Pts',(-37.3033966274914,-6.43660260973375,
1.59647061166179));
#31726=CARTESIAN_POINT('Ctrl Pts',(-37.2745307626585,-6.47323503721974,
1.15259158903741));
#31727=CARTESIAN_POINT('Ctrl Pts',(-37.2319287549561,-6.51242252436172,
0.635572970257452));
#31728=CARTESIAN_POINT('Ctrl Pts',(-37.2086313911891,-6.6806672881766,-1.86858636175417));
#31729=CARTESIAN_POINT('Ctrl Pts',(-37.5526056149658,-6.85206832389808,
-3.71029995869313));
#31730=CARTESIAN_POINT('Ctrl Pts',(-38.9340442470254,-7.30894385837246,
-7.16936247494213));
#31731=CARTESIAN_POINT('Ctrl Pts',(-39.9547842113923,-7.57843851744686,
-8.73699595769433));
#31732=CARTESIAN_POINT('Ctrl Pts',(-42.5289010478687,-8.2024198539634,-11.3730256982255));
#31733=CARTESIAN_POINT('Ctrl Pts',(-44.0622129909323,-8.54561121037124,
-12.4235805192426));
#31734=CARTESIAN_POINT('Ctrl Pts',(-47.4509287397419,-9.2910896727123,-13.8529470821398));
#31735=CARTESIAN_POINT('Ctrl Pts',(-49.263355378298,-9.67429759298781,-14.2204718555978));
#31736=CARTESIAN_POINT('Ctrl Pts',(-51.0877106274638,-10.063967519702,-14.2198708430667));
#31737=CARTESIAN_POINT('Ctrl Pts',(-37.6428571267913,-4.07974739676256,
1.59674356901123));
#31738=CARTESIAN_POINT('Ctrl Pts',(-37.6140009933228,-4.11636747458817,
1.15301418850057));
#31739=CARTESIAN_POINT('Ctrl Pts',(-37.5712498180903,-4.15554717390732,
0.635579075433858));
#31740=CARTESIAN_POINT('Ctrl Pts',(-37.5462016739223,-4.32354021344296,
-1.86860431099037));
#31741=CARTESIAN_POINT('Ctrl Pts',(-37.8928601802435,-4.4953270829205,-3.70979114471123));
#31742=CARTESIAN_POINT('Ctrl Pts',(-39.2713030320569,-4.95177211897636,
-7.17014261468437));
#31743=CARTESIAN_POINT('Ctrl Pts',(-40.2938806509817,-5.22153084803759,
-8.73670574472958));
#31744=CARTESIAN_POINT('Ctrl Pts',(-42.8673335718798,-5.84541678129231,
-11.3734544105354));
#31745=CARTESIAN_POINT('Ctrl Pts',(-44.4017327311728,-6.18876436207153,
-12.4221714958137));
#31746=CARTESIAN_POINT('Ctrl Pts',(-47.7892355626787,-6.93406856623022,
-13.8545909095719));
#31747=CARTESIAN_POINT('Ctrl Pts',(-49.6024712046779,-7.31741049752216,
-14.219518810015));
#31748=CARTESIAN_POINT('Ctrl Pts',(-51.4265873271606,-7.70702829356582,
-14.2201291128083));
#31749=CARTESIAN_POINT('Ctrl Pts',(-40.0109749372547,-4.10743210000935,
1.47327592501251));
#31750=CARTESIAN_POINT('Ctrl Pts',(-39.9812322386616,-4.14517727949942,
1.01591356788712));
#31751=CARTESIAN_POINT('Ctrl Pts',(-39.9425801423964,-4.18356833531871,
0.528588387345957));
#31752=CARTESIAN_POINT('Ctrl Pts',(-39.9175526247628,-4.34979992137534,
-1.55405138008967));
#31753=CARTESIAN_POINT('Ctrl Pts',(-40.2059756280345,-4.51601802195226,
-3.10057294641937));
#31754=CARTESIAN_POINT('Ctrl Pts',(-41.3475424919847,-4.93510316560563,
-5.9822748433334));
#31755=CARTESIAN_POINT('Ctrl Pts',(-42.200696259442,-5.18267423522269,-7.29352824387884));
#31756=CARTESIAN_POINT('Ctrl Pts',(-44.3399748842863,-5.74316333527725,
-9.49167634237876));
#31757=CARTESIAN_POINT('Ctrl Pts',(-45.6216384820464,-6.05234484883429,
-10.3690524867304));
#31758=CARTESIAN_POINT('Ctrl Pts',(-48.4365247491692,-6.71201694062915,
-11.5624766483838));
#31759=CARTESIAN_POINT('Ctrl Pts',(-49.9564645932,-7.05586981549073,-11.8682745705877));
#31760=CARTESIAN_POINT('Ctrl Pts',(-51.4707901907297,-7.39975358641511,
-11.8690397849987));
#31761=CARTESIAN_POINT('Ctrl Pts',(-42.339165491681,-3.67196736957056,1.35541211815623));
#31762=CARTESIAN_POINT('Ctrl Pts',(-42.3085779896418,-3.71078465277919,
0.885058966159984));
#31763=CARTESIAN_POINT('Ctrl Pts',(-42.2738114687052,-3.74842099134944,
0.426408535682965));
#31764=CARTESIAN_POINT('Ctrl Pts',(-42.2484605261705,-3.91292097416349,
-1.25364232212393));
#31765=CARTESIAN_POINT('Ctrl Pts',(-42.4817920098702,-4.07389626033816,
-2.51864171289909));
#31766=CARTESIAN_POINT('Ctrl Pts',(-43.396544242274,-4.45721661077528,-4.84795915805471));
#31767=CARTESIAN_POINT('Ctrl Pts',(-44.0882505573392,-4.68364919432705,
-5.91517020464438));
#31768=CARTESIAN_POINT('Ctrl Pts',(-45.8127425618219,-5.18357269340747,
-7.6945754034185));
#31769=CARTESIAN_POINT('Ctrl Pts',(-46.8532451029838,-5.46015465231553,
-8.40795287030642));
#31770=CARTESIAN_POINT('Ctrl Pts',(-49.1210183946318,-6.03800997039364,
-9.37372383748275));
#31771=CARTESIAN_POINT('Ctrl Pts',(-50.3610047224977,-6.3441696743126,-9.62254086010597));
#31772=CARTESIAN_POINT('Ctrl Pts',(-51.5794202324976,-6.64437068472187,
-9.62369151535368));
#31773=CARTESIAN_POINT('Ctrl Pts',(-44.5379552064474,-2.790088343341,1.24768171633315));
#31774=CARTESIAN_POINT('Ctrl Pts',(-44.5065971288718,-2.82988353081354,
0.765479194268018));
#31775=CARTESIAN_POINT('Ctrl Pts',(-44.4753533549367,-2.86682808256602,
0.332966345714832));
#31776=CARTESIAN_POINT('Ctrl Pts',(-44.4493473654519,-3.02969285879393,
-0.978922014688285));
#31777=CARTESIAN_POINT('Ctrl Pts',(-44.6328485090435,-3.18595276917332,
-1.98636136655288));
#31778=CARTESIAN_POINT('Ctrl Pts',(-45.3395640714125,-3.53647788533013,
-3.81078790532369));
#31779=CARTESIAN_POINT('Ctrl Pts',(-45.8840038433993,-3.7436335193008,-4.65460264911415));
#31780=CARTESIAN_POINT('Ctrl Pts',(-47.229037370506,-4.18815021742915,-6.0512151249181));
#31781=CARTESIAN_POINT('Ctrl Pts',(-48.0492213058428,-4.4349519522404,-6.61423873293507));
#31782=CARTESIAN_POINT('Ctrl Pts',(-49.8164110494045,-4.93795009675474,
-7.3724473949287));
#31783=CARTESIAN_POINT('Ctrl Pts',(-50.8005446234514,-5.20966094395016,
-7.56862230188086));
#31784=CARTESIAN_POINT('Ctrl Pts',(-51.7483027430072,-5.46990934942787,
-7.57037421505979));
#31785=CARTESIAN_POINT('Ctrl Pts',(-37.8397258902528,-1.06226042836983,
1.59647049649061));
#31786=CARTESIAN_POINT('Ctrl Pts',(-37.8163671782138,-1.10262802813137,
1.15259151033015));
#31787=CARTESIAN_POINT('Ctrl Pts',(-37.7797757625724,-1.14747953738618,
0.635572917992124));
#31788=CARTESIAN_POINT('Ctrl Pts',(-37.7806592587368,-1.3173273690917,-1.86858636175756));
#31789=CARTESIAN_POINT('Ctrl Pts',(-38.1455252315402,-1.43803115336822,
-3.71029995869359));
#31790=CARTESIAN_POINT('Ctrl Pts',(-39.5779229780038,-1.6936571382057,-7.16936247494164));
#31791=CARTESIAN_POINT('Ctrl Pts',(-40.6266263701707,-1.81514228728191,
-8.73699595770662));
#31792=CARTESIAN_POINT('Ctrl Pts',(-43.2633442117449,-2.06643737217002,
-11.3730256982132));
#31793=CARTESIAN_POINT('Ctrl Pts',(-44.8298904725261,-2.18792249430067,
-12.423580519232));
#31794=CARTESIAN_POINT('Ctrl Pts',(-48.290206627889,-2.44354852691099,-13.8529470821504));
#31795=CARTESIAN_POINT('Ctrl Pts',(-50.1387215498246,-2.56492073909757,
-14.2204718556739));
#31796=CARTESIAN_POINT('Ctrl Pts',(-51.9999633056261,-2.69099156569442,
-14.2198708430667));
#31797=CARTESIAN_POINT('Ctrl Pts',(-37.2107726459064,-0.347755560296676,
1.62964593809825));
#31798=CARTESIAN_POINT('Ctrl Pts',(-37.187608809593,-0.387786383581497,
1.18947011987297));
#31799=CARTESIAN_POINT('Ctrl Pts',(-37.149910451344,-0.433007907801872,
0.664243870391023));
#31800=CARTESIAN_POINT('Ctrl Pts',(-37.1502632733282,-0.60332371572967,
-1.95287905125797));
#31801=CARTESIAN_POINT('Ctrl Pts',(-37.5316956084247,-0.723283698714533,
-3.87337387077939));
#31802=CARTESIAN_POINT('Ctrl Pts',(-39.0273309715372,-0.979785618813286,
-7.48792130214639));
#31803=CARTESIAN_POINT('Ctrl Pts',(-40.122438463387,-1.10069469071833,-9.12360836231754));
#31804=CARTESIAN_POINT('Ctrl Pts',(-42.8765051571204,-1.35224759481462,
-11.8774049927137));
#31805=CARTESIAN_POINT('Ctrl Pts',(-44.5117551326353,-1.4731566546783,-12.9732563608865));
#31806=CARTESIAN_POINT('Ctrl Pts',(-48.1268013090037,-1.72965859379875,
-14.4676858045483));
#31807=CARTESIAN_POINT('Ctrl Pts',(-50.0548871962075,-1.85032539217923,
-14.8501851005246));
#31808=CARTESIAN_POINT('Ctrl Pts',(-51.9999570907662,-1.97670704765964,
-14.8499483202528));
#31809=CARTESIAN_POINT('Ctrl Pts',(-37.2110085708708,0.604714876209623,
1.62975512103804));
#31810=CARTESIAN_POINT('Ctrl Pts',(-37.1878478844851,0.564689496473117,
1.18963915964644));
#31811=CARTESIAN_POINT('Ctrl Pts',(-37.1500900231858,0.5194625641754,0.664246312460969));
#31812=CARTESIAN_POINT('Ctrl Pts',(-37.1497353315531,0.349146756271212,
-1.95288623095124));
#31813=CARTESIAN_POINT('Ctrl Pts',(-37.5322524147683,0.229186815971294,
-3.87317034518232));
#31814=CARTESIAN_POINT('Ctrl Pts',(-39.0266771563376,-0.0273151950943185,
-7.48823335804761));
#31815=CARTESIAN_POINT('Ctrl Pts',(-40.1225272605685,-0.14822420964857,
-9.12349227713884));
#31816=CARTESIAN_POINT('Ctrl Pts',(-42.8763256602482,-0.399777134882658,
-11.8775764776305));
#31817=CARTESIAN_POINT('Ctrl Pts',(-44.5120149889433,-0.520686157638547,
-12.9726927515284));
#31818=CARTESIAN_POINT('Ctrl Pts',(-48.1265710168888,-0.777188149416765,
-14.4683433355077));
#31819=CARTESIAN_POINT('Ctrl Pts',(-50.0549848089133,-0.897861662839052,
-14.8498038985338));
#31820=CARTESIAN_POINT('Ctrl Pts',(-51.9999570902567,-1.02423658127892,
-14.8500516281495));
#31821=CARTESIAN_POINT('Ctrl Pts',(-37.8403157026637,1.31891566289592,1.59674345384007));
#31822=CARTESIAN_POINT('Ctrl Pts',(-37.8169648654319,1.27856167200519,1.15301410976464));
#31823=CARTESIAN_POINT('Ctrl Pts',(-37.7802246921753,1.23369664255699,0.635579023166993));
#31824=CARTESIAN_POINT('Ctrl Pts',(-37.7793394043038,1.06384881091044,-1.86860431099072));
#31825=CARTESIAN_POINT('Ctrl Pts',(-38.1469172474041,0.943145133346677,
-3.70979114470212));
#31826=CARTESIAN_POINT('Ctrl Pts',(-39.5762884400003,0.687518921091354,
-7.17014261469349));
#31827=CARTESIAN_POINT('Ctrl Pts',(-40.6268483631268,0.566033915392139,
-8.73670574474909));
#31828=CARTESIAN_POINT('Ctrl Pts',(-43.2628954695621,0.314738777660199,
-11.373454410516));
#31829=CARTESIAN_POINT('Ctrl Pts',(-44.8305401132913,0.193253748298748,
-12.4221714958415));
#31830=CARTESIAN_POINT('Ctrl Pts',(-48.2896308976067,-0.0623724159560662,
-13.8545909095441));
#31831=CARTESIAN_POINT('Ctrl Pts',(-50.138965660225,-0.183762141924027,
-14.2195188100055));
#31832=CARTESIAN_POINT('Ctrl Pts',(-51.9999633043523,-0.309815399742648,
-14.2201291128083));
#31833=CARTESIAN_POINT('Ctrl Pts',(-37.7800000000001,-1.19058808997893,
0.));
#31834=CARTESIAN_POINT('Ctrl Pts',(-37.7806592587368,-1.3173273690917,-1.86858636175756));
#31835=CARTESIAN_POINT('Ctrl Pts',(-38.1455252315402,-1.43803115336822,
-3.71029995869359));
#31836=CARTESIAN_POINT('Ctrl Pts',(-39.5779229780038,-1.6936571382057,-7.16936247494164));
#31837=CARTESIAN_POINT('Ctrl Pts',(-40.6266263701707,-1.81514228728206,
-8.73699595770662));
#31838=CARTESIAN_POINT('Ctrl Pts',(-42.0790951378327,-1.95357130555297,
-10.1890856763502));
#31839=CARTESIAN_POINT('Ctrl Pts',(-42.215773213043,-1.96630970889372,-10.3203928635173));
#31840=CARTESIAN_POINT('Ctrl Pts',(-42.3549304887756,-1.97901608230199,
-10.4488603766005));
#31841=CARTESIAN_POINT('Ctrl Pts',(-37.7800000000001,1.19058808997921,9.99200722162641E-16));
#31842=CARTESIAN_POINT('Ctrl Pts',(-37.7793394043038,1.06384881091044,-1.86860431099072));
#31843=CARTESIAN_POINT('Ctrl Pts',(-38.1469172474041,0.943145133346677,
-3.70979114470212));
#31844=CARTESIAN_POINT('Ctrl Pts',(-39.5762884400003,0.687518921091354,
-7.17014261469349));
#31845=CARTESIAN_POINT('Ctrl Pts',(-40.6268483631268,0.566033915392139,
-8.73670574474909));
#31846=CARTESIAN_POINT('Ctrl Pts',(-42.0863595386742,0.426898290317344,
-10.1966053555722));
#31847=CARTESIAN_POINT('Ctrl Pts',(-42.2307237103631,0.413458201811568,
-10.3350231942284));
#31848=CARTESIAN_POINT('Ctrl Pts',(-42.3778559173172,0.400053103664163,
-10.4702558451011));
#31849=CARTESIAN_POINT('Ctrl Pts',(-44.4799848904464,-3.32327712822001,
1.24689064510956));
#31850=CARTESIAN_POINT('Ctrl Pts',(-44.4545866216563,-3.36716940899891,
0.764254540719541));
#31851=CARTESIAN_POINT('Ctrl Pts',(-44.4293496851003,-3.40814518985126,
0.332948627189092));
#31852=CARTESIAN_POINT('Ctrl Pts',(-44.4319119278341,-3.5730532724153,-0.978870002669229));
#31853=CARTESIAN_POINT('Ctrl Pts',(-44.6279251367563,-3.70160805587855,
-1.98783577088437));
#31854=CARTESIAN_POINT('Ctrl Pts',(-45.38610240764,-3.94798856177068,-3.80852727284065));
#31855=CARTESIAN_POINT('Ctrl Pts',(-45.949102167262,-4.07555420744993,-4.65544360722782));
#31856=CARTESIAN_POINT('Ctrl Pts',(-47.3456501222141,-4.32412798455906,
-6.04997283342565));
#31857=CARTESIAN_POINT('Ctrl Pts',(-48.18942650203,-4.4516935582084,-6.61832169901018));
#31858=CARTESIAN_POINT('Ctrl Pts',(-50.0137636932357,-4.69807420295161,
-7.36768403080659));
#31859=CARTESIAN_POINT('Ctrl Pts',(-51.0241709100446,-4.82686758917973,
-7.57138648682792));
#31860=CARTESIAN_POINT('Ctrl Pts',(-52.0000289040989,-4.94968218283394,
-7.56962581969448));
#31861=CARTESIAN_POINT('Ctrl Pts',(-42.4296678529921,-2.13646282181002,
1.35489302548969));
#31862=CARTESIAN_POINT('Ctrl Pts',(-42.4049009926057,-2.17926392766553,
0.884255395659172));
#31863=CARTESIAN_POINT('Ctrl Pts',(-42.3761273929606,-2.22143926476923,
0.426396892758864));
#31864=CARTESIAN_POINT('Ctrl Pts',(-42.3778082879602,-2.38787268687571,
-1.25360819498431));
#31865=CARTESIAN_POINT('Ctrl Pts',(-42.6265178497854,-2.51400314727506,
-2.51960912779415));
#31866=CARTESIAN_POINT('Ctrl Pts',(-43.592265824811,-2.76323860082922,-4.84647586782669));
#31867=CARTESIAN_POINT('Ctrl Pts',(-44.3056264360906,-2.88892662741274,
-5.91572199046927));
#31868=CARTESIAN_POINT('Ctrl Pts',(-46.0849874081721,-3.138340724919,-7.69376028691788));
#31869=CARTESIAN_POINT('Ctrl Pts',(-47.1521724801633,-3.26402870377879,
-8.41063186555663));
#31870=CARTESIAN_POINT('Ctrl Pts',(-49.481430310228,-3.51326424840763,-9.37059840620967));
#31871=CARTESIAN_POINT('Ctrl Pts',(-50.750806496017,-3.63979023544967,-9.62435378626137));
#31872=CARTESIAN_POINT('Ctrl Pts',(-52.0000086477592,-3.76358612954908,
-9.62320046360553));
#31873=CARTESIAN_POINT('Ctrl Pts',(-40.1875259567355,-1.37301063256228,
1.47293173916724));
#31874=CARTESIAN_POINT('Ctrl Pts',(-40.1634477706347,-1.4146215988494,1.01538079143144));
#31875=CARTESIAN_POINT('Ctrl Pts',(-40.1308402311895,-1.45810560976085,
0.528580648123612));
#31876=CARTESIAN_POINT('Ctrl Pts',(-40.1319542826431,-1.62620698164256,
-1.55402875454962));
#31877=CARTESIAN_POINT('Ctrl Pts',(-40.4376784663554,-1.74968648306518,
-3.10121432123338));
#31878=CARTESIAN_POINT('Ctrl Pts',(-41.6310829191806,-2.00204375396032,
-5.98129145451077));
#31879=CARTESIAN_POINT('Ctrl Pts',(-42.5084456369507,-2.12567864734773,
-7.29389406576292));
#31880=CARTESIAN_POINT('Ctrl Pts',(-44.706560886716,-2.37601161837734,-9.49113593804378));
#31881=CARTESIAN_POINT('Ctrl Pts',(-46.0177955705402,-2.49964647926416,
-10.3708286017169));
#31882=CARTESIAN_POINT('Ctrl Pts',(-48.8994560970704,-2.75200381048057,
-11.5604045561253));
#31883=CARTESIAN_POINT('Ctrl Pts',(-50.4518266808772,-2.87602039417437,
-11.8694761541285));
#31884=CARTESIAN_POINT('Ctrl Pts',(-51.9999864978575,-3.00091936260182,
-11.8687142284813));
#31885=CARTESIAN_POINT('Ctrl Pts',(-37.8397258902528,-1.06226042836983,
1.59647049649061));
#31886=CARTESIAN_POINT('Ctrl Pts',(-37.8163671782138,-1.10262802813137,
1.15259151033015));
#31887=CARTESIAN_POINT('Ctrl Pts',(-37.7797757625724,-1.14747953738618,
0.635572917992124));
#31888=CARTESIAN_POINT('Ctrl Pts',(-37.7806592587368,-1.3173273690917,-1.86858636175756));
#31889=CARTESIAN_POINT('Ctrl Pts',(-38.1455252315402,-1.43803115336822,
-3.71029995869359));
#31890=CARTESIAN_POINT('Ctrl Pts',(-39.5779229780038,-1.6936571382057,-7.16936247494164));
#31891=CARTESIAN_POINT('Ctrl Pts',(-40.6266263701707,-1.81514228728206,
-8.73699595770662));
#31892=CARTESIAN_POINT('Ctrl Pts',(-43.2633442117449,-2.06643737216986,
-11.3730256982132));
#31893=CARTESIAN_POINT('Ctrl Pts',(-44.829890472526,-2.18792249430096,-12.423580519232));
#31894=CARTESIAN_POINT('Ctrl Pts',(-48.290206627889,-2.44354852691069,-13.8529470821504));
#31895=CARTESIAN_POINT('Ctrl Pts',(-50.1387215498246,-2.56492073909667,
-14.2204718556739));
#31896=CARTESIAN_POINT('Ctrl Pts',(-51.9999633056261,-2.69099156569442,
-14.2198708430667));
#31897=CARTESIAN_POINT('Ctrl Pts',(-37.8403157026637,1.31891566289592,1.59674345384007));
#31898=CARTESIAN_POINT('Ctrl Pts',(-37.8169648654319,1.2785616720052,1.15301410976464));
#31899=CARTESIAN_POINT('Ctrl Pts',(-37.7802246921753,1.23369664255699,0.635579023166993));
#31900=CARTESIAN_POINT('Ctrl Pts',(-37.7793394043038,1.06384881091045,-1.86860431099072));
#31901=CARTESIAN_POINT('Ctrl Pts',(-38.1469172474041,0.943145133346679,
-3.70979114470212));
#31902=CARTESIAN_POINT('Ctrl Pts',(-39.5762884400003,0.687518921091357,
-7.17014261469349));
#31903=CARTESIAN_POINT('Ctrl Pts',(-40.6268483631268,0.566033915392151,
-8.73670574474909));
#31904=CARTESIAN_POINT('Ctrl Pts',(-43.2628954695621,0.314738777660206,
-11.373454410516));
#31905=CARTESIAN_POINT('Ctrl Pts',(-44.8305401132913,0.193253748298752,
-12.4221714958415));
#31906=CARTESIAN_POINT('Ctrl Pts',(-48.2896308976067,-0.0623724159560593,
-13.8545909095441));
#31907=CARTESIAN_POINT('Ctrl Pts',(-50.138965660225,-0.183762141924011,
-14.2195188100055));
#31908=CARTESIAN_POINT('Ctrl Pts',(-51.9999633043523,-0.309815399742647,
-14.2201291128083));
#31909=CARTESIAN_POINT('Ctrl Pts',(-40.1882694324258,1.62853105321851,1.47327580984132));
#31910=CARTESIAN_POINT('Ctrl Pts',(-40.1642011727661,1.58693724130854,1.01591349030302));
#31911=CARTESIAN_POINT('Ctrl Pts',(-40.131406120005,1.54343618780035,0.528588343874024));
#31912=CARTESIAN_POINT('Ctrl Pts',(-40.1302905677598,1.37533481599316,-1.55405138007982));
#31913=CARTESIAN_POINT('Ctrl Pts',(-40.4394331428155,1.25185544908462,-3.10057294640439));
#31914=CARTESIAN_POINT('Ctrl Pts',(-41.6290225365131,0.999497891523314,
-5.98227484334839));
#31915=CARTESIAN_POINT('Ctrl Pts',(-42.5087254655197,0.875863178866758,
-7.29352824389351));
#31916=CARTESIAN_POINT('Ctrl Pts',(-44.7059952341549,0.625530141225346,
-9.49167634236414));
#31917=CARTESIAN_POINT('Ctrl Pts',(-46.018614461608,0.501895397276723,-10.369052486768));
#31918=CARTESIAN_POINT('Ctrl Pts',(-48.898730372315,0.249537900119352,-11.5624766483463));
#31919=CARTESIAN_POINT('Ctrl Pts',(-50.4521347865908,0.125494944839277,
-11.8682745705877));
#31920=CARTESIAN_POINT('Ctrl Pts',(-51.9999864962518,0.000622417322863719,
-11.8690397849987));
#31921=CARTESIAN_POINT('Ctrl Pts',(-42.4307892712954,2.39089944281244,1.35541200298501));
#31922=CARTESIAN_POINT('Ctrl Pts',(-42.4060373834038,2.34812421168677,0.885058889671389));
#31923=CARTESIAN_POINT('Ctrl Pts',(-42.3769809488765,2.30592316845675,0.426408500610301));
#31924=CARTESIAN_POINT('Ctrl Pts',(-42.3752988309043,2.13948974646265,-1.25364232210375));
#31925=CARTESIAN_POINT('Ctrl Pts',(-42.6291645083404,2.01335948895693,-2.51864171287944));
#31926=CARTESIAN_POINT('Ctrl Pts',(-43.5891580556361,1.76412360301131,-4.8479591580744));
#31927=CARTESIAN_POINT('Ctrl Pts',(-44.3060485143004,1.63843584903247,-5.91517020465661));
#31928=CARTESIAN_POINT('Ctrl Pts',(-46.084134208595,1.38902165105224,-7.69457540340634));
#31929=CARTESIAN_POINT('Ctrl Pts',(-47.1534076509246,1.26333384857631,-8.40795287034413));
#31930=CARTESIAN_POINT('Ctrl Pts',(-49.4803356664663,1.01409805365021,-9.37372383744511));
#31931=CARTESIAN_POINT('Ctrl Pts',(-50.7512717901674,0.8875230677712,-9.62254086005841));
#31932=CARTESIAN_POINT('Ctrl Pts',(-52.0000086453373,0.76377627707492,-9.62369151535371));
#31933=CARTESIAN_POINT('Ctrl Pts',(-44.4816940061639,3.57672261477362,1.24768160116191));
#31934=CARTESIAN_POINT('Ctrl Pts',(-44.4563185564429,3.53286976879546,0.765479118775378));
#31935=CARTESIAN_POINT('Ctrl Pts',(-44.4306505608096,3.49185481010524,0.332966318322973));
#31936=CARTESIAN_POINT('Ctrl Pts',(-44.4280873491905,3.32694672771256,-0.978922014658035));
#31937=CARTESIAN_POINT('Ctrl Pts',(-44.631958819594,3.19839225347229,-1.98636136652375));
#31938=CARTESIAN_POINT('Ctrl Pts',(-45.381365961698,2.95201108858753,-3.81078790535288));
#31939=CARTESIAN_POINT('Ctrl Pts',(-45.9497454423884,2.82444585837497,-4.65460264912874));
#31940=CARTESIAN_POINT('Ctrl Pts',(-47.3443497895892,2.57587192813805,-6.05121512490362));
#31941=CARTESIAN_POINT('Ctrl Pts',(-48.1913089840218,2.44830662330916,-6.61423873299694));
#31942=CARTESIAN_POINT('Ctrl Pts',(-50.0120953836924,2.20192559709565,-7.37244739486697));
#31943=CARTESIAN_POINT('Ctrl Pts',(-51.0248803821906,2.07303718494182,-7.56862230179044));
#31944=CARTESIAN_POINT('Ctrl Pts',(-52.0000289004077,1.95031777657942,-7.57037421505984));
#31945=CARTESIAN_POINT('Ctrl Pts',(-37.6057474666452,4.33370633274489,1.59647061166167));
#31946=CARTESIAN_POINT('Ctrl Pts',(-37.6014604087211,4.32302794314895,1.48695576756414));
#31947=CARTESIAN_POINT('Ctrl Pts',(-37.5971743516736,4.31235100760161,1.37746396775989));
#31948=CARTESIAN_POINT('Ctrl Pts',(-37.5789019782659,4.26684181644195,0.910698635112159));
#31949=CARTESIAN_POINT('Ctrl Pts',(-37.5600270135807,4.23081870485879,0.486448413019324));
#31950=CARTESIAN_POINT('Ctrl Pts',(-37.5835818541665,4.07282953635717,-1.8685863617356));
#31951=CARTESIAN_POINT('Ctrl Pts',(-37.9619119570033,4.00528018449519,-3.71029995871943));
#31952=CARTESIAN_POINT('Ctrl Pts',(-39.4161093304632,3.95610755720103,-7.1693624749157));
#31953=CARTESIAN_POINT('Ctrl Pts',(-40.4714275735225,3.98510500543641,-8.73699595769429));
#31954=CARTESIAN_POINT('Ctrl Pts',(-43.1170704486978,4.1116118153854,-11.3730256982255));
#31955=CARTESIAN_POINT('Ctrl Pts',(-44.6849606628027,4.21430601437161,-12.4235805192234));
#31956=CARTESIAN_POINT('Ctrl Pts',(-48.1464351665736,4.45373622022133,-13.852947082159));
#31957=CARTESIAN_POINT('Ctrl Pts',(-49.993407938683,4.59667050421463,-14.2204718556549));
#31958=CARTESIAN_POINT('Ctrl Pts',(-51.8536466863969,4.73676521641199,-14.2198708430668));
#31959=CARTESIAN_POINT('Ctrl Pts',(-36.8815114147052,4.95142919224145,1.6296460532693));
#31960=CARTESIAN_POINT('Ctrl Pts',(-36.8772243107663,4.94075068802638,1.52013003366919));
#31961=CARTESIAN_POINT('Ctrl Pts',(-36.8729383891555,4.93007388724636,1.41064098632203));
#31962=CARTESIAN_POINT('Ctrl Pts',(-36.8546656346297,4.88456461021452,0.943868932650714));
#31963=CARTESIAN_POINT('Ctrl Pts',(-36.8348655943225,4.84834678143282,0.508392298446954));
#31964=CARTESIAN_POINT('Ctrl Pts',(-36.8579890764718,4.68985095932364,-1.95287905122974));
#31965=CARTESIAN_POINT('Ctrl Pts',(-37.2526110659712,4.62539547710255,-3.87337387080524));
#31966=CARTESIAN_POINT('Ctrl Pts',(-38.7695270468993,4.58435548148662,-7.48792130212039));
#31967=CARTESIAN_POINT('Ctrl Pts',(-39.8706950784938,4.62052713520107,-9.12360836230517));
#31968=CARTESIAN_POINT('Ctrl Pts',(-42.6325290552102,4.76347923308833,-11.877404992726));
#31969=CARTESIAN_POINT('Ctrl Pts',(-44.2683416970911,4.87652118890886,-12.973256360878));
#31970=CARTESIAN_POINT('Ctrl Pts',(-47.8830959478462,5.13710478162807,-14.4676858045569));
#31971=CARTESIAN_POINT('Ctrl Pts',(-49.8087293766818,5.29206142837056,-14.8501851005009));
#31972=CARTESIAN_POINT('Ctrl Pts',(-51.7519872491301,5.44377846349967,-14.8499483202528));
#31973=CARTESIAN_POINT('Ctrl Pts',(-36.7461942621622,5.89423842867625,1.62975523620908));
#31974=CARTESIAN_POINT('Ctrl Pts',(-36.7419071579067,5.88355992367606,1.52023920855918));
#31975=CARTESIAN_POINT('Ctrl Pts',(-36.7376212482649,5.87288312535246,1.41075017947915));
#31976=CARTESIAN_POINT('Ctrl Pts',(-36.719348444076,5.82737384119746,0.943978082261264));
#31977=CARTESIAN_POINT('Ctrl Pts',(-36.6994509531039,5.79114203694912,0.508394167533837));
#31978=CARTESIAN_POINT('Ctrl Pts',(-36.7219158272034,5.63255152132131,-1.95288623092271));
#31979=CARTESIAN_POINT('Ctrl Pts',(-37.1176115175746,5.56825045710434,-3.87317034520815));
#31980=CARTESIAN_POINT('Ctrl Pts',(-38.6333292122811,5.52703808203503,-7.48823335802159));
#31981=CARTESIAN_POINT('Ctrl Pts',(-39.7352322893736,5.5633154772789,-9.12349227711925));
#31982=CARTESIAN_POINT('Ctrl Pts',(-42.496800705893,5.70622937201901,-11.87757647765));
#31983=CARTESIAN_POINT('Ctrl Pts',(-44.1330482236871,5.81933389104568,-12.9726927515247));
#31984=CARTESIAN_POINT('Ctrl Pts',(-47.7473173225239,6.07984767625072,-14.4683433355114));
#31985=CARTESIAN_POINT('Ctrl Pts',(-49.6732762742263,6.23484434202318,-14.8498038985576));
#31986=CARTESIAN_POINT('Ctrl Pts',(-51.6164365682427,6.38655415380911,-14.8500516281495));
#31987=CARTESIAN_POINT('Ctrl Pts',(-37.2674545852877,6.69072942383186,1.59674356901112));
#31988=CARTESIAN_POINT('Ctrl Pts',(-37.263167526575,6.680051032273,1.48722870478903));
#31989=CARTESIAN_POINT('Ctrl Pts',(-37.2588814994477,6.66937410286672,1.37773695065262));
#31990=CARTESIAN_POINT('Ctrl Pts',(-37.2406090018804,6.6238648938997,0.910971509138724));
#31991=CARTESIAN_POINT('Ctrl Pts',(-37.2214904105359,6.58780684365017,0.48645308573652));
#31992=CARTESIAN_POINT('Ctrl Pts',(-37.2433987309883,6.42958094134897,-1.86860431096801));
#31993=CARTESIAN_POINT('Ctrl Pts',(-37.624413086019,6.36241763449877,-3.70979114472192));
#31994=CARTESIAN_POINT('Ctrl Pts',(-39.0756147439105,6.31281405857297,-7.1701426146735));
#31995=CARTESIAN_POINT('Ctrl Pts',(-40.1327706007244,6.3420758606307,-8.73670574473669));
#31996=CARTESIAN_POINT('Ctrl Pts',(-42.7777495754025,6.46848716271241,-11.3734544105282));
#31997=CARTESIAN_POINT('Ctrl Pts',(-44.3467269792927,6.57133776971453,-12.4221714958329));
#31998=CARTESIAN_POINT('Ctrl Pts',(-47.806988603268,6.81059345677706,-13.8545909095527));
#31999=CARTESIAN_POINT('Ctrl Pts',(-49.6547753637294,6.95362708074825,-14.2195188100197));
#32000=CARTESIAN_POINT('Ctrl Pts',(-51.5147699841784,7.09370444218559,-14.2201291128083));
#32001=CARTESIAN_POINT('Ctrl Pts',(-37.5648924257371,4.19818497005551,0.));
#32002=CARTESIAN_POINT('Ctrl Pts',(-37.5835818541665,4.07282953635717,-1.8685863617356));
#32003=CARTESIAN_POINT('Ctrl Pts',(-37.9619119570033,4.00528018449519,-3.71029995871943));
#32004=CARTESIAN_POINT('Ctrl Pts',(-39.4161093304632,3.95610755720103,-7.1693624749157));
#32005=CARTESIAN_POINT('Ctrl Pts',(-40.4714275735225,3.98510500543642,-8.73699595769429));
#32006=CARTESIAN_POINT('Ctrl Pts',(-41.92881280678,4.05479285274799,-10.1890856763504));
#32007=CARTESIAN_POINT('Ctrl Pts',(-42.0659125600695,4.06163542615554,-10.3203928635174));
#32008=CARTESIAN_POINT('Ctrl Pts',(-42.2054617208597,4.06886253049829,-10.4488603766002));
#32009=CARTESIAN_POINT('Ctrl Pts',(-37.2260157226955,6.55512420933882,-4.87766496047995E-9));
#32010=CARTESIAN_POINT('Ctrl Pts',(-37.243398731537,6.42958094105718,-1.86860431419405));
#32011=CARTESIAN_POINT('Ctrl Pts',(-37.6244130865614,6.36241763433584,-3.70979114625967));
#32012=CARTESIAN_POINT('Ctrl Pts',(-38.3500139148987,6.3376158464277,-5.43996687972819));
#32013=CARTESIAN_POINT('Ctrl Pts',(-39.0756147438695,6.31281405849791,-7.17014261470714));
#32014=CARTESIAN_POINT('Ctrl Pts',(-40.1327706007051,6.34207586058859,-8.7367057447602));
#32015=CARTESIAN_POINT('Ctrl Pts',(-41.4552600880589,6.40528151166132,-10.0550800776384));
#32016=CARTESIAN_POINT('Ctrl Pts',(-41.5972271209419,6.41206653251029,-10.1966053555764));
#32017=CARTESIAN_POINT('Ctrl Pts',(-41.7420345975428,6.41930840847686,-10.3350231942305));
#32018=CARTESIAN_POINT('Ctrl Pts',(-41.8895769551533,6.42697885114131,-10.4702558451008));
#32019=CARTESIAN_POINT('Ctrl Pts',(-44.5001944306519,3.04071090848703,1.24689076028072));
#32020=CARTESIAN_POINT('Ctrl Pts',(-44.4959078567086,3.03003372440579,1.13738827963299));
#32021=CARTESIAN_POINT('Ctrl Pts',(-44.4916204363957,3.01935537993451,1.02786752739767));
#32022=CARTESIAN_POINT('Ctrl Pts',(-44.4733518105235,2.9738470557106,0.561172897445051));
#32023=CARTESIAN_POINT('Ctrl Pts',(-44.463701217077,2.93980180526124,0.254828874448762));
#32024=CARTESIAN_POINT('Ctrl Pts',(-44.488157628525,2.78663561816024,-0.97887000271182));
#32025=CARTESIAN_POINT('Ctrl Pts',(-44.7004709588269,2.68728492514594,-1.98783577088727));
#32026=CARTESIAN_POINT('Ctrl Pts',(-45.485994680174,2.55131209327259,-3.80852727283799));
#32027=CARTESIAN_POINT('Ctrl Pts',(-46.0614183982389,2.50516810166005,-4.65544360721341));
#32028=CARTESIAN_POINT('Ctrl Pts',(-47.4791272455575,2.45787394352684,-6.04997283344033));
#32029=CARTESIAN_POINT('Ctrl Pts',(-48.3324696724478,2.45168870251976,-6.61832169900605));
#32030=CARTESIAN_POINT('Ctrl Pts',(-50.1733013631053,2.46744610981289,-7.36768403081099));
#32031=CARTESIAN_POINT('Ctrl Pts',(-51.1917533012898,2.48375959427692,-7.57138648673751));
#32032=CARTESIAN_POINT('Ctrl Pts',(-52.1751568070597,2.50107414862785,-7.56962581969461));
#32033=CARTESIAN_POINT('Ctrl Pts',(-42.3018453782487,3.92365461890858,1.35489314066083));
#32034=CARTESIAN_POINT('Ctrl Pts',(-42.2975586546965,3.91297706217519,1.24538683818762));
#32035=CARTESIAN_POINT('Ctrl Pts',(-42.2932716614844,3.90229915402396,1.13587503551223));
#32036=CARTESIAN_POINT('Ctrl Pts',(-42.275001852934,3.85679055844576,0.669158551014111));
#32037=CARTESIAN_POINT('Ctrl Pts',(-42.2624528820652,3.82212739678175,0.326351368872599));
#32038=CARTESIAN_POINT('Ctrl Pts',(-42.2862930185762,3.66742334692284,-1.25360819500681));
#32039=CARTESIAN_POINT('Ctrl Pts',(-42.5504213117424,3.57797177380988,-2.51960912780189));
#32040=CARTESIAN_POINT('Ctrl Pts',(-43.5418092681773,3.46871344469679,-4.84647586781908));
#32041=CARTESIAN_POINT('Ctrl Pts',(-44.2657961681649,3.44582654101586,-5.91572199045955));
#32042=CARTESIAN_POINT('Ctrl Pts',(-46.0625411381428,3.45218058836645,-7.69376028692778));
#32043=CARTESIAN_POINT('Ctrl Pts',(-47.1367510692374,3.47964820283165,-8.4106318655574));
#32044=CARTESIAN_POINT('Ctrl Pts',(-49.4777703293181,3.56443746806506,-9.37059840620908));
#32045=CARTESIAN_POINT('Ctrl Pts',(-50.7522326212179,3.61985039974676,-9.62435378620432));
#32046=CARTESIAN_POINT('Ctrl Pts',(-52.0063376889004,3.67509457152191,-9.62320046360563));
#32047=CARTESIAN_POINT('Ctrl Pts',(-39.9738746787523,4.36024590432563,1.47293185433834));
#32048=CARTESIAN_POINT('Ctrl Pts',(-39.969587791779,4.34956794053916,1.36342137723756));
#32049=CARTESIAN_POINT('Ctrl Pts',(-39.9653012588855,4.33889050812397,1.25391935060529));
#32050=CARTESIAN_POINT('Ctrl Pts',(-39.9470301849496,4.29338161981705,0.787178992719804));
#32051=CARTESIAN_POINT('Ctrl Pts',(-39.9313665239408,4.25805061593316,0.404559744691303));
#32052=CARTESIAN_POINT('Ctrl Pts',(-39.9549022371146,4.10171804395403,-1.55402875455033));
#32053=CARTESIAN_POINT('Ctrl Pts',(-40.2750875547445,4.02300447358394,-3.10121432124956));
#32054=CARTESIAN_POINT('Ctrl Pts',(-41.4922590551962,3.94305499752666,-5.98129145449459));
#32055=CARTESIAN_POINT('Ctrl Pts',(-42.3782865653892,3.94554026237538,-7.29389406575069));
#32056=CARTESIAN_POINT('Ctrl Pts',(-44.5896542676445,4.01057973632249,-9.49113593805607));
#32057=CARTESIAN_POINT('Ctrl Pts',(-45.9051375482497,4.0748114520141,-10.3708286017082));
#32058=CARTESIAN_POINT('Ctrl Pts',(-48.7933811184128,4.23512580635715,-11.5604045561341));
#32059=CARTESIAN_POINT('Ctrl Pts',(-50.3476002080614,4.33329690120631,-11.8694761541143));
#32060=CARTESIAN_POINT('Ctrl Pts',(-51.8977769668582,4.42999533819672,-11.8687142284813));
#32061=CARTESIAN_POINT('Ctrl Pts',(-37.6057474666452,4.33370633274489,1.59647061166167));
#32062=CARTESIAN_POINT('Ctrl Pts',(-37.6014604087211,4.32302794314895,1.48695576756414));
#32063=CARTESIAN_POINT('Ctrl Pts',(-37.5971743516736,4.31235100760161,1.37746396775989));
#32064=CARTESIAN_POINT('Ctrl Pts',(-37.5789019782659,4.26684181644196,0.910698635112159));
#32065=CARTESIAN_POINT('Ctrl Pts',(-37.5600270135807,4.23081870485879,0.486448413019324));
#32066=CARTESIAN_POINT('Ctrl Pts',(-37.5835818541665,4.07282953635717,-1.8685863617356));
#32067=CARTESIAN_POINT('Ctrl Pts',(-37.9619119570033,4.00528018449519,-3.71029995871943));
#32068=CARTESIAN_POINT('Ctrl Pts',(-39.4161093304632,3.95610755720103,-7.1693624749157));
#32069=CARTESIAN_POINT('Ctrl Pts',(-40.4714275735225,3.98510500543642,-8.73699595769429));
#32070=CARTESIAN_POINT('Ctrl Pts',(-43.1170704486978,4.1116118153854,-11.3730256982255));
#32071=CARTESIAN_POINT('Ctrl Pts',(-44.6849606628027,4.21430601437221,-12.4235805192234));
#32072=CARTESIAN_POINT('Ctrl Pts',(-48.1464351665736,4.45373622022074,-13.852947082159));
#32073=CARTESIAN_POINT('Ctrl Pts',(-49.9934079386831,4.59667050421464,-14.2204718556549));
#32074=CARTESIAN_POINT('Ctrl Pts',(-51.8536466863969,4.73676521641199,-14.2198708430668));
#32075=CARTESIAN_POINT('Ctrl Pts',(-37.2674545852877,6.69072942383186,1.59674356901112));
#32076=CARTESIAN_POINT('Ctrl Pts',(-37.263167526575,6.68005103227299,1.48722870478903));
#32077=CARTESIAN_POINT('Ctrl Pts',(-37.2588814994477,6.66937410286672,1.37773695065262));
#32078=CARTESIAN_POINT('Ctrl Pts',(-37.2406090018803,6.62386489389971,0.910971509138724));
#32079=CARTESIAN_POINT('Ctrl Pts',(-37.2214904105359,6.58780684365017,0.48645308573652));
#32080=CARTESIAN_POINT('Ctrl Pts',(-37.2433987309883,6.42958094134897,-1.86860431096802));
#32081=CARTESIAN_POINT('Ctrl Pts',(-37.6244130860238,6.36241763449877,-3.70979114472193));
#32082=CARTESIAN_POINT('Ctrl Pts',(-39.0756147439057,6.31281405857297,-7.1701426146735));
#32083=CARTESIAN_POINT('Ctrl Pts',(-40.1327706007196,6.3420758606307,-8.7367057447367));
#32084=CARTESIAN_POINT('Ctrl Pts',(-42.7777495754072,6.4684871627124,-11.3734544105282));
#32085=CARTESIAN_POINT('Ctrl Pts',(-44.3467269792975,6.57133776971454,-12.4221714958329));
#32086=CARTESIAN_POINT('Ctrl Pts',(-47.8069886032632,6.81059345677706,-13.8545909095527));
#32087=CARTESIAN_POINT('Ctrl Pts',(-49.6547753637331,6.95362708074793,-14.2195188100197));
#32088=CARTESIAN_POINT('Ctrl Pts',(-51.5147699841784,7.09370444218559,-14.2201291128083));
#32089=CARTESIAN_POINT('Ctrl Pts',(-39.5474466673498,7.33134203123354,1.47327592501242));
#32090=CARTESIAN_POINT('Ctrl Pts',(-39.5431597793819,7.3206640649734,1.36376542254399));
#32091=CARTESIAN_POINT('Ctrl Pts',(-39.5388732842043,7.30998664029854,1.25426345347746));
#32092=CARTESIAN_POINT('Ctrl Pts',(-39.5206020537614,7.26447772954494,0.787522958362851));
#32093=CARTESIAN_POINT('Ctrl Pts',(-39.5046312942642,7.22910268445617,0.404565634787169));
#32094=CARTESIAN_POINT('Ctrl Pts',(-39.5260915209543,7.07247170264163,-1.55405138007959));
#32095=CARTESIAN_POINT('Ctrl Pts',(-39.849660416496,6.99424475323091,-3.10057294641452));
#32096=CARTESIAN_POINT('Ctrl Pts',(-41.0630557303939,6.91375205389509,-5.98227484333816));
#32097=CARTESIAN_POINT('Ctrl Pts',(-41.9513996061357,6.91657054442171,-7.29352824388359));
#32098=CARTESIAN_POINT('Ctrl Pts',(-44.1619304425256,6.98148962792627,-9.49167634237396));
#32099=CARTESIAN_POINT('Ctrl Pts',(-45.4787841574542,7.04591850046845,-10.369052486764));
#32100=CARTESIAN_POINT('Ctrl Pts',(-48.3654988573771,7.20601286880697,-11.5624766483502));
#32101=CARTESIAN_POINT('Ctrl Pts',(-49.9207450076547,7.30430498991027,-11.8682745706258));
#32102=CARTESIAN_POINT('Ctrl Pts',(-51.4706130322883,7.40098575043911,-11.8690397849986));
#32103=CARTESIAN_POINT('Ctrl Pts',(-41.6586445536368,8.40509445805904,1.35541211815616));
#32104=CARTESIAN_POINT('Ctrl Pts',(-41.6543578285816,8.39441689759386,1.24590577741992));
#32105=CARTESIAN_POINT('Ctrl Pts',(-41.6500708922605,8.38373900111844,1.13639406157341));
#32106=CARTESIAN_POINT('Ctrl Pts',(-41.6318008476447,8.33823037168265,0.669677370086285));
#32107=CARTESIAN_POINT('Ctrl Pts',(-41.6187886661146,8.30350078066026,0.326360253172907));
#32108=CARTESIAN_POINT('Ctrl Pts',(-41.6394982516697,8.14834662563191,-1.25364232212485));
#32109=CARTESIAN_POINT('Ctrl Pts',(-41.9087301497829,8.05962904511491,-2.5186417128775));
#32110=CARTESIAN_POINT('Ctrl Pts',(-42.8944223117343,7.94955134754417,-4.84795915807629));
#32111=CARTESIAN_POINT('Ctrl Pts',(-43.6219030915765,7.927167063359,-5.91517020464915));
#32112=CARTESIAN_POINT('Ctrl Pts',(-45.4173857785771,7.9333395203096,-7.69457540341371));
#32113=CARTESIAN_POINT('Ctrl Pts',(-46.4936627982941,7.96110451544745,-8.40795287034476));
#32114=CARTESIAN_POINT('Ctrl Pts',(-48.832375993634,8.04556196575667,-9.37372383744437));
#32115=CARTESIAN_POINT('Ctrl Pts',(-50.1083893187814,8.10114839964074,-9.62254086011549));
#32116=CARTESIAN_POINT('Ctrl Pts',(-51.3620268377999,8.15637495641934,-9.62369151535365));
#32117=CARTESIAN_POINT('Ctrl Pts',(-43.5199138025264,9.87072183560205,1.24768171633308));
#32118=CARTESIAN_POINT('Ctrl Pts',(-43.5156272262978,9.86004464583405,1.1381791773697));
#32119=CARTESIAN_POINT('Ctrl Pts',(-43.5113398926855,9.84936631915668,1.02865855746757));
#32120=CARTESIAN_POINT('Ctrl Pts',(-43.4930709070328,9.80385794333174,0.561963612050125));
#32121=CARTESIAN_POINT('Ctrl Pts',(-43.4827143498822,9.76971145014305,0.254842414710469));
#32122=CARTESIAN_POINT('Ctrl Pts',(-43.5023995944666,9.6158592729741,-0.978922014698472));
#32123=CARTESIAN_POINT('Ctrl Pts',(-43.7224911564956,9.51762723325487,-1.98636136651214));
#32124=CARTESIAN_POINT('Ctrl Pts',(-44.4993341100792,9.3804056296222,-3.81078790536449));
#32125=CARTESIAN_POINT('Ctrl Pts',(-45.0800827322848,9.33502766338411,-4.65460264911893));
#32126=CARTESIAN_POINT('Ctrl Pts',(-46.4958677767967,9.28745674946867,-6.05121512491333));
#32127=CARTESIAN_POINT('Ctrl Pts',(-47.3523605835637,9.2817247362875,-6.61423873300218));
#32128=CARTESIAN_POINT('Ctrl Pts',(-49.1896776789234,9.29697643567186,-7.37244739486155));
#32129=CARTESIAN_POINT('Ctrl Pts',(-50.2104967199979,9.31353425505037,-7.56862230187132));
#32130=CARTESIAN_POINT('Ctrl Pts',(-51.1931844250964,9.33084205690745,-7.57037421505974));
#32131=CARTESIAN_POINT('Ctrl Pts',(-36.6062244663075,9.64145132693343,1.5964706812662));
#32132=CARTESIAN_POINT('Ctrl Pts',(-36.5951848118755,9.59613798296134,1.15259163661763));
#32133=CARTESIAN_POINT('Ctrl Pts',(-36.57271173128,9.54279427445571,0.635573001827313));
#32134=CARTESIAN_POINT('Ctrl Pts',(-36.6214111051725,9.38007537749595,-1.86858636170199));
#32135=CARTESIAN_POINT('Ctrl Pts',(-37.0055036281526,9.36705556804786,-3.71029995870504));
#32136=CARTESIAN_POINT('Ctrl Pts',(-38.451897363611,9.52533731124315,-7.1693624749302));
#32137=CARTESIAN_POINT('Ctrl Pts',(-39.4923472214662,9.70422705234564,-8.73699595770811));
#32138=CARTESIAN_POINT('Ctrl Pts',(-42.09305747065,10.2059604432804,-11.3730256982116));
#32139=CARTESIAN_POINT('Ctrl Pts',(-43.6303739147953,10.5307434056437,-12.423580519237));
#32140=CARTESIAN_POINT('Ctrl Pts',(-47.0225411280958,11.2603557414264,-13.8529470821453));
#32141=CARTESIAN_POINT('Ctrl Pts',(-48.8303727110256,11.6646867918221,-14.2204718556263));
#32142=CARTESIAN_POINT('Ctrl Pts',(-50.6517393542018,12.0680951184147,-14.2198708430666));
#32143=CARTESIAN_POINT('Ctrl Pts',(-35.8014489642672,10.1498171217997,1.62964612287382));
#32144=CARTESIAN_POINT('Ctrl Pts',(-35.7905014108219,10.1048818153751,1.18947024667539));
#32145=CARTESIAN_POINT('Ctrl Pts',(-35.7670704718544,10.0508712183131,0.664243958002629));
#32146=CARTESIAN_POINT('Ctrl Pts',(-35.8153925117153,9.88755379323324,-1.95287905118396));
#32147=CARTESIAN_POINT('Ctrl Pts',(-36.2151707898863,9.87991493951249,-3.87337387079329));
#32148=CARTESIAN_POINT('Ctrl Pts',(-37.7224873536581,10.0551723244044,-7.48792130213255));
#32149=CARTESIAN_POINT('Ctrl Pts',(-38.8072993194189,10.2476883531559,-9.12360836232142));
#32150=CARTESIAN_POINT('Ctrl Pts',(-41.5206776037716,10.7822353605362,-11.8774049927098));
#32151=CARTESIAN_POINT('Ctrl Pts',(-43.1237524839735,11.1269271238125,-12.9732563608916));
#32152=CARTESIAN_POINT('Ctrl Pts',(-46.6646288366134,11.89929151789,-14.4676858045432));
#32153=CARTESIAN_POINT('Ctrl Pts',(-48.548609463595,12.3267171393501,-14.8501851004771));
#32154=CARTESIAN_POINT('Ctrl Pts',(-50.4504961875093,12.7534443437023,-14.8499483202528));
#32155=CARTESIAN_POINT('Ctrl Pts',(-35.5333334012201,11.0637722809465,1.62975530581362));
#32156=CARTESIAN_POINT('Ctrl Pts',(-35.5223873364771,11.0188430850026,1.18963928646867));
#32157=CARTESIAN_POINT('Ctrl Pts',(-35.4989008284127,10.9648105349916,0.664246400071012));
#32158=CARTESIAN_POINT('Ctrl Pts',(-35.5465440138952,10.8012937803065,-1.95288623087167));
#32159=CARTESIAN_POINT('Ctrl Pts',(-35.9473630882428,10.7939605764042,-3.87317034519864));
#32160=CARTESIAN_POINT('Ctrl Pts',(-37.4535180947772,10.9688768025096,-7.48823335803139));
#32161=CARTESIAN_POINT('Ctrl Pts',(-38.5390425757456,11.1616021043726,-9.12349227713797));
#32162=CARTESIAN_POINT('Ctrl Pts',(-41.2521634397885,11.6960735043055,-11.8775764776314));
#32163=CARTESIAN_POINT('Ctrl Pts',(-42.8556598658218,12.040889083279,-12.9726927515335));
#32164=CARTESIAN_POINT('Ctrl Pts',(-46.3960659393421,12.813115336064,-14.4683433355027));
#32165=CARTESIAN_POINT('Ctrl Pts',(-48.2803630805299,13.2406268959519,-14.8498038985528));
#32166=CARTESIAN_POINT('Ctrl Pts',(-50.182154247211,13.6673330636264,-14.8500516281495));
#32167=CARTESIAN_POINT('Ctrl Pts',(-35.9359355586898,11.9263392248004,1.59674363861568));
#32168=CARTESIAN_POINT('Ctrl Pts',(-35.924899625982,11.8810411570281,1.15301423610205));
#32169=CARTESIAN_POINT('Ctrl Pts',(-35.9022876226749,11.8276425661526,0.635579106998265));
#32170=CARTESIAN_POINT('Ctrl Pts',(-35.9492898606247,11.6644253451772,-1.86860431092127));
#32171=CARTESIAN_POINT('Ctrl Pts',(-36.3359843740511,11.6521696602785,-3.70979114471603));
#32172=CARTESIAN_POINT('Ctrl Pts',(-37.7794742164016,11.809598506505,-7.17014261467971));
#32173=CARTESIAN_POINT('Ctrl Pts',(-38.8217053622759,11.9890114303897,-8.73670574475068));
#32174=CARTESIAN_POINT('Ctrl Pts',(-41.4217720606996,12.4905558027012,-11.3734544105145));
#32175=CARTESIAN_POINT('Ctrl Pts',(-42.9601423694208,12.8156483043099,-12.4221714958467));
#32176=CARTESIAN_POINT('Ctrl Pts',(-46.3511338849127,13.5449152868614,-13.8545909095391));
#32177=CARTESIAN_POINT('Ctrl Pts',(-48.1597570334068,13.9494605087261,-14.2195188100293));
#32178=CARTESIAN_POINT('Ctrl Pts',(-49.9808845034561,14.3528169182249,-14.2201291128084));
#32179=CARTESIAN_POINT('Ctrl Pts',(-36.5850719698905,9.50149509066535,0.));
#32180=CARTESIAN_POINT('Ctrl Pts',(-36.6214111051725,9.38007537749594,-1.86858636170199));
#32181=CARTESIAN_POINT('Ctrl Pts',(-37.0055036281526,9.36705556804786,-3.71029995870503));
#32182=CARTESIAN_POINT('Ctrl Pts',(-38.451897363611,9.52533731124314,-7.1693624749302));
#32183=CARTESIAN_POINT('Ctrl Pts',(-39.492347221471,9.70422705234564,-8.73699595770811));
#32184=CARTESIAN_POINT('Ctrl Pts',(-40.9249807596918,9.9806131216229,-10.1890856763501));
#32185=CARTESIAN_POINT('Ctrl Pts',(-41.0597112354463,10.006897376716,-10.3203928635172));
#32186=CARTESIAN_POINT('Ctrl Pts',(-41.1968114628076,10.0339108358061,-10.4488603766004));
#32187=CARTESIAN_POINT('Ctrl Pts',(-35.914217116421,11.7862169042734,-1.22124532708767E-15));
#32188=CARTESIAN_POINT('Ctrl Pts',(-35.9492898606247,11.6644253451772,-1.86860431092127));
#32189=CARTESIAN_POINT('Ctrl Pts',(-36.3359843740511,11.6521696602785,-3.70979114471603));
#32190=CARTESIAN_POINT('Ctrl Pts',(-37.7794742164016,11.809598506505,-7.17014261467971));
#32191=CARTESIAN_POINT('Ctrl Pts',(-38.8217053622759,11.9890114303897,-8.73670574475068));
#32192=CARTESIAN_POINT('Ctrl Pts',(-40.2612951155293,12.2667035909867,-10.196605355572));
#32193=CARTESIAN_POINT('Ctrl Pts',(-40.4035980344055,12.2944800077075,-10.3350231942279));
#32194=CARTESIAN_POINT('Ctrl Pts',(-40.5485470057464,12.3230698430838,-10.4702558451006));
#32195=CARTESIAN_POINT('Ctrl Pts',(-43.6145083358836,9.34279883641509,1.24689082988537));
#32196=CARTESIAN_POINT('Ctrl Pts',(-43.6025047583784,9.29352897570348,0.764254661685365));
#32197=CARTESIAN_POINT('Ctrl Pts',(-43.5898343018983,9.24710292813362,0.332948671153414));
#32198=CARTESIAN_POINT('Ctrl Pts',(-43.6387527331905,9.08959664356559,-0.978870002777604));
#32199=CARTESIAN_POINT('Ctrl Pts',(-43.8630440977203,9.02147253460984,-1.98783577088221));
#32200=CARTESIAN_POINT('Ctrl Pts',(-44.6599232717658,8.99867539144857,-3.80852727284259));
#32201=CARTESIAN_POINT('Ctrl Pts',(-45.2360569807998,9.03489241252397,-4.65544360722721));
#32202=CARTESIAN_POINT('Ctrl Pts',(-46.6460662566679,9.18984064605092,-6.04997283342596));
#32203=CARTESIAN_POINT('Ctrl Pts',(-47.4916031396373,9.30516165135672,-6.61832169900054));
#32204=CARTESIAN_POINT('Ctrl Pts',(-49.3114553051051,9.5827363353036,-7.36768403081585));
#32205=CARTESIAN_POINT('Ctrl Pts',(-50.3172192201065,9.74382459494245,-7.57138648668015));
#32206=CARTESIAN_POINT('Ctrl Pts',(-51.2881489781559,9.90091582292617,-7.56962581969428));
#32207=CARTESIAN_POINT('Ctrl Pts',(-41.3128793157233,9.90389776310336,1.35489321026544));
#32208=CARTESIAN_POINT('Ctrl Pts',(-41.3011741506654,9.85585276552896,0.884255518278619));
#32209=CARTESIAN_POINT('Ctrl Pts',(-41.2854482448446,9.80727935893038,0.426396949034063));
#32210=CARTESIAN_POINT('Ctrl Pts',(-41.3339507669686,9.64806121736179,-1.25360819503921));
#32211=CARTESIAN_POINT('Ctrl Pts',(-41.6081209011007,9.5971095076056,-2.51960912779453));
#32212=CARTESIAN_POINT('Ctrl Pts',(-42.6049670390268,9.63005248742562,-4.84647586782619));
#32213=CARTESIAN_POINT('Ctrl Pts',(-43.3248419422851,9.71043261801081,-5.9157219904686));
#32214=CARTESIAN_POINT('Ctrl Pts',(-45.1023943639257,9.97242546014147,-7.69376028691838));
#32215=CARTESIAN_POINT('Ctrl Pts',(-46.1617613376966,10.1524895065124,-8.4106318655567));
#32216=CARTESIAN_POINT('Ctrl Pts',(-48.466885626621,10.5695775166739,-9.37059840620937));
#32217=CARTESIAN_POINT('Ctrl Pts',(-49.7204896475891,10.8058013195906,-9.62435378613754));
#32218=CARTESIAN_POINT('Ctrl Pts',(-50.9539676685889,11.0389609452144,-9.62320046360541));
#32219=CARTESIAN_POINT('Ctrl Pts',(-38.9464705831155,10.0047404051439,1.47293192394291));
#32220=CARTESIAN_POINT('Ctrl Pts',(-38.9350908951662,9.95803136027088,1.01538091584758));
#32221=CARTESIAN_POINT('Ctrl Pts',(-38.9160550470335,9.90712214456995,0.528580717861568));
#32222=CARTESIAN_POINT('Ctrl Pts',(-38.9644836025053,9.74614391854898,-1.55402875454917));
#32223=CARTESIAN_POINT('Ctrl Pts',(-39.2926120042888,9.71379866052871,-3.10121432124109));
#32224=CARTESIAN_POINT('Ctrl Pts',(-40.5087724506345,9.80788452010445,-5.98129145450301));
#32225=CARTESIAN_POINT('Ctrl Pts',(-41.3854277882649,9.93643935035659,-7.29389406576453));
#32226=CARTESIAN_POINT('Ctrl Pts',(-43.5650308736069,10.3155272531459,-9.49113593804205));
#32227=CARTESIAN_POINT('Ctrl Pts',(-44.8579833049637,10.5663179729168,-10.3708286017171));
#32228=CARTESIAN_POINT('Ctrl Pts',(-47.6940136086746,11.1360404748698,-11.560404556125));
#32229=CARTESIAN_POINT('Ctrl Pts',(-49.2184417855036,11.4544007679043,-11.8694761540619));
#32230=CARTESIAN_POINT('Ctrl Pts',(-50.7390783576438,11.770728108961,-11.8687142284812));
#32231=CARTESIAN_POINT('Ctrl Pts',(-36.6062244663075,9.64145132693344,1.5964706812662));
#32232=CARTESIAN_POINT('Ctrl Pts',(-36.5951848118755,9.59613798296134,1.15259163661763));
#32233=CARTESIAN_POINT('Ctrl Pts',(-36.57271173128,9.54279427445571,0.635573001827313));
#32234=CARTESIAN_POINT('Ctrl Pts',(-36.6214111051725,9.38007537749594,-1.86858636170199));
#32235=CARTESIAN_POINT('Ctrl Pts',(-37.0055036281526,9.36705556804786,-3.71029995870503));
#32236=CARTESIAN_POINT('Ctrl Pts',(-38.451897363611,9.52533731124314,-7.1693624749302));
#32237=CARTESIAN_POINT('Ctrl Pts',(-39.492347221471,9.70422705234564,-8.73699595770811));
#32238=CARTESIAN_POINT('Ctrl Pts',(-42.0930574706453,10.2059604432804,-11.3730256982116));
#32239=CARTESIAN_POINT('Ctrl Pts',(-43.6303739147953,10.5307434056437,-12.423580519237));
#32240=CARTESIAN_POINT('Ctrl Pts',(-47.0225411280958,11.2603557414264,-13.8529470821453));
#32241=CARTESIAN_POINT('Ctrl Pts',(-48.8303727110256,11.6646867918221,-14.2204718556263));
#32242=CARTESIAN_POINT('Ctrl Pts',(-50.6517393542018,12.0680951184147,-14.2198708430666));
#32243=CARTESIAN_POINT('Ctrl Pts',(-35.9359355586898,11.9263392248004,1.59674363861568));
#32244=CARTESIAN_POINT('Ctrl Pts',(-35.924899625982,11.8810411570281,1.15301423610205));
#32245=CARTESIAN_POINT('Ctrl Pts',(-35.9022876226749,11.8276425661526,0.635579106998265));
#32246=CARTESIAN_POINT('Ctrl Pts',(-35.9492898606247,11.6644253451772,-1.86860431092127));
#32247=CARTESIAN_POINT('Ctrl Pts',(-36.3359843740511,11.6521696602785,-3.70979114471722));
#32248=CARTESIAN_POINT('Ctrl Pts',(-37.7794742164016,11.809598506505,-7.17014261467851));
#32249=CARTESIAN_POINT('Ctrl Pts',(-38.8217053622759,11.9890114303897,-8.73670574475307));
#32250=CARTESIAN_POINT('Ctrl Pts',(-41.4217720606996,12.4905558027012,-11.3734544105121));
#32251=CARTESIAN_POINT('Ctrl Pts',(-42.9601423694208,12.8156483043111,-12.4221714958467));
#32252=CARTESIAN_POINT('Ctrl Pts',(-46.3511338849127,13.5449152868602,-13.8545909095391));
#32253=CARTESIAN_POINT('Ctrl Pts',(-48.159757033407,13.9494605087261,-14.2195188100293));
#32254=CARTESIAN_POINT('Ctrl Pts',(-49.9808845034561,14.3528169182249,-14.2201291128084));
#32255=CARTESIAN_POINT('Ctrl Pts',(-38.1015519292156,12.8849080239688,1.47327599461702));
#32256=CARTESIAN_POINT('Ctrl Pts',(-38.0901769326121,12.8382182351928,1.0159136147825));
#32257=CARTESIAN_POINT('Ctrl Pts',(-38.0709659683617,12.787239838666,0.528588413607038));
#32258=CARTESIAN_POINT('Ctrl Pts',(-38.1172552346282,12.6256334607371,-1.55405138006188));
#32259=CARTESIAN_POINT('Ctrl Pts',(-38.4486635210218,12.5942514039233,-3.10057294641456));
#32260=CARTESIAN_POINT('Ctrl Pts',(-39.6611635256837,12.6872621620782,-5.9822748433383));
#32261=CARTESIAN_POINT('Ctrl Pts',(-40.5400642286511,12.8164764794374,-7.29352824389523));
#32262=CARTESIAN_POINT('Ctrl Pts',(-42.7188560995434,13.1953261187531,-9.49167634236253));
#32263=CARTESIAN_POINT('Ctrl Pts',(-44.0131369578426,13.4465070217416,-10.3690524867731));
#32264=CARTESIAN_POINT('Ctrl Pts',(-46.8476852602797,14.0157941959106,-11.5624766483414));
#32265=CARTESIAN_POINT('Ctrl Pts',(-48.3731128199116,14.3344204492882,-11.8682745706306));
#32266=CARTESIAN_POINT('Ctrl Pts',(-49.8934463159786,14.6506863563568,-11.8690397849988));
#32267=CARTESIAN_POINT('Ctrl Pts',(-40.0384499621469,14.2481859850621,1.35541218776081));
#32268=CARTESIAN_POINT('Ctrl Pts',(-40.0267518732657,14.2001700323356,0.885059012385724));
#32269=CARTESIAN_POINT('Ctrl Pts',(-40.0107618318058,14.1514922771421,0.42640855687806));
#32270=CARTESIAN_POINT('Ctrl Pts',(-40.0560375664346,13.9913266653952,-1.25364232213227));
#32271=CARTESIAN_POINT('Ctrl Pts',(-40.3351549001509,13.9418277959651,-2.51864171288711));
#32272=CARTESIAN_POINT('Ctrl Pts',(-41.3264798268871,13.9731491512543,-4.84795915806681));
#32273=CARTESIAN_POINT('Ctrl Pts',(-42.049741517119,14.0545240163351,-5.9151702046561));
#32274=CARTESIAN_POINT('Ctrl Pts',(-43.8260703470018,14.3161574747981,-7.69457540340699));
#32275=CARTESIAN_POINT('Ctrl Pts',(-44.8874410477371,14.4968100523227,-8.40795287035882));
#32276=CARTESIAN_POINT('Ctrl Pts',(-47.1903299665196,14.9132414377163,-9.37372383743066));
#32277=CARTESIAN_POINT('Ctrl Pts',(-48.4454445415192,15.1498577118804,-9.62254086012515));
#32278=CARTESIAN_POINT('Ctrl Pts',(-49.6784622796991,15.3829333626942,-9.62369151535384));
#32279=CARTESIAN_POINT('Ctrl Pts',(-41.6721936506077,15.9637816213006,1.24768178593779));
#32280=CARTESIAN_POINT('Ctrl Pts',(-41.6602008576572,15.9145560268582,0.765479239885611));
#32281=CARTESIAN_POINT('Ctrl Pts',(-41.6471278409878,15.8679709451247,0.332966362275953));
#32282=CARTESIAN_POINT('Ctrl Pts',(-41.6911284345662,15.7090206532942,-0.978922014726203));
#32283=CARTESIAN_POINT('Ctrl Pts',(-41.9229596586979,15.6431107691499,-1.98636136652895));
#32284=CARTESIAN_POINT('Ctrl Pts',(-42.7114241414665,15.6178421628833,-3.81078790534779));
#32285=CARTESIAN_POINT('Ctrl Pts',(-43.2927195379906,15.6555752251637,-4.65460264912839));
#32286=CARTESIAN_POINT('Ctrl Pts',(-44.7008639790628,15.8099757341941,-6.05121512490418));
#32287=CARTESIAN_POINT('Ctrl Pts',(-45.5494546745316,15.926193699927,-6.61423873300684));
#32288=CARTESIAN_POINT('Ctrl Pts',(-47.3658999879521,16.2027676442764,-7.3724473948574));
#32289=CARTESIAN_POINT('Ctrl Pts',(-48.3739721396694,16.3644346257032,-7.56862230190484));
#32290=CARTESIAN_POINT('Ctrl Pts',(-49.3441943438429,16.5214173008837,-7.57037421506003));
#32291=CARTESIAN_POINT('Ctrl Pts',(-34.8615042977019,14.752924178887,1.59647077610298));
#32292=CARTESIAN_POINT('Ctrl Pts',(-34.857025771947,14.7065009496435,1.1525917014061));
#32293=CARTESIAN_POINT('Ctrl Pts',(-34.8423730342687,14.6505019462284,0.635573044894269));
#32294=CARTESIAN_POINT('Ctrl Pts',(-34.9137340335311,14.4963699338419,-1.86858636178585));
#32295=CARTESIAN_POINT('Ctrl Pts',(-35.2957699604605,14.5381447126175,-3.71029995870276));
#32296=CARTESIAN_POINT('Ctrl Pts',(-36.7049156525828,14.9006586664088,-7.16936247493249));
#32297=CARTESIAN_POINT('Ctrl Pts',(-37.7093165664795,15.2257990211696,-8.7369959577155));
#32298=CARTESIAN_POINT('Ctrl Pts',(-40.2121512288796,16.0925451480898,-11.3730256982043));
#32299=CARTESIAN_POINT('Ctrl Pts',(-41.6875985735023,16.6328052292555,-12.4235805192037));
#32300=CARTESIAN_POINT('Ctrl Pts',(-44.9414037540494,17.8377468919989,-13.8529470821786));
#32301=CARTESIAN_POINT('Ctrl Pts',(-46.6732919100481,18.4952436947574,-14.2204718556881));
#32302=CARTESIAN_POINT('Ctrl Pts',(-48.4187086763094,19.1537534053194,-14.2198708430667));
#32303=CARTESIAN_POINT('Ctrl Pts',(-33.9925722540019,15.1415840475453,1.62964621771058));
#32304=CARTESIAN_POINT('Ctrl Pts',(-33.9881310914378,15.095548115337,1.18947031171891));
#32305=CARTESIAN_POINT('Ctrl Pts',(-33.9726251531373,15.0387526938571,0.664244003018932));
#32306=CARTESIAN_POINT('Ctrl Pts',(-34.043697838502,14.8839745452467,-1.95287905129093));
#32307=CARTESIAN_POINT('Ctrl Pts',(-34.4404940724067,14.9333078251056,-3.87337387078857));
#32308=CARTESIAN_POINT('Ctrl Pts',(-35.9075266006076,15.321294855491,-7.48792130213727));
#32309=CARTESIAN_POINT('Ctrl Pts',(-36.9538988571888,15.6662361881643,-9.1236083623312));
#32310=CARTESIAN_POINT('Ctrl Pts',(-39.5635848920882,16.5814962694126,-11.8774049927));
#32311=CARTESIAN_POINT('Ctrl Pts',(-41.1012880289292,17.1508209097894,-12.9732563608727));
#32312=CARTESIAN_POINT('Ctrl Pts',(-44.4962044519299,18.4192429936658,-14.4676858045621));
#32313=CARTESIAN_POINT('Ctrl Pts',(-46.3001798643524,19.1104364369558,-14.8501851005151));
#32314=CARTESIAN_POINT('Ctrl Pts',(-48.1219785107276,19.8034868749642,-14.8499483202528));
#32315=CARTESIAN_POINT('Ctrl Pts',(-33.597116340133,16.0080796379929,1.62975540065037));
#32316=CARTESIAN_POINT('Ctrl Pts',(-33.5926757814912,15.9620499659323,1.18963935151889));
#32317=CARTESIAN_POINT('Ctrl Pts',(-33.5771179639666,15.9052249066534,0.664246445091293));
#32318=CARTESIAN_POINT('Ctrl Pts',(-33.647547072249,15.7501528462652,-1.95288623098987));
#32319=CARTESIAN_POINT('Ctrl Pts',(-34.0453300100375,15.7999367856098,-3.87317034519032));
#32320=CARTESIAN_POINT('Ctrl Pts',(-35.5112613559224,16.1874208228852,-7.48823335803971));
#32321=CARTESIAN_POINT('Ctrl Pts',(-36.5583090926775,16.5326707000636,-9.12349227715013));
#32322=CARTESIAN_POINT('Ctrl Pts',(-39.1677510874848,17.447819308696,-11.8775764776193));
#32323=CARTESIAN_POINT('Ctrl Pts',(-40.7058538586162,18.0173264967329,-12.9726927515434));
#32324=CARTESIAN_POINT('Ctrl Pts',(-44.1003244488304,19.2855449177099,-14.4683433354928));
#32325=CARTESIAN_POINT('Ctrl Pts',(-45.9046009234708,19.9768684693681,-14.8498038985005));
#32326=CARTESIAN_POINT('Ctrl Pts',(-47.7263079790886,20.6698844856026,-14.8500516281495));
#32327=CARTESIAN_POINT('Ctrl Pts',(-33.8728645130296,16.919163155006,1.59674373345245));
#32328=CARTESIAN_POINT('Ctrl Pts',(-33.8683874970857,16.8727555761311,1.15301430090585));
#32329=CARTESIAN_POINT('Ctrl Pts',(-33.8536050613443,16.816682478221,0.635579150075179));
#32330=CARTESIAN_POINT('Ctrl Pts',(-33.9233571178916,16.6618156863834,-1.86860431103318));
#32331=CARTESIAN_POINT('Ctrl Pts',(-34.3078598045327,16.7047171138864,-3.70979114470774));
#32332=CARTESIAN_POINT('Ctrl Pts',(-35.7142525408745,17.0659735848861,-7.17014261468798));
#32333=CARTESIAN_POINT('Ctrl Pts',(-36.720342155194,17.3918853009154,-8.73670574476044));
#32334=CARTESIAN_POINT('Ctrl Pts',(-39.2225667173783,18.2583527463007,-11.3734544105047));
#32335=CARTESIAN_POINT('Ctrl Pts',(-40.6990131477318,18.7990691966204,-12.4221714958709));
#32336=CARTESIAN_POINT('Ctrl Pts',(-43.9517037462886,20.0035017021032,-13.8545909095149));
#32337=CARTESIAN_POINT('Ctrl Pts',(-45.6843449310622,20.6613231478773,-14.2195188099484));
#32338=CARTESIAN_POINT('Ctrl Pts',(-47.429532347212,21.3197474319156,-14.2201291128084));
#32339=CARTESIAN_POINT('Ctrl Pts',(-34.8604849513722,14.6113821712785,0.));
#32340=CARTESIAN_POINT('Ctrl Pts',(-34.9137340335311,14.4963699338419,-1.86858636178585));
#32341=CARTESIAN_POINT('Ctrl Pts',(-35.2957699604605,14.5381447126175,-3.71029995870396));
#32342=CARTESIAN_POINT('Ctrl Pts',(-36.7049156525828,14.9006586664088,-7.16936247493129));
#32343=CARTESIAN_POINT('Ctrl Pts',(-37.7093165664795,15.225799021172,-8.73699595771789));
#32344=CARTESIAN_POINT('Ctrl Pts',(-39.0880341222376,15.7032568890511,-10.1890856763494));
#32345=CARTESIAN_POINT('Ctrl Pts',(-39.2176525965035,15.748447754191,-10.3203928635156));
#32346=CARTESIAN_POINT('Ctrl Pts',(-39.3495129251727,15.7946976518991,-10.4488603765979));
#32347=CARTESIAN_POINT('Ctrl Pts',(-33.8713086176151,16.7773762111444,1.66533453693773E-16));
#32348=CARTESIAN_POINT('Ctrl Pts',(-33.9233571178916,16.6618156863834,-1.86860431103318));
#32349=CARTESIAN_POINT('Ctrl Pts',(-34.3078598045327,16.7047171138864,-3.70979114470774));
#32350=CARTESIAN_POINT('Ctrl Pts',(-35.7142525408745,17.0659735848861,-7.17014261468798));
#32351=CARTESIAN_POINT('Ctrl Pts',(-36.720342155194,17.3918853009154,-8.73670574476044));
#32352=CARTESIAN_POINT('Ctrl Pts',(-38.1057592455502,17.8716259385927,-10.196605355572));
#32353=CARTESIAN_POINT('Ctrl Pts',(-38.2426607296438,17.9193714483236,-10.3350231942284));
#32354=CARTESIAN_POINT('Ctrl Pts',(-38.382065571659,17.9682986698096,-10.4702558451019));
#32355=CARTESIAN_POINT('Ctrl Pts',(-41.8409566234847,15.4546943255723,1.24689092472229));
#32356=CARTESIAN_POINT('Ctrl Pts',(-41.8360870570322,15.4042176703914,0.764254723812363));
#32357=CARTESIAN_POINT('Ctrl Pts',(-41.8301526811182,15.356460975121,0.332948693666065));
#32358=CARTESIAN_POINT('Ctrl Pts',(-41.9009886759728,15.207519693579,-0.978870002679738));
#32359=CARTESIAN_POINT('Ctrl Pts',(-42.1326921493261,15.1720089790277,-1.98783577089606));
#32360=CARTESIAN_POINT('Ctrl Pts',(-42.9247046141597,15.2628516087108,-3.80852727282881));
#32361=CARTESIAN_POINT('Ctrl Pts',(-43.4898198932031,15.3806923683063,-4.65544360720821));
#32362=CARTESIAN_POINT('Ctrl Pts',(-44.8634258749837,15.7347286943737,-6.04997283344502));
#32363=CARTESIAN_POINT('Ctrl Pts',(-45.6839445213885,15.9692083429235,-6.61832169892883));
#32364=CARTESIAN_POINT('Ctrl Pts',(-47.4457702195768,16.5029496832554,-7.36768403088772));
#32365=CARTESIAN_POINT('Ctrl Pts',(-48.4183716585645,16.8055334254949,-7.57138648688498));
#32366=CARTESIAN_POINT('Ctrl Pts',(-49.3570623388652,17.0992034029529,-7.5696258196944));
#32367=CARTESIAN_POINT('Ctrl Pts',(-39.4829021650676,15.6825261124556,1.35489330510232));
#32368=CARTESIAN_POINT('Ctrl Pts',(-39.4781536574581,15.6333043216781,0.884255581230426));
#32369=CARTESIAN_POINT('Ctrl Pts',(-39.4695005333236,15.5829872885716,0.426396977895696));
#32370=CARTESIAN_POINT('Ctrl Pts',(-39.5401684750185,15.4322923841483,-1.25360819500321));
#32371=CARTESIAN_POINT('Ctrl Pts',(-39.8187991367997,15.4208777676018,-2.51960912780342));
#32372=CARTESIAN_POINT('Ctrl Pts',(-40.8008105435659,15.5953514322915,-4.84647586781735));
#32373=CARTESIAN_POINT('Ctrl Pts',(-41.5019188729544,15.7773622894618,-5.91572199046159));
#32374=CARTESIAN_POINT('Ctrl Pts',(-43.2240929050568,16.2896605076646,-7.69376028692545));
#32375=CARTESIAN_POINT('Ctrl Pts',(-44.2470512648569,16.6186554012354,-8.41063186550418));
#32376=CARTESIAN_POINT('Ctrl Pts',(-46.4693548995128,17.3595514471548,-9.37059840626199));
#32377=CARTESIAN_POINT('Ctrl Pts',(-47.6765808868229,17.7717772858477,-9.62435378628037));
#32378=CARTESIAN_POINT('Ctrl Pts',(-48.8643218056538,18.1781059077968,-9.62320046360549));
#32379=CARTESIAN_POINT('Ctrl Pts',(-37.1262286569851,15.4455672457339,1.47293201877974));
#32380=CARTESIAN_POINT('Ctrl Pts',(-37.1216121877099,15.3977141299005,1.01538097969802));
#32381=CARTESIAN_POINT('Ctrl Pts',(-37.1100152319898,15.3446140089039,0.528580753663548));
#32382=CARTESIAN_POINT('Ctrl Pts',(-37.1808604460415,15.1921664085235,-1.55402875457453));
#32383=CARTESIAN_POINT('Ctrl Pts',(-37.5102521839442,15.2068479190352,-3.10121432124141));
#32384=CARTESIAN_POINT('Ctrl Pts',(-38.7006440566484,15.4730537974485,-5.98129145450273));
#32385=CARTESIAN_POINT('Ctrl Pts',(-39.550081047065,15.7250611874948,-7.29389406576472));
#32386=CARTESIAN_POINT('Ctrl Pts',(-41.653549082182,16.4104803826143,-9.4911359380419));
#32387=CARTESIAN_POINT('Ctrl Pts',(-42.8976498813487,16.8427247306107,-10.3708286016838));
#32388=CARTESIAN_POINT('Ctrl Pts',(-45.6237335200226,17.8102574730284,-11.5604045561584));
#32389=CARTESIAN_POINT('Ctrl Pts',(-47.0873378224411,18.3423260668025,-11.8694761541428));
#32390=CARTESIAN_POINT('Ctrl Pts',(-48.547478432487,18.8718427994039,-11.8687142284812));
#32391=CARTESIAN_POINT('Ctrl Pts',(-34.8615042977019,14.752924178887,1.59647077610298));
#32392=CARTESIAN_POINT('Ctrl Pts',(-34.857025771947,14.7065009496435,1.1525917014061));
#32393=CARTESIAN_POINT('Ctrl Pts',(-34.8423730342687,14.6505019462284,0.635573044894269));
#32394=CARTESIAN_POINT('Ctrl Pts',(-34.9137340335311,14.4963699338419,-1.86858636178585));
#32395=CARTESIAN_POINT('Ctrl Pts',(-35.2957699604605,14.5381447126175,-3.71029995870396));
#32396=CARTESIAN_POINT('Ctrl Pts',(-36.7049156525828,14.9006586664088,-7.16936247493129));
#32397=CARTESIAN_POINT('Ctrl Pts',(-37.7093165664795,15.225799021172,-8.73699595771789));
#32398=CARTESIAN_POINT('Ctrl Pts',(-40.2121512288796,16.0925451480874,-11.3730256982019));
#32399=CARTESIAN_POINT('Ctrl Pts',(-41.6875985735023,16.6328052292555,-12.4235805192037));
#32400=CARTESIAN_POINT('Ctrl Pts',(-44.9414037540494,17.8377468919989,-13.8529470821786));
#32401=CARTESIAN_POINT('Ctrl Pts',(-46.6732919100457,18.4952436947636,-14.2204718556929));
#32402=CARTESIAN_POINT('Ctrl Pts',(-48.4187086763094,19.1537534053194,-14.2198708430667));
#32403=CARTESIAN_POINT('Ctrl Pts',(-33.8728645130296,16.9191631550061,1.59674373345245));
#32404=CARTESIAN_POINT('Ctrl Pts',(-33.8683874970857,16.8727555761311,1.15301430090585));
#32405=CARTESIAN_POINT('Ctrl Pts',(-33.8536050613443,16.816682478221,0.635579150075179));
#32406=CARTESIAN_POINT('Ctrl Pts',(-33.9233571178916,16.6618156863834,-1.86860431103318));
#32407=CARTESIAN_POINT('Ctrl Pts',(-34.3078598045327,16.7047171138864,-3.70979114470774));
#32408=CARTESIAN_POINT('Ctrl Pts',(-35.7142525408745,17.0659735848861,-7.17014261468798));
#32409=CARTESIAN_POINT('Ctrl Pts',(-36.7203421551987,17.3918853009154,-8.73670574475805));
#32410=CARTESIAN_POINT('Ctrl Pts',(-39.2225667173735,18.2583527463006,-11.3734544105071));
#32411=CARTESIAN_POINT('Ctrl Pts',(-40.6990131477318,18.7990691966228,-12.4221714958757));
#32412=CARTESIAN_POINT('Ctrl Pts',(-43.9517037462886,20.0035017021008,-13.8545909095101));
#32413=CARTESIAN_POINT('Ctrl Pts',(-45.6843449310646,20.6613231478728,-14.2195188099532));
#32414=CARTESIAN_POINT('Ctrl Pts',(-47.429532347212,21.3197474319156,-14.2201291128084));
#32415=CARTESIAN_POINT('Ctrl Pts',(-35.880019467837,18.1761744494742,1.47327608945385));
#32416=CARTESIAN_POINT('Ctrl Pts',(-35.8754049017175,18.1283410613835,1.015913678653));
#32417=CARTESIAN_POINT('Ctrl Pts',(-35.8636444578228,18.0751475421239,0.528588449421553));
#32418=CARTESIAN_POINT('Ctrl Pts',(-35.932461552811,17.9217737308839,-1.55405138012259));
#32419=CARTESIAN_POINT('Ctrl Pts',(-36.2649627130451,17.9378754148675,-3.10057294640886));
#32420=CARTESIAN_POINT('Ctrl Pts',(-37.4518844049458,18.2024961996707,-5.982274843344));
#32421=CARTESIAN_POINT('Ctrl Pts',(-38.3034500513458,18.4554759130143,-7.29352824389302));
#32422=CARTESIAN_POINT('Ctrl Pts',(-40.4061490373992,19.1405438219642,-9.49167634236476));
#32423=CARTESIAN_POINT('Ctrl Pts',(-41.6515092131746,19.5733634365479,-10.3690524868116));
#32424=CARTESIAN_POINT('Ctrl Pts',(-44.3761878888518,20.540254371427,-11.5624766483028));
#32425=CARTESIAN_POINT('Ctrl Pts',(-45.840743551661,21.0727284454457,-11.8682745705212));
#32426=CARTESIAN_POINT('Ctrl Pts',(-47.3005929134933,21.6021412371497,-11.8690397849987));
#32427=CARTESIAN_POINT('Ctrl Pts',(-37.603187989015,19.8012255369164,1.35541228259769));
#32428=CARTESIAN_POINT('Ctrl Pts',(-37.5984423520298,19.7520335023962,0.885059075367221));
#32429=CARTESIAN_POINT('Ctrl Pts',(-37.5895426312144,19.7015755924255,0.426408585758618));
#32430=CARTESIAN_POINT('Ctrl Pts',(-37.6571514683988,19.549483641906,-1.2536423221496));
#32431=CARTESIAN_POINT('Ctrl Pts',(-37.9404722137416,19.5402111378006,-2.51864171288158));
#32432=CARTESIAN_POINT('Ctrl Pts',(-38.9172493884832,19.7122939334796,-4.84795915807232));
#32433=CARTESIAN_POINT('Ctrl Pts',(-39.62156846681,19.8957713902405,-5.91517020464428));
#32434=CARTESIAN_POINT('Ctrl Pts',(-41.3425825071162,20.4075397474871,-7.69457540341882));
#32435=CARTESIAN_POINT('Ctrl Pts',(-42.3674404421148,20.7374023418884,-8.40795287041649));
#32436=CARTESIAN_POINT('Ctrl Pts',(-44.5876249069854,21.4773303202329,-9.37372383737288));
#32437=CARTESIAN_POINT('Ctrl Pts',(-45.7962902185241,21.8901596096075,-9.62254085999184));
#32438=CARTESIAN_POINT('Ctrl Pts',(-46.9835874904387,22.2963396064212,-9.62369151535377));
#32439=CARTESIAN_POINT('Ctrl Pts',(-38.9761478068776,21.7318648520658,1.24768188077471));
#32440=CARTESIAN_POINT('Ctrl Pts',(-38.9712826154474,21.6814335473931,0.765479302057181));
#32441=CARTESIAN_POINT('Ctrl Pts',(-38.9649724098685,21.6334621464558,0.332966384817446));
#32442=CARTESIAN_POINT('Ctrl Pts',(-39.0311461269804,21.482391674194,-0.978922014709598));
#32443=CARTESIAN_POINT('Ctrl Pts',(-39.2699975980932,21.450145680789,-1.98636136652356));
#32444=CARTESIAN_POINT('Ctrl Pts',(-40.0540327468988,21.5373444678476,-3.81078790535314));
#32445=CARTESIAN_POINT('Ctrl Pts',(-40.6240414198234,21.657420422293,-4.65460264910458));
#32446=CARTESIAN_POINT('Ctrl Pts',(-41.9958794973358,22.0106492051928,-6.051215124928));
#32447=CARTESIAN_POINT('Ctrl Pts',(-42.8192932220765,22.2464512872438,-6.61423873309801));
#32448=CARTESIAN_POINT('Ctrl Pts',(-44.5778891652326,22.7787172285086,-7.37244739476607));
#32449=CARTESIAN_POINT('Ctrl Pts',(-45.5526929856396,23.0822022983076,-7.56862230169532));
#32450=CARTESIAN_POINT('Ctrl Pts',(-46.4906987626549,23.3756641324467,-7.57037421505994));
#32451=CARTESIAN_POINT('Ctrl Pts',(-31.1202396243797,21.567561713547,1.59674381934676));
#32452=CARTESIAN_POINT('Ctrl Pts',(-31.1224126652072,21.520989348265,1.15301435962634));
#32453=CARTESIAN_POINT('Ctrl Pts',(-31.1157607260923,21.4633832297208,0.635579189057524));
#32454=CARTESIAN_POINT('Ctrl Pts',(-31.2068426511149,21.320019509059,-1.86860431103819));
#32455=CARTESIAN_POINT('Ctrl Pts',(-31.5813261451172,21.4172046994746,-3.70979114470734));
#32456=CARTESIAN_POINT('Ctrl Pts',(-32.9219916749895,21.9749346552901,-7.17014261468839));
#32457=CARTESIAN_POINT('Ctrl Pts',(-33.8714586745438,22.4407105406856,-8.73670574473668));
#32458=CARTESIAN_POINT('Ctrl Pts',(-36.2249030242442,23.6544622808116,-11.3734544105284));
#32459=CARTESIAN_POINT('Ctrl Pts',(-37.609369384537,24.39979525241,-12.4221714958177));
#32460=CARTESIAN_POINT('Ctrl Pts',(-40.6575436657173,26.0548745077421,-13.854590909568));
#32461=CARTESIAN_POINT('Ctrl Pts',(-42.2789313088126,26.9525808298053,-14.2195188100055));
#32462=CARTESIAN_POINT('Ctrl Pts',(-43.9126516878553,27.8526693689671,-14.2201291128083));
#32463=CARTESIAN_POINT('Ctrl Pts',(-32.9280732767458,23.0974263782808,1.47327617534825));
#32464=CARTESIAN_POINT('Ctrl Pts',(-32.9303130812698,23.0494231409436,1.01591373651662));
#32465=CARTESIAN_POINT('Ctrl Pts',(-32.9262425677185,22.9950973654565,0.528588481838949));
#32466=CARTESIAN_POINT('Ctrl Pts',(-33.0161865744697,22.8530783700625,-1.55405138011843));
#32467=CARTESIAN_POINT('Ctrl Pts',(-33.3430118437576,22.9163360109255,-3.10057294640473));
#32468=CARTESIAN_POINT('Ctrl Pts',(-34.4801929200291,23.347179906303,-5.98227484334812));
#32469=CARTESIAN_POINT('Ctrl Pts',(-35.287088088999,23.7187750781554,-7.29352824388356));
#32470=CARTESIAN_POINT('Ctrl Pts',(-37.2708893025901,24.6961152497751,-9.49167634237414));
#32471=CARTESIAN_POINT('Ctrl Pts',(-38.441976853959,25.3017626168119,-10.3690524867345));
#32472=CARTESIAN_POINT('Ctrl Pts',(-41.0013193023666,26.6465742010366,-11.5624766483798));
#32473=CARTESIAN_POINT('Ctrl Pts',(-42.3751889385489,27.3820564590927,-11.8682745706115));
#32474=CARTESIAN_POINT('Ctrl Pts',(-43.7448358429354,28.1138388177854,-11.8690397849987));
#32475=CARTESIAN_POINT('Ctrl Pts',(-34.402433544287,24.951169238192,1.35541236849215));
#32476=CARTESIAN_POINT('Ctrl Pts',(-34.4047369675988,24.9018025300722,0.885059132417908));
#32477=CARTESIAN_POINT('Ctrl Pts',(-34.4031087413091,24.8505916427384,0.426408611904495));
#32478=CARTESIAN_POINT('Ctrl Pts',(-34.491674360816,24.7096695075291,-1.25364232213153));
#32479=CARTESIAN_POINT('Ctrl Pts',(-34.7734309243617,24.740812130188,-2.51864171287491));
#32480=CARTESIAN_POINT('Ctrl Pts',(-35.7157759805954,25.0501532567791,-4.84795915807897));
#32481=CARTESIAN_POINT('Ctrl Pts',(-36.3868145416537,25.3319982332986,-5.91517020464913));
#32482=CARTESIAN_POINT('Ctrl Pts',(-38.0174789095801,26.083483361411,-7.69457540341387));
#32483=CARTESIAN_POINT('Ctrl Pts',(-38.984960926787,26.5558409214617,-8.4079528702915));
#32484=CARTESIAN_POINT('Ctrl Pts',(-41.0772443843504,27.6042026929775,-9.37372383749777));
#32485=CARTESIAN_POINT('Ctrl Pts',(-42.2148554923058,28.1848409837727,-9.6225408600775));
#32486=CARTESIAN_POINT('Ctrl Pts',(-43.332262349351,28.7558566730953,-9.62369151535374));
#32487=CARTESIAN_POINT('Ctrl Pts',(-35.486659988949,27.0575499832999,1.24768196666921));
#32488=CARTESIAN_POINT('Ctrl Pts',(-35.4890214412267,27.0069396045613,0.765479358370163));
#32489=CARTESIAN_POINT('Ctrl Pts',(-35.4896025055318,26.9585584436997,0.332966405226273));
#32490=CARTESIAN_POINT('Ctrl Pts',(-35.5766022409445,26.8184431506731,-0.97892201467345));
#32491=CARTESIAN_POINT('Ctrl Pts',(-35.8176116317276,26.8205174834717,-1.98636136651437));
#32492=CARTESIAN_POINT('Ctrl Pts',(-36.5812567518819,27.0184085480268,-3.81078790536229));
#32493=CARTESIAN_POINT('Ctrl Pts',(-37.1283749683434,27.2183829944883,-4.65460264912373));
#32494=CARTESIAN_POINT('Ctrl Pts',(-38.4359800152259,27.7632493318237,-6.05121512490869));
#32495=CARTESIAN_POINT('Ctrl Pts',(-39.2174544404323,28.1138352796401,-6.61423873291071));
#32496=CARTESIAN_POINT('Ctrl Pts',(-40.8824010709582,28.8909578185445,-7.37244739495321));
#32497=CARTESIAN_POINT('Ctrl Pts',(-41.8040923655509,29.3300828959434,-7.56862230183338));
#32498=CARTESIAN_POINT('Ctrl Pts',(-42.6907866227634,29.7540498521221,-7.57037421505989));
#32499=CARTESIAN_POINT('Ctrl Pts',(-31.1388779521428,21.4269965203143,6.66133814775094E-16));
#32500=CARTESIAN_POINT('Ctrl Pts',(-31.2068426511149,21.320019509059,-1.86860431103819));
#32501=CARTESIAN_POINT('Ctrl Pts',(-31.5813261451172,21.4172046994746,-3.70979114470734));
#32502=CARTESIAN_POINT('Ctrl Pts',(-32.9219916749895,21.9749346552901,-7.17014261468839));
#32503=CARTESIAN_POINT('Ctrl Pts',(-33.8714586745438,22.4407105406856,-8.73670574473668));
#32504=CARTESIAN_POINT('Ctrl Pts',(-35.174500005265,23.1127335196102,-10.1966053555722));
#32505=CARTESIAN_POINT('Ctrl Pts',(-35.3032131351478,23.1794761614689,-10.3350231942278));
#32506=CARTESIAN_POINT('Ctrl Pts',(-35.4342359672601,23.247744751939,-10.4702558450996));
#32507=CARTESIAN_POINT('Ctrl Pts',(-39.2156436908076,21.2519768052527,1.24689101061711));
#32508=CARTESIAN_POINT('Ctrl Pts',(-39.2180072667082,21.2013209149781,0.764254780044368));
#32509=CARTESIAN_POINT('Ctrl Pts',(-39.2189297793852,21.1532057605131,0.332948714099626));
#32510=CARTESIAN_POINT('Ctrl Pts',(-39.3102413217382,21.0158614973477,-0.978870002719474));
#32511=CARTESIAN_POINT('Ctrl Pts',(-39.5446400894402,21.0136870730836,-1.98783577088449));
#32512=CARTESIAN_POINT('Ctrl Pts',(-40.3156627552177,21.2163201816587,-3.80852727284038));
#32513=CARTESIAN_POINT('Ctrl Pts',(-40.8582554869351,21.4133857818112,-4.65544360722271));
#32514=CARTESIAN_POINT('Ctrl Pts',(-42.1674955178514,21.959303041602,-6.04997283343062));
#32515=CARTESIAN_POINT('Ctrl Pts',(-42.9462925343072,22.3081680037475,-6.61832169909177));
#32516=CARTESIAN_POINT('Ctrl Pts',(-44.6142260746748,23.0872105665078,-7.36768403072499));
#32517=CARTESIAN_POINT('Ctrl Pts',(-45.5338656769843,23.5251300588861,-7.57138648682314));
#32518=CARTESIAN_POINT('Ctrl Pts',(-46.4212082443694,23.9494005117262,-7.56962581969446));
#32519=CARTESIAN_POINT('Ctrl Pts',(-36.8491669828396,21.1419034541629,1.35489339099699));
#32520=CARTESIAN_POINT('Ctrl Pts',(-36.8514717995443,21.0925068841255,0.884255638228302));
#32521=CARTESIAN_POINT('Ctrl Pts',(-36.8500676110146,21.0414705340931,0.426397004057789));
#32522=CARTESIAN_POINT('Ctrl Pts',(-36.9414623772912,20.9023665809846,-1.25360819503494));
#32523=CARTESIAN_POINT('Ctrl Pts',(-37.2188814500308,20.930721426378,-2.51960912779677));
#32524=CARTESIAN_POINT('Ctrl Pts',(-38.1660672052366,21.2431739952863,-4.84647586782401));
#32525=CARTESIAN_POINT('Ctrl Pts',(-38.8341364170724,21.5231103628896,-5.91572199046653));
#32526=CARTESIAN_POINT('Ctrl Pts',(-40.4658735625807,22.2752850427188,-7.69376028692058));
#32527=CARTESIAN_POINT('Ctrl Pts',(-41.4315988261873,22.7465133961231,-8.4106318656095));
#32528=CARTESIAN_POINT('Ctrl Pts',(-43.5258421132404,23.7961349710949,-9.37059840615683));
#32529=CARTESIAN_POINT('Ctrl Pts',(-44.662114427036,24.3759711161915,-9.6243537862471));
#32530=CARTESIAN_POINT('Ctrl Pts',(-45.7799392638233,24.9471970554251,-9.62320046360553));
#32531=CARTESIAN_POINT('Ctrl Pts',(-34.5502037758216,20.5719668778723,1.47293210467427));
#32532=CARTESIAN_POINT('Ctrl Pts',(-34.5524445041311,20.5239438427405,1.01538103752678));
#32533=CARTESIAN_POINT('Ctrl Pts',(-34.5485225226913,20.4697337816475,0.52858078609168));
#32534=CARTESIAN_POINT('Ctrl Pts',(-34.6403421915888,20.3289202010311,-1.55402875460338));
#32535=CARTESIAN_POINT('Ctrl Pts',(-34.9642917997815,20.3903296068275,-3.10121432123848));
#32536=CARTESIAN_POINT('Ctrl Pts',(-36.1046821530982,20.8232363200899,-5.98129145450567));
#32537=CARTESIAN_POINT('Ctrl Pts',(-36.909608708792,21.193566126174,-7.29389406575294));
#32538=CARTESIAN_POINT('Ctrl Pts',(-38.8941211503306,22.1713634554236,-9.49113593805375));
#32539=CARTESIAN_POINT('Ctrl Pts',(-40.0640440126769,22.7762621832733,-10.3708286017602));
#32540=CARTESIAN_POINT('Ctrl Pts',(-42.6246857849653,24.1219089895008,-11.560404556082));
#32541=CARTESIAN_POINT('Ctrl Pts',(-43.9976714499894,24.85685450176,-11.8694761541476));
#32542=CARTESIAN_POINT('Ctrl Pts',(-45.3675918458117,25.5887811923515,-11.8687142284812));
#32543=CARTESIAN_POINT('Ctrl Pts',(-32.4071044310924,19.5640700378122,1.59647086199739));
#32544=CARTESIAN_POINT('Ctrl Pts',(-32.4092782047768,19.5174819665907,1.15259176009847));
#32545=CARTESIAN_POINT('Ctrl Pts',(-32.4027440988122,19.4599676463217,0.635573083885156));
#32546=CARTESIAN_POINT('Ctrl Pts',(-32.4953140197739,19.3175602025112,-1.86858636181704));
#32547=CARTESIAN_POINT('Ctrl Pts',(-32.867516200987,19.413279155377,-3.71029995870358));
#32548=CARTESIAN_POINT('Ctrl Pts',(-34.210727707086,19.9726455810862,-7.16936247493171));
#32549=CARTESIAN_POINT('Ctrl Pts',(-35.1586329709074,20.4374176294472,-8.73699595769419));
#32550=CARTESIAN_POINT('Ctrl Pts',(-37.5126415503381,21.6515320408062,-11.3730256982257));
#32551=CARTESIAN_POINT('Ctrl Pts',(-38.8961839422237,22.3962711037012,-12.4235805192657));
#32552=CARTESIAN_POINT('Ctrl Pts',(-41.9453890000128,24.0520129554125,-13.8529470821167));
#32553=CARTESIAN_POINT('Ctrl Pts',(-43.5660774805196,24.9492907716475,-14.2204718556786));
#32554=CARTESIAN_POINT('Ctrl Pts',(-45.2000127177929,25.8494965077555,-14.2198708430667));
#32555=CARTESIAN_POINT('Ctrl Pts',(-32.4262389885812,19.423823646631,6.93889390390723E-15));
#32556=CARTESIAN_POINT('Ctrl Pts',(-32.4953140197739,19.3175602025112,-1.86858636181704));
#32557=CARTESIAN_POINT('Ctrl Pts',(-32.867516200987,19.413279155377,-3.71029995870358));
#32558=CARTESIAN_POINT('Ctrl Pts',(-34.210727707086,19.9726455810862,-7.16936247493171));
#32559=CARTESIAN_POINT('Ctrl Pts',(-35.1586329709074,20.4374176294472,-8.73699595769419));
#32560=CARTESIAN_POINT('Ctrl Pts',(-36.4553678306327,21.106227630677,-10.1890856763504));
#32561=CARTESIAN_POINT('Ctrl Pts',(-36.5772356450577,21.1694051501756,-10.3203928635177));
#32562=CARTESIAN_POINT('Ctrl Pts',(-36.7011717789913,21.2339499719654,-10.4488603766012));
#32563=CARTESIAN_POINT('Ctrl Pts',(-32.4071044310924,19.5640700378122,1.59647086199739));
#32564=CARTESIAN_POINT('Ctrl Pts',(-32.4092782047768,19.5174819665907,1.15259176009847));
#32565=CARTESIAN_POINT('Ctrl Pts',(-32.4027440988122,19.4599676463217,0.635573083885156));
#32566=CARTESIAN_POINT('Ctrl Pts',(-32.4953140197739,19.3175602025112,-1.86858636181704));
#32567=CARTESIAN_POINT('Ctrl Pts',(-32.867516200987,19.413279155377,-3.71029995870358));
#32568=CARTESIAN_POINT('Ctrl Pts',(-34.210727707086,19.9726455810862,-7.16936247493171));
#32569=CARTESIAN_POINT('Ctrl Pts',(-35.1586329709074,20.4374176294472,-8.73699595769419));
#32570=CARTESIAN_POINT('Ctrl Pts',(-37.5126415503381,21.6515320408062,-11.3730256982257));
#32571=CARTESIAN_POINT('Ctrl Pts',(-38.8961839422237,22.3962711037012,-12.4235805192657));
#32572=CARTESIAN_POINT('Ctrl Pts',(-41.9453890000128,24.0520129554125,-13.8529470821167));
#32573=CARTESIAN_POINT('Ctrl Pts',(-43.5660774805196,24.9492907716475,-14.2204718556786));
#32574=CARTESIAN_POINT('Ctrl Pts',(-45.2000127177929,25.8494965077555,-14.2198708430667));
#32575=CARTESIAN_POINT('Ctrl Pts',(-31.4917047963494,19.8251119861393,1.62964630360494));
#32576=CARTESIAN_POINT('Ctrl Pts',(-31.4938604347888,19.7789125871878,1.18947037065042));
#32577=CARTESIAN_POINT('Ctrl Pts',(-31.48659515468,19.7204885321119,0.664244043766078));
#32578=CARTESIAN_POINT('Ctrl Pts',(-31.5789716511435,19.577400497487,-1.95287905131582));
#32579=CARTESIAN_POINT('Ctrl Pts',(-31.9647082138306,19.6827016274759,-3.87337387078821));
#32580=CARTESIAN_POINT('Ctrl Pts',(-33.3615921546903,20.275520006293,-7.48792130213766));
#32581=CARTESIAN_POINT('Ctrl Pts',(-34.3482235804788,20.7658646320009,-9.12360836230511));
#32582=CARTESIAN_POINT('Ctrl Pts',(-36.801091683951,22.0432057314057,-11.8774049927262));
#32583=CARTESIAN_POINT('Ctrl Pts',(-38.2421198758022,22.8255734412324,-12.9732563609011));
#32584=CARTESIAN_POINT('Ctrl Pts',(-41.4219656612033,24.5642317984951,-14.4676858045338));
#32585=CARTESIAN_POINT('Ctrl Pts',(-43.1092121218766,25.5051223583055,-14.8501851005342));
#32586=CARTESIAN_POINT('Ctrl Pts',(-44.8138361237939,26.4503875219919,-14.8499483202528));
#32587=CARTESIAN_POINT('Ctrl Pts',(-30.9769588736643,20.6265086564332,1.62975548654469));
#32588=CARTESIAN_POINT('Ctrl Pts',(-30.9791142189643,20.5803155398589,1.1896394104614));
#32589=CARTESIAN_POINT('Ctrl Pts',(-30.9718018055912,20.5218547654718,0.664246485835027));
#32590=CARTESIAN_POINT('Ctrl Pts',(-31.0635831036823,20.3783842201051,-1.95288623100427));
#32591=CARTESIAN_POINT('Ctrl Pts',(-31.4502321914808,20.4842718451115,-3.87317034518997));
#32592=CARTESIAN_POINT('Ctrl Pts',(-32.8460977418536,21.0764356359779,-7.48823335804009));
#32593=CARTESIAN_POINT('Ctrl Pts',(-33.8333538619286,21.5671817964958,-9.12349227712162));
#32594=CARTESIAN_POINT('Ctrl Pts',(-36.2859962735183,22.8443778274084,-11.8775764776478));
#32595=CARTESIAN_POINT('Ctrl Pts',(-37.7273940527265,23.6269831007203,-12.9726927515238));
#32596=CARTESIAN_POINT('Ctrl Pts',(-40.906827527486,25.3653764194226,-14.4683433355124));
#32597=CARTESIAN_POINT('Ctrl Pts',(-42.5943534696917,26.3064386089228,-14.8498038985481));
#32598=CARTESIAN_POINT('Ctrl Pts',(-44.2988917118189,27.2516566664766,-14.8500516281495));
#32599=CARTESIAN_POINT('Ctrl Pts',(-31.1202396243797,21.567561713547,1.59674381934676));
#32600=CARTESIAN_POINT('Ctrl Pts',(-31.1224126652072,21.520989348265,1.15301435962634));
#32601=CARTESIAN_POINT('Ctrl Pts',(-31.1157607260923,21.4633832297208,0.635579189057524));
#32602=CARTESIAN_POINT('Ctrl Pts',(-31.2068426511149,21.320019509059,-1.86860431103819));
#32603=CARTESIAN_POINT('Ctrl Pts',(-31.5813261451172,21.4172046994746,-3.70979114470735));
#32604=CARTESIAN_POINT('Ctrl Pts',(-32.9219916749894,21.9749346552901,-7.17014261468839));
#32605=CARTESIAN_POINT('Ctrl Pts',(-33.871458674539,22.440710540688,-8.73670574473669));
#32606=CARTESIAN_POINT('Ctrl Pts',(-36.224903024249,23.6544622808092,-11.3734544105285));
#32607=CARTESIAN_POINT('Ctrl Pts',(-37.609369384537,24.3997952524124,-12.4221714958129));
#32608=CARTESIAN_POINT('Ctrl Pts',(-40.6575436657173,26.0548745077397,-13.8545909095728));
#32609=CARTESIAN_POINT('Ctrl Pts',(-42.2789313088166,26.9525808297997,-14.2195188100245));
#32610=CARTESIAN_POINT('Ctrl Pts',(-43.9126516878553,27.8526693689671,-14.2201291128084));
#32611=CARTESIAN_POINT('Ctrl Pts',(-29.2929893708797,23.9769478445538,1.59647090706387));
#32612=CARTESIAN_POINT('Ctrl Pts',(-29.3017711927823,23.9311433314971,1.15259179089162));
#32613=CARTESIAN_POINT('Ctrl Pts',(-29.3034887354907,23.8732845217124,0.635573104344381));
#32614=CARTESIAN_POINT('Ctrl Pts',(-29.4153831213449,23.7455006526433,-1.86858636183877));
#32615=CARTESIAN_POINT('Ctrl Pts',(-29.7701745938413,23.8932152177425,-3.71029995868823));
#32616=CARTESIAN_POINT('Ctrl Pts',(-31.0201080009748,24.6380470281508,-7.16936247494709));
#32617=CARTESIAN_POINT('Ctrl Pts',(-31.8922209971496,25.2329893514979,-8.73699595771819));
#32618=CARTESIAN_POINT('Ctrl Pts',(-34.04948266738,26.769756178971,-11.3730256982017));
#32619=CARTESIAN_POINT('Ctrl Pts',(-35.3129551733011,27.7038134838192,-12.4235805192756));
#32620=CARTESIAN_POINT('Ctrl Pts',(-38.0954870863618,29.7766493955002,-13.8529470821068));
#32621=CARTESIAN_POINT('Ctrl Pts',(-39.5719833475633,30.8954422364741,-14.2204718557262));
#32622=CARTESIAN_POINT('Ctrl Pts',(-41.0611748464153,32.0190184050857,-14.2198708430667));
#32623=CARTESIAN_POINT('Ctrl Pts',(-28.3497570418624,24.1050578112644,1.62964634867147));
#32624=CARTESIAN_POINT('Ctrl Pts',(-28.3584655992857,24.0596354334535,1.18947040156752));
#32625=CARTESIAN_POINT('Ctrl Pts',(-28.3595888789042,24.000772091711,0.66424406514856));
#32626=CARTESIAN_POINT('Ctrl Pts',(-28.4713886672159,23.8722870320852,-1.95287905133948));
#32627=CARTESIAN_POINT('Ctrl Pts',(-28.8382130746991,24.0314123848382,-3.87337387078001));
#32628=CARTESIAN_POINT('Ctrl Pts',(-30.1365118993193,24.8169940396349,-7.48792130214588));
#32629=CARTESIAN_POINT('Ctrl Pts',(-31.0433175237566,25.4427599558226,-9.12360836232668));
#32630=CARTESIAN_POINT('Ctrl Pts',(-33.2894343747244,27.0561790919793,-11.8774049927046));
#32631=CARTESIAN_POINT('Ctrl Pts',(-34.6044524432567,28.0356631207245,-12.973256360911));
#32632=CARTESIAN_POINT('Ctrl Pts',(-37.5044951006137,30.2091636815072,-14.4676858045239));
#32633=CARTESIAN_POINT('Ctrl Pts',(-39.0406651371294,31.3805975394391,-14.8501851005484));
#32634=CARTESIAN_POINT('Ctrl Pts',(-40.5934132658116,32.5588345556907,-14.8499483202528));
#32635=CARTESIAN_POINT('Ctrl Pts',(-27.7261998529423,24.8250414362346,1.62975553161125));
#32636=CARTESIAN_POINT('Ctrl Pts',(-27.7349072261382,24.7796252351385,1.18963944138304));
#32637=CARTESIAN_POINT('Ctrl Pts',(-27.7359890779435,24.720718840073,0.664246507217367));
#32638=CARTESIAN_POINT('Ctrl Pts',(-27.8472541630979,24.5917704575537,-1.95288623102729));
#32639=CARTESIAN_POINT('Ctrl Pts',(-28.2148983405374,24.751606201496,-3.87317034519134));
#32640=CARTESIAN_POINT('Ctrl Pts',(-29.5122822980333,25.536394999056,-7.48823335803871));
#32641=CARTESIAN_POINT('Ctrl Pts',(-30.4196491139021,26.1626472662679,-9.12349227714079));
#32642=CARTESIAN_POINT('Ctrl Pts',(-32.6655632155794,27.7758906912001,-11.8775764776286));
#32643=CARTESIAN_POINT('Ctrl Pts',(-33.9809133008013,28.7556624631466,-12.9726927515193));
#32644=CARTESIAN_POINT('Ctrl Pts',(-36.8805855631737,30.9288420051638,-14.4683433355169));
#32645=CARTESIAN_POINT('Ctrl Pts',(-38.4170078110451,32.1004855202031,-14.849803898529));
#32646=CARTESIAN_POINT('Ctrl Pts',(-39.9696777567512,33.2786637049092,-14.8500516281495));
#32647=CARTESIAN_POINT('Ctrl Pts',(-27.7340963985795,25.7769069069792,1.59674386441333));
#32648=CARTESIAN_POINT('Ctrl Pts',(-27.7428752599128,25.7311178357017,1.15301439043128));
#32649=CARTESIAN_POINT('Ctrl Pts',(-27.7444892330881,25.6731513926165,0.635579209516401));
#32650=CARTESIAN_POINT('Ctrl Pts',(-27.8550468610524,25.5442092163171,-1.8686043110583));
#32651=CARTESIAN_POINT('Ctrl Pts',(-28.2118877584287,25.6936997593906,-3.70979114471355));
#32652=CARTESIAN_POINT('Ctrl Pts',(-29.459533997768,26.4365494266998,-7.17014261468215));
#32653=CARTESIAN_POINT('Ctrl Pts',(-30.3330499725088,27.0327076276087,-8.73670574475106));
#32654=CARTESIAN_POINT('Ctrl Pts',(-32.4898047695223,28.5690351770253,-11.373454410514));
#32655=CARTESIAN_POINT('Ctrl Pts',(-33.7541073171722,29.5038118398731,-12.4221714958132));
#32656=CARTESIAN_POINT('Ctrl Pts',(-36.5357132427521,31.5758452046431,-13.8545909095725));
#32657=CARTESIAN_POINT('Ctrl Pts',(-38.0128405673296,32.6951616910819,-14.2195188099437));
#32658=CARTESIAN_POINT('Ctrl Pts',(-39.5018360737643,33.8185912781321,-14.2201291128084));
#32659=CARTESIAN_POINT('Ctrl Pts',(-29.331888309534,23.8408520862201,0.));
#32660=CARTESIAN_POINT('Ctrl Pts',(-29.4153831213449,23.7455006526433,-1.86858636183877));
#32661=CARTESIAN_POINT('Ctrl Pts',(-29.7701745938413,23.8932152177425,-3.71029995868823));
#32662=CARTESIAN_POINT('Ctrl Pts',(-31.0201080009748,24.6380470281508,-7.16936247494709));
#32663=CARTESIAN_POINT('Ctrl Pts',(-31.8922209971496,25.2329893514979,-8.73699595771819));
#32664=CARTESIAN_POINT('Ctrl Pts',(-33.0805753786004,26.0795364430711,-10.1890856763491));
#32665=CARTESIAN_POINT('Ctrl Pts',(-33.1922116559259,26.1594145048145,-10.3203928635157));
#32666=CARTESIAN_POINT('Ctrl Pts',(-33.3057006128448,26.2409403042404,-10.4488603765989));
#32667=CARTESIAN_POINT('Ctrl Pts',(-27.7725495286736,25.640424970686,5.55111512312578E-17));
#32668=CARTESIAN_POINT('Ctrl Pts',(-27.8550468610524,25.5442092163171,-1.8686043110583));
#32669=CARTESIAN_POINT('Ctrl Pts',(-28.2118877584287,25.6936997593906,-3.70979114471355));
#32670=CARTESIAN_POINT('Ctrl Pts',(-29.459533997768,26.4365494266998,-7.17014261468215));
#32671=CARTESIAN_POINT('Ctrl Pts',(-30.3330499725088,27.0327076276087,-8.73670574475106));
#32672=CARTESIAN_POINT('Ctrl Pts',(-31.5271893797574,27.8833324977795,-10.1966053555727));
#32673=CARTESIAN_POINT('Ctrl Pts',(-31.6450939272868,27.9677135840395,-10.335023194229));
#32674=CARTESIAN_POINT('Ctrl Pts',(-31.7650675024774,28.0539337918545,-10.4702558451016));
#32675=CARTESIAN_POINT('Ctrl Pts',(-35.7920133394053,26.6166303184858,1.24689105568334));
#32676=CARTESIAN_POINT('Ctrl Pts',(-35.8015619426389,26.5668264024534,0.764254809553763));
#32677=CARTESIAN_POINT('Ctrl Pts',(-35.8093225655934,26.5193322760963,0.332948724812664));
#32678=CARTESIAN_POINT('Ctrl Pts',(-35.9192508155956,26.396380965825,-0.978870002717184));
#32679=CARTESIAN_POINT('Ctrl Pts',(-36.151573194664,26.4275870969477,-1.98783577086484));
#32680=CARTESIAN_POINT('Ctrl Pts',(-36.885910263345,26.7378856583767,-3.80852727286012));
#32681=CARTESIAN_POINT('Ctrl Pts',(-37.394934824389,27.0101644118135,-4.65544360724195));
#32682=CARTESIAN_POINT('Ctrl Pts',(-38.6131565530345,27.7368493043946,-6.04997283341153));
#32683=CARTESIAN_POINT('Ctrl Pts',(-39.3343778781397,28.1929976956455,-6.61832169911591));
#32684=CARTESIAN_POINT('Ctrl Pts',(-40.8744649436646,29.2014824204577,-7.36768403070085));
#32685=CARTESIAN_POINT('Ctrl Pts',(-41.722421499192,29.7658228850063,-7.57138648695631));
#32686=CARTESIAN_POINT('Ctrl Pts',(-42.5403522177283,30.3120568904488,-7.56962581969436));
#32687=CARTESIAN_POINT('Ctrl Pts',(-33.4652890233053,26.1708926054255,1.35489343606331));
#32688=CARTESIAN_POINT('Ctrl Pts',(-33.4746002454611,26.1223268292986,0.884255668136539));
#32689=CARTESIAN_POINT('Ctrl Pts',(-33.4804735791531,26.0716101167974,0.426397017780271));
#32690=CARTESIAN_POINT('Ctrl Pts',(-33.5907346359763,25.9469288716972,-1.25360819503973));
#32691=CARTESIAN_POINT('Ctrl Pts',(-33.8612946673472,26.0144759562051,-2.51960912778176));
#32692=CARTESIAN_POINT('Ctrl Pts',(-34.7543728004411,26.4585467959166,-4.84647586783908));
#32693=CARTESIAN_POINT('Ctrl Pts',(-35.3758029321054,26.8307099768199,-5.91572199047857));
#32694=CARTESIAN_POINT('Ctrl Pts',(-36.8838857283486,27.8074490109549,-7.69376028690863));
#32695=CARTESIAN_POINT('Ctrl Pts',(-37.7727185143269,28.411317973868,-8.41063186563368));
#32696=CARTESIAN_POINT('Ctrl Pts',(-39.6962686996607,29.7482978093359,-9.37059840613264));
#32697=CARTESIAN_POINT('Ctrl Pts',(-40.7384561124906,30.4839404690763,-9.62435378635169));
#32698=CARTESIAN_POINT('Ctrl Pts',(-41.7636091770245,31.2084352127806,-9.62320046360546));
#32699=CARTESIAN_POINT('Ctrl Pts',(-31.2708363785844,25.2795805846979,1.47293214974068));
#32700=CARTESIAN_POINT('Ctrl Pts',(-31.2798886902769,25.2323652421878,1.01538106786831));
#32701=CARTESIAN_POINT('Ctrl Pts',(-31.2837215247332,25.1781488031011,0.528580803105061));
#32702=CARTESIAN_POINT('Ctrl Pts',(-31.3946464646314,25.0518358019868,-1.55402875461628));
#32703=CARTESIAN_POINT('Ctrl Pts',(-31.7065592633163,25.1587229846853,-3.1012143212269));
#32704=CARTESIAN_POINT('Ctrl Pts',(-32.7737330381668,25.7495178005034,-5.9812914545173));
#32705=CARTESIAN_POINT('Ctrl Pts',(-33.5177631757073,26.2306311757364,-7.29389406577215));
#32706=CARTESIAN_POINT('Ctrl Pts',(-35.3429210732647,27.4809015051985,-9.4911359380346));
#32707=CARTESIAN_POINT('Ctrl Pts',(-36.4148497431273,28.246140619147,-10.3708286017653));
#32708=CARTESIAN_POINT('Ctrl Pts',(-38.7579223667115,29.9425080008419,-11.560404556077));
#32709=CARTESIAN_POINT('Ctrl Pts',(-40.0123393655922,30.8653690604201,-11.8694761541998));
#32710=CARTESIAN_POINT('Ctrl Pts',(-41.2641519184871,31.7848057921741,-11.8687142284812));
#32711=CARTESIAN_POINT('Ctrl Pts',(-29.2929893708797,23.9769478445538,1.59647090706387));
#32712=CARTESIAN_POINT('Ctrl Pts',(-29.3017711927823,23.9311433314971,1.15259179089162));
#32713=CARTESIAN_POINT('Ctrl Pts',(-29.3034887354907,23.8732845217124,0.635573104344381));
#32714=CARTESIAN_POINT('Ctrl Pts',(-29.4153831213449,23.7455006526433,-1.86858636183877));
#32715=CARTESIAN_POINT('Ctrl Pts',(-29.7701745938413,23.8932152177425,-3.71029995868823));
#32716=CARTESIAN_POINT('Ctrl Pts',(-31.0201080009748,24.6380470281508,-7.16936247494709));
#32717=CARTESIAN_POINT('Ctrl Pts',(-31.8922209971496,25.2329893514979,-8.73699595771819));
#32718=CARTESIAN_POINT('Ctrl Pts',(-34.04948266738,26.769756178971,-11.3730256982017));
#32719=CARTESIAN_POINT('Ctrl Pts',(-35.3129551733011,27.7038134838192,-12.4235805192756));
#32720=CARTESIAN_POINT('Ctrl Pts',(-38.0954870863618,29.7766493955002,-13.8529470821068));
#32721=CARTESIAN_POINT('Ctrl Pts',(-39.5719833475633,30.8954422364741,-14.2204718557262));
#32722=CARTESIAN_POINT('Ctrl Pts',(-41.0611748464153,32.0190184050857,-14.2198708430667));
#32723=CARTESIAN_POINT('Ctrl Pts',(-27.7340963985795,25.7769069069792,1.59674386441333));
#32724=CARTESIAN_POINT('Ctrl Pts',(-27.7428752599097,25.7311178357017,1.15301439043125));
#32725=CARTESIAN_POINT('Ctrl Pts',(-27.7444892330881,25.6731513926165,0.635579209516401));
#32726=CARTESIAN_POINT('Ctrl Pts',(-27.8550468610524,25.5442092163171,-1.8686043110583));
#32727=CARTESIAN_POINT('Ctrl Pts',(-28.2118877584311,25.6936997593906,-3.70979114471235));
#32728=CARTESIAN_POINT('Ctrl Pts',(-29.4595339977656,26.4365494266998,-7.17014261468335));
#32729=CARTESIAN_POINT('Ctrl Pts',(-30.3330499725136,27.0327076276087,-8.73670574475107));
#32730=CARTESIAN_POINT('Ctrl Pts',(-32.4898047695175,28.5690351770252,-11.373454410514));
#32731=CARTESIAN_POINT('Ctrl Pts',(-33.7541073171722,29.5038118398683,-12.4221714958132));
#32732=CARTESIAN_POINT('Ctrl Pts',(-36.5357132427521,31.5758452046479,-13.8545909095725));
#32733=CARTESIAN_POINT('Ctrl Pts',(-38.0128405673159,32.6951616910965,-14.2195188099295));
#32734=CARTESIAN_POINT('Ctrl Pts',(-39.5018360737643,33.8185912781321,-14.2201291128084));
#32735=CARTESIAN_POINT('Ctrl Pts',(-29.3058064687038,27.5484813091701,1.47327622041476));
#32736=CARTESIAN_POINT('Ctrl Pts',(-29.314855048509,27.5012854314731,1.01591376687318));
#32737=CARTESIAN_POINT('Ctrl Pts',(-29.318557330564,27.4469333174803,0.528588498851873));
#32738=CARTESIAN_POINT('Ctrl Pts',(-29.4277972482719,27.3191602364301,-1.55405138012929));
#32739=CARTESIAN_POINT('Ctrl Pts',(-29.7422934066125,27.4282860909958,-3.10057294641829));
#32740=CARTESIAN_POINT('Ctrl Pts',(-30.8065841399506,28.016582357811,-5.98227484333453));
#32741=CARTESIAN_POINT('Ctrl Pts',(-31.5523827727639,28.4992283820582,-7.29352824389315));
#32742=CARTESIAN_POINT('Ctrl Pts',(-33.3769017419046,29.7489449887618,-9.49167634236451));
#32743=CARTESIAN_POINT('Ctrl Pts',(-34.4498767034895,30.5150908743752,-10.36905248673));
#32744=CARTESIAN_POINT('Ctrl Pts',(-36.7917820929404,32.2104466223681,-11.5624766483843));
#32745=CARTESIAN_POINT('Ctrl Pts',(-38.0469976785282,33.1339647666331,-11.8682745705308));
#32746=CARTESIAN_POINT('Ctrl Pts',(-39.2985600643046,34.0532197137072,-11.8690397849988));
#32747=CARTESIAN_POINT('Ctrl Pts',(-30.5013447592649,29.5931790826756,1.35541241355863));
#32748=CARTESIAN_POINT('Ctrl Pts',(-30.5106503524477,29.5446426662131,0.885059162349099));
#32749=CARTESIAN_POINT('Ctrl Pts',(-30.5163267679929,29.4937213090629,0.426408625626303));
#32750=CARTESIAN_POINT('Ctrl Pts',(-30.6240462289741,29.3668377587799,-1.25364232213325));
#32751=CARTESIAN_POINT('Ctrl Pts',(-30.8985028595643,29.4377615341981,-2.51864171289819));
#32752=CARTESIAN_POINT('Ctrl Pts',(-31.7872323696267,29.8780636984644,-4.84795915805562));
#32753=CARTESIAN_POINT('Ctrl Pts',(-32.4113300033956,30.2525386438001,-5.91517020464911));
#32754=CARTESIAN_POINT('Ctrl Pts',(-33.9184490747425,31.2284424726283,-7.69457540341378));
#32755=CARTESIAN_POINT('Ctrl Pts',(-34.8088600302747,31.8336791606204,-8.40795287028212));
#32756=CARTESIAN_POINT('Ctrl Pts',(-36.7306496230996,33.1691331028151,-9.37372383750715));
#32757=CARTESIAN_POINT('Ctrl Pts',(-37.7740480458323,33.9057602738446,-9.62254085996342));
#32758=CARTESIAN_POINT('Ctrl Pts',(-38.798817306756,34.6299874229481,-9.6236915153538));
#32759=CARTESIAN_POINT('Ctrl Pts',(-31.2747661069637,31.8324214200722,1.24768201173568));
#32760=CARTESIAN_POINT('Ctrl Pts',(-31.2843061312616,31.7826622501022,0.76547938791503));
#32761=CARTESIAN_POINT('Ctrl Pts',(-31.2917666379332,31.734856231766,0.332966415938288));
#32762=CARTESIAN_POINT('Ctrl Pts',(-31.3978213276601,31.6085484626272,-0.978922014666463));
#32763=CARTESIAN_POINT('Ctrl Pts',(-31.6360823818443,31.6449008941949,-1.98636136655456));
#32764=CARTESIAN_POINT('Ctrl Pts',(-32.3637918611878,31.9494557448061,-3.81078790532199));
#32765=CARTESIAN_POINT('Ctrl Pts',(-32.8768818719989,32.2252577802497,-4.6546026491141));
#32766=CARTESIAN_POINT('Ctrl Pts',(-34.0936348201201,32.9506697646595,-6.05121512491815));
#32767=CARTESIAN_POINT('Ctrl Pts',(-34.8172613800643,33.4089026594542,-6.61423873289649));
#32768=CARTESIAN_POINT('Ctrl Pts',(-36.3546651861043,34.4150618219321,-7.37244739496743));
#32769=CARTESIAN_POINT('Ctrl Pts',(-37.2044809779672,34.9808875866207,-7.56862230164793));
#32770=CARTESIAN_POINT('Ctrl Pts',(-38.0218131772948,35.5267289204026,-7.57037421506));
#32771=CARTESIAN_POINT('Ctrl Pts',(-25.5825535213022,27.901724132258,1.59647090706392));
#32772=CARTESIAN_POINT('Ctrl Pts',(-25.5977646187839,27.8576356266619,1.15259179090154));
#32773=CARTESIAN_POINT('Ctrl Pts',(-25.6076988465242,27.8006101679571,0.635573104329545));
#32774=CARTESIAN_POINT('Ctrl Pts',(-25.7366398496131,27.6900511858226,-1.86858636179538));
#32775=CARTESIAN_POINT('Ctrl Pts',(-26.0667980818804,27.8867543207442,-3.71029995871436));
#32776=CARTESIAN_POINT('Ctrl Pts',(-27.1980083507482,28.8018888878555,-7.16936247492051));
#32777=CARTESIAN_POINT('Ctrl Pts',(-27.9765753733663,29.5148901762992,-8.73699595772989));
#32778=CARTESIAN_POINT('Ctrl Pts',(-29.8931745080091,31.3430252789184,-11.3730256981895));
#32779=CARTESIAN_POINT('Ctrl Pts',(-31.0108564712645,32.4473861125716,-12.4235805192514));
#32780=CARTESIAN_POINT('Ctrl Pts',(-33.470070913885,34.8951191226966,-13.8529470821305));
#32781=CARTESIAN_POINT('Ctrl Pts',(-34.7723177498354,36.2126515924125,-14.2204718557451));
#32782=CARTESIAN_POINT('Ctrl Pts',(-36.086449865815,37.5367254229123,-14.2198708430665));
#32783=CARTESIAN_POINT('Ctrl Pts',(-24.6306899881719,27.8942941678687,1.62964634867149));
#32784=CARTESIAN_POINT('Ctrl Pts',(-24.645774183387,27.8505734813085,1.18947040157924));
#32785=CARTESIAN_POINT('Ctrl Pts',(-24.6552631565805,27.7924691428847,0.664244065130957));
#32786=CARTESIAN_POINT('Ctrl Pts',(-24.7842103148136,27.6812026446449,-1.95287905128799));
#32787=CARTESIAN_POINT('Ctrl Pts',(-25.1246550797452,27.8909128870965,-3.87337387080019));
#32788=CARTESIAN_POINT('Ctrl Pts',(-26.2979391683636,28.8532656404492,-7.48792130212534));
#32789=CARTESIAN_POINT('Ctrl Pts',(-27.1064590436759,29.6017140578355,-9.12360836232651));
#32790=CARTESIAN_POINT('Ctrl Pts',(-29.1001001805409,31.5183666697857,-11.8774049927045));
#32791=CARTESIAN_POINT('Ctrl Pts',(-30.2623381500346,32.6750275472119,-12.9732563608965));
#32792=CARTESIAN_POINT('Ctrl Pts',(-32.8235411737415,35.2391241080399,-14.4676858045382));
#32793=CARTESIAN_POINT('Ctrl Pts',(-34.1773627942051,36.6172542487414,-14.8501851005579));
#32794=CARTESIAN_POINT('Ctrl Pts',(-35.5466255754748,38.0044776097606,-14.8499483202527));
#32795=CARTESIAN_POINT('Ctrl Pts',(-23.9110153591928,28.518207957172,1.6297555316112));
#32796=CARTESIAN_POINT('Ctrl Pts',(-23.9260975032013,28.4744932159134,1.18963944139604));
#32797=CARTESIAN_POINT('Ctrl Pts',(-23.9355515973827,28.4163403666075,0.664246507199459));
#32798=CARTESIAN_POINT('Ctrl Pts',(-24.0640354326714,28.3045391652296,-1.95288623097488));
#32799=CARTESIAN_POINT('Ctrl Pts',(-24.4051905243015,28.5150692335709,-3.87317034520081));
#32800=CARTESIAN_POINT('Ctrl Pts',(-25.5776818931472,29.4765070006193,-7.48823335802904));
#32801=CARTESIAN_POINT('Ctrl Pts',(-26.3866880328324,30.225516684584,-9.12349227712161));
#32802=CARTESIAN_POINT('Ctrl Pts',(-28.3801534903862,32.1419665195312,-11.8775764776477));
#32803=CARTESIAN_POINT('Ctrl Pts',(-29.5426791470118,33.2989594622607,-12.9726927515242));
#32804=CARTESIAN_POINT('Ctrl Pts',(-32.103561231544,35.8626855591394,-14.4683433355121));
#32805=CARTESIAN_POINT('Ctrl Pts',(-33.4576026588981,37.2410591163594,-14.8498038984863));
#32806=CARTESIAN_POINT('Ctrl Pts',(-34.8267964255889,38.6282131180508,-14.8500516281496));
#32807=CARTESIAN_POINT('Ctrl Pts',(-23.7833669488544,29.4615086055164,1.59674386441321));
#32808=CARTESIAN_POINT('Ctrl Pts',(-23.7985729183198,29.4174349631855,1.15301439044218));
#32809=CARTESIAN_POINT('Ctrl Pts',(-23.8084199485281,29.3602882272665,0.635579209500779));
#32810=CARTESIAN_POINT('Ctrl Pts',(-23.9362026442624,29.2483924872771,-1.86860431101262));
#32811=CARTESIAN_POINT('Ctrl Pts',(-24.2681366932807,29.4471451869314,-3.70979114471473));
#32812=CARTESIAN_POINT('Ctrl Pts',(-25.3973651626975,30.3599922882794,-7.17014261468097));
#32813=CARTESIAN_POINT('Ctrl Pts',(-26.1771478462482,31.0743967431656,-8.73670574471763));
#32814=CARTESIAN_POINT('Ctrl Pts',(-28.0933077826319,32.9020249032871,-11.3734544105476));
#32815=CARTESIAN_POINT('Ctrl Pts',(-29.2117089637015,34.0072159001959,-12.422171495823));
#32816=CARTESIAN_POINT('Ctrl Pts',(-31.6701210583974,36.4540227504429,-13.854590909563));
#32817=CARTESIAN_POINT('Ctrl Pts',(-32.972918011878,37.7721633453382,-14.2195188099105));
#32818=CARTESIAN_POINT('Ctrl Pts',(-34.2868769911003,39.0960641936379,-14.2201291128085));
#32819=CARTESIAN_POINT('Ctrl Pts',(-25.6404249706857,27.7725495286739,1.04083408558608E-14));
#32820=CARTESIAN_POINT('Ctrl Pts',(-25.7366398496132,27.6900511858226,-1.86858636179538));
#32821=CARTESIAN_POINT('Ctrl Pts',(-26.0667980818804,27.8867543207442,-3.71029995871436));
#32822=CARTESIAN_POINT('Ctrl Pts',(-27.1980083507482,28.8018888878555,-7.16936247492051));
#32823=CARTESIAN_POINT('Ctrl Pts',(-27.9765753733639,29.5148901762992,-8.7369959577275));
#32824=CARTESIAN_POINT('Ctrl Pts',(-29.03235780837,30.5219411006535,-10.1890856763466));
#32825=CARTESIAN_POINT('Ctrl Pts',(-29.1314899559286,30.616893617651,-10.320392863511));
#32826=CARTESIAN_POINT('Ctrl Pts',(-29.2322214279503,30.7137407645344,-10.448860376592));
#32827=CARTESIAN_POINT('Ctrl Pts',(-23.8408520862198,29.3318883095343,-8.88178419700125E-16));
#32828=CARTESIAN_POINT('Ctrl Pts',(-23.9362026442624,29.2483924872771,-1.86860431101262));
#32829=CARTESIAN_POINT('Ctrl Pts',(-24.2681366932807,29.4471451869314,-3.70979114471473));
#32830=CARTESIAN_POINT('Ctrl Pts',(-25.3973651626975,30.3599922882794,-7.17014261468097));
#32831=CARTESIAN_POINT('Ctrl Pts',(-26.1771478462482,31.0743967431656,-8.73670574471763));
#32832=CARTESIAN_POINT('Ctrl Pts',(-27.2380760953908,32.0863072351785,-10.1966053555756));
#32833=CARTESIAN_POINT('Ctrl Pts',(-27.3427718639926,32.1866090102528,-10.335023194234));
#32834=CARTESIAN_POINT('Ctrl Pts',(-27.4492538662495,32.2890256406149,-10.4702558451083));
#32835=CARTESIAN_POINT('Ctrl Pts',(-31.6397608122766,31.4394459897279,1.24689105568327));
#32836=CARTESIAN_POINT('Ctrl Pts',(-31.6563000607263,31.3915079136632,0.764254809546443));
#32837=CARTESIAN_POINT('Ctrl Pts',(-31.6707408106672,31.3456016608171,0.332948724825213));
#32838=CARTESIAN_POINT('Ctrl Pts',(-31.7970479454232,31.239546238828,-0.978870002754192));
#32839=CARTESIAN_POINT('Ctrl Pts',(-32.0225645221741,31.3034976581128,-1.98783577088618));
#32840=CARTESIAN_POINT('Ctrl Pts',(-32.7052670086903,31.7151448890596,-3.80852727283832));
#32841=CARTESIAN_POINT('Ctrl Pts',(-33.1703611269162,32.0570939851866,-4.65544360728939));
#32842=CARTESIAN_POINT('Ctrl Pts',(-34.2727650719352,32.9497533019061,-6.0499728333633));
#32843=CARTESIAN_POINT('Ctrl Pts',(-34.9217287193182,33.5038992564081,-6.61832169905306));
#32844=CARTESIAN_POINT('Ctrl Pts',(-36.3026175786583,34.7212963023931,-7.36768403076268));
#32845=CARTESIAN_POINT('Ctrl Pts',(-37.0616291372176,35.400569394778,-7.57138648706064));
#32846=CARTESIAN_POINT('Ctrl Pts',(-37.7934972961794,36.0576472036357,-7.56962581969389));
#32847=CARTESIAN_POINT('Ctrl Pts',(-29.4001542854016,30.6671178491337,1.35489343606325));
#32848=CARTESIAN_POINT('Ctrl Pts',(-29.4162823633,30.6203715276532,0.884255668134132));
#32849=CARTESIAN_POINT('Ctrl Pts',(-29.4293136556726,30.5710069006836,0.426397017784211));
#32850=CARTESIAN_POINT('Ctrl Pts',(-29.5561964051726,30.4632865154017,-1.25360819505145));
#32851=CARTESIAN_POINT('Ctrl Pts',(-29.814389573106,30.5686507749802,-2.51960912780314));
#32852=CARTESIAN_POINT('Ctrl Pts',(-30.6351795888044,31.1352998840684,-4.84647586781734));
#32853=CARTESIAN_POINT('Ctrl Pts',(-31.1973201148198,31.5921137089528,-5.91572199050937));
#32854=CARTESIAN_POINT('Ctrl Pts',(-32.551048345043,32.7735335074371,-7.69376028687725));
#32855=CARTESIAN_POINT('Ctrl Pts',(-33.3448945810382,33.4977500491683,-8.41063186559017));
#32856=CARTESIAN_POINT('Ctrl Pts',(-35.0585937299434,35.0948710911578,-9.37059840617546));
#32857=CARTESIAN_POINT('Ctrl Pts',(-35.9854803115198,35.9713447024496,-9.62435378640853));
#32858=CARTESIAN_POINT('Ctrl Pts',(-36.8970924436849,36.8343596268991,-9.62320046360515));
#32859=CARTESIAN_POINT('Ctrl Pts',(-27.3548849305453,29.4725749263795,1.47293214974066));
#32860=CARTESIAN_POINT('Ctrl Pts',(-27.3705645465822,29.4271284462505,1.01538106787189));
#32861=CARTESIAN_POINT('Ctrl Pts',(-27.3820741720672,29.3740093215552,0.52858080309974));
#32862=CARTESIAN_POINT('Ctrl Pts',(-27.5098462703896,29.2647682695534,-1.55402875460085));
#32863=CARTESIAN_POINT('Ctrl Pts',(-27.8033726143254,29.4149573143428,-3.10121432124709));
#32864=CARTESIAN_POINT('Ctrl Pts',(-28.7756052303118,30.1516133539741,-5.98129145449675));
#32865=CARTESIAN_POINT('Ctrl Pts',(-29.4435926415566,30.733716217446,-7.29389406578866));
#32866=CARTESIAN_POINT('Ctrl Pts',(-31.0722410437714,32.2310076487118,-9.49113593801764));
#32867=CARTESIAN_POINT('Ctrl Pts',(-32.0243541445899,33.1410090871553,-10.370828601741));
#32868=CARTESIAN_POINT('Ctrl Pts',(-34.1021594176632,35.1535638963511,-11.5604045561007));
#32869=CARTESIAN_POINT('Ctrl Pts',(-35.212471437781,36.2455537133643,-11.869476154252));
#32870=CARTESIAN_POINT('Ctrl Pts',(-36.3206928540897,37.3337834058788,-11.868714228481));
#32871=CARTESIAN_POINT('Ctrl Pts',(-25.5825535213022,27.901724132258,1.59647090706392));
#32872=CARTESIAN_POINT('Ctrl Pts',(-25.5977646187839,27.8576356266619,1.15259179090154));
#32873=CARTESIAN_POINT('Ctrl Pts',(-25.6076988465242,27.8006101679571,0.635573104329545));
#32874=CARTESIAN_POINT('Ctrl Pts',(-25.7366398496132,27.6900511858226,-1.86858636179538));
#32875=CARTESIAN_POINT('Ctrl Pts',(-26.0667980818804,27.8867543207442,-3.71029995871436));
#32876=CARTESIAN_POINT('Ctrl Pts',(-27.1980083507482,28.8018888878555,-7.16936247492051));
#32877=CARTESIAN_POINT('Ctrl Pts',(-27.9765753733639,29.5148901762992,-8.7369959577275));
#32878=CARTESIAN_POINT('Ctrl Pts',(-29.8931745080115,31.3430252789184,-11.3730256981919));
#32879=CARTESIAN_POINT('Ctrl Pts',(-31.0108564712693,32.4473861125668,-12.4235805192514));
#32880=CARTESIAN_POINT('Ctrl Pts',(-33.4700709138802,34.8951191227014,-13.8529470821305));
#32881=CARTESIAN_POINT('Ctrl Pts',(-34.7723177498282,36.2126515924196,-14.2204718557498));
#32882=CARTESIAN_POINT('Ctrl Pts',(-36.086449865815,37.5367254229123,-14.2198708430665));
#32883=CARTESIAN_POINT('Ctrl Pts',(-23.7833669488544,29.4615086055164,1.59674386441321));
#32884=CARTESIAN_POINT('Ctrl Pts',(-23.7985729183197,29.4174349631855,1.15301439044218));
#32885=CARTESIAN_POINT('Ctrl Pts',(-23.8084199485281,29.3602882272665,0.635579209500779));
#32886=CARTESIAN_POINT('Ctrl Pts',(-23.9362026442624,29.2483924872771,-1.86860431101262));
#32887=CARTESIAN_POINT('Ctrl Pts',(-24.2681366932831,29.4471451869314,-3.70979114471473));
#32888=CARTESIAN_POINT('Ctrl Pts',(-25.3973651626951,30.3599922882794,-7.17014261468097));
#32889=CARTESIAN_POINT('Ctrl Pts',(-26.1771478462457,31.0743967431704,-8.73670574471765));
#32890=CARTESIAN_POINT('Ctrl Pts',(-28.0933077826343,32.9020249032823,-11.3734544105476));
#32891=CARTESIAN_POINT('Ctrl Pts',(-29.2117089636991,34.0072159001958,-12.4221714958182));
#32892=CARTESIAN_POINT('Ctrl Pts',(-31.6701210583998,36.4540227504429,-13.8545909095678));
#32893=CARTESIAN_POINT('Ctrl Pts',(-32.972918011877,37.7721633453374,-14.2195188099153));
#32894=CARTESIAN_POINT('Ctrl Pts',(-34.2868769911003,39.0960641936379,-14.2201291128086));
#32895=CARTESIAN_POINT('Ctrl Pts',(-25.0869579521468,31.4387285991345,1.47327622041453));
#32896=CARTESIAN_POINT('Ctrl Pts',(-25.1026311041719,31.3933008545835,1.0159137668782));
#32897=CARTESIAN_POINT('Ctrl Pts',(-25.1140308146307,31.3400288564346,0.528588498845575));
#32898=CARTESIAN_POINT('Ctrl Pts',(-25.2403428328608,31.2291027822935,-1.55405138011097));
#32899=CARTESIAN_POINT('Ctrl Pts',(-25.536107645434,31.3818753630146,-3.10057294640638));
#32900=CARTESIAN_POINT('Ctrl Pts',(-26.5058421456017,32.1156479855494,-5.98227484334664));
#32901=CARTESIAN_POINT('Ctrl Pts',(-27.1753619327859,32.6995195811097,-7.29352824385025));
#32902=CARTESIAN_POINT('Ctrl Pts',(-28.8034567128381,34.1961719966305,-9.49167634240776));
#32903=CARTESIAN_POINT('Ctrl Pts',(-29.7564764086048,35.1072198799865,-10.3690524867446));
#32904=CARTESIAN_POINT('Ctrl Pts',(-31.8332702988131,37.1186072377306,-11.5624766483702));
#32905=CARTESIAN_POINT('Ctrl Pts',(-32.9442792642516,38.2113611019873,-11.8682745704738));
#32906=CARTESIAN_POINT('Ctrl Pts',(-34.0522789304537,39.2993752576343,-11.869039784999));
#32907=CARTESIAN_POINT('Ctrl Pts',(-25.9793365537798,33.6327571359871,1.35541241355826));
#32908=CARTESIAN_POINT('Ctrl Pts',(-25.9954548817196,33.5860390742308,0.885059162349419));
#32909=CARTESIAN_POINT('Ctrl Pts',(-26.0083203842389,33.5364438612578,0.426408625628756));
#32910=CARTESIAN_POINT('Ctrl Pts',(-26.1330008283201,33.4261818802138,-1.25364232214062));
#32911=CARTESIAN_POINT('Ctrl Pts',(-26.3945703806265,33.5354430048991,-2.51864171287205));
#32912=CARTESIAN_POINT('Ctrl Pts',(-27.2115923742643,34.0977429244363,-4.84795915808225));
#32913=CARTESIAN_POINT('Ctrl Pts',(-27.7760442528266,34.5572246086334,-5.91517020458963));
#32914=CARTESIAN_POINT('Ctrl Pts',(-29.1289374294719,35.7376805504921,-7.69457540347394));
#32915=CARTESIAN_POINT('Ctrl Pts',(-29.9241511239976,36.4634754928399,-8.40795287031606));
#32916=CARTESIAN_POINT('Ctrl Pts',(-31.6363247579804,38.0588356145396,-9.37372383747396));
#32917=CARTESIAN_POINT('Ctrl Pts',(-32.5642699125256,38.9364560608696,-9.62254085990179));
#32918=CARTESIAN_POINT('Ctrl Pts',(-33.4755402303454,39.7991514935069,-9.62369151535411));
#32919=CARTESIAN_POINT('Ctrl Pts',(-26.4262081762393,35.9592765491247,1.24768201173514));
#32920=CARTESIAN_POINT('Ctrl Pts',(-26.4427325651026,35.9113815427634,0.765479387909697));
#32921=CARTESIAN_POINT('Ctrl Pts',(-26.4569206403356,35.8651238615744,0.332966415948582));
#32922=CARTESIAN_POINT('Ctrl Pts',(-26.5798713158797,35.7551948794183,-0.978922014696859));
#32923=CARTESIAN_POINT('Ctrl Pts',(-26.8105337258744,35.8250853790548,-1.98636136650463));
#32924=CARTESIAN_POINT('Ctrl Pts',(-27.4874934973876,36.2301041572591,-3.81078790537277));
#32925=CARTESIAN_POINT('Ctrl Pts',(-27.9561102698756,36.5761192475661,-4.65460264902373));
#32926=CARTESIAN_POINT('Ctrl Pts',(-29.0572415379625,37.4673095829807,-6.05121512500961));
#32927=CARTESIAN_POINT('Ctrl Pts',(-29.7082892826565,38.0238611245015,-6.61423873294022));
#32928=CARTESIAN_POINT('Ctrl Pts',(-31.0868531562901,39.2385744114085,-7.37244739492485));
#32929=CARTESIAN_POINT('Ctrl Pts',(-31.8474936465763,39.9195822825963,-7.56862230155307));
#32930=CARTESIAN_POINT('Ctrl Pts',(-32.5788252613913,40.5761862384901,-7.57037421506044));
#32931=CARTESIAN_POINT('Ctrl Pts',(-21.3513306581892,31.2585017743465,1.59647086199749));
#32932=CARTESIAN_POINT('Ctrl Pts',(-21.372661376489,31.2170267923784,1.15259176011709));
#32933=CARTESIAN_POINT('Ctrl Pts',(-21.390610056738,31.1619955607677,0.635573083859853));
#32934=CARTESIAN_POINT('Ctrl Pts',(-21.5339728088269,31.0709121284019,-1.86858636174266));
#32935=CARTESIAN_POINT('Ctrl Pts',(-21.8327767314457,31.3125995244709,-3.7102999587274));
#32936=CARTESIAN_POINT('Ctrl Pts',(-22.822235683043,32.3794073476566,-7.16936247490758));
#32937=CARTESIAN_POINT('Ctrl Pts',(-23.4914073530992,33.1959529508684,-8.73699595766537));
#32938=CARTESIAN_POINT('Ctrl Pts',(-25.1283275201135,35.2782407701667,-11.3730256982543));
#32939=CARTESIAN_POINT('Ctrl Pts',(-26.0774661594562,36.5304235305538,-12.4235805192081));
#32940=CARTESIAN_POINT('Ctrl Pts',(-28.1633006172565,39.303224853823,-13.8529470821741));
#32941=CARTESIAN_POINT('Ctrl Pts',(-29.2647880382077,40.7926757902301,-14.2204718556168));
#32942=CARTESIAN_POINT('Ctrl Pts',(-30.377108830674,42.2902929581066,-14.2198708430667));
#32943=CARTESIAN_POINT('Ctrl Pts',(-20.4102131175328,31.1156831315057,1.62964630360509));
#32944=CARTESIAN_POINT('Ctrl Pts',(-20.4313658791504,31.0745541646192,1.18947037066851));
#32945=CARTESIAN_POINT('Ctrl Pts',(-20.4490273774855,31.0183916684046,0.664244043741713));
#32946=CARTESIAN_POINT('Ctrl Pts',(-20.592496912111,30.9266087974082,-1.95287905124417));
#32947=CARTESIAN_POINT('Ctrl Pts',(-20.8996315609143,31.1826348336499,-3.87337387081084));
#32948=CARTESIAN_POINT('Ctrl Pts',(-21.9240162329082,32.3021679588473,-7.48792130211473));
#32949=CARTESIAN_POINT('Ctrl Pts',(-22.6177912263983,33.1580626256957,-9.12360836229304));
#32950=CARTESIAN_POINT('Ctrl Pts',(-24.3183718640796,35.33893119389,-11.8774049927381));
#32951=CARTESIAN_POINT('Ctrl Pts',(-25.3041699215151,36.6492226397706,-12.9732563608771));
#32952=CARTESIAN_POINT('Ctrl Pts',(-27.4743946037862,39.5517175890428,-14.4676858045577));
#32953=CARTESIAN_POINT('Ctrl Pts',(-28.6183079046236,41.1084892565677,-14.8501851004866));
#32954=CARTESIAN_POINT('Ctrl Pts',(-29.7762110964237,42.67645909556,-14.8499483202528));
#32955=CARTESIAN_POINT('Ctrl Pts',(-19.6090715485703,31.6308259996108,1.62975548654486));
#32956=CARTESIAN_POINT('Ctrl Pts',(-19.6302214337532,31.5897026256002,1.18963941047576));
#32957=CARTESIAN_POINT('Ctrl Pts',(-19.6478553119118,31.5334871484633,0.664246485816154));
#32958=CARTESIAN_POINT('Ctrl Pts',(-19.7909423357445,31.4411090791072,-1.95288623094877));
#32959=CARTESIAN_POINT('Ctrl Pts',(-20.0986634077675,31.6980476866425,-3.87317034520541));
#32960=CARTESIAN_POINT('Ctrl Pts',(-21.12239364484,32.8165623229556,-7.48823335802438));
#32961=CARTESIAN_POINT('Ctrl Pts',(-21.816570076654,33.6730817461045,-9.12349227713351));
#32962=CARTESIAN_POINT('Ctrl Pts',(-23.5170056814165,35.8537245995938,-11.8775764776358));
#32963=CARTESIAN_POINT('Ctrl Pts',(-24.5030412398847,37.1643856729197,-12.9726927515334));
#32964=CARTESIAN_POINT('Ctrl Pts',(-26.6730009722203,40.0664682546505,-14.4683433355028));
#32965=CARTESIAN_POINT('Ctrl Pts',(-27.8170972008357,41.6235121428184,-14.849803898548));
#32966=CARTESIAN_POINT('Ctrl Pts',(-28.9749419513881,43.1914035066778,-14.8500516281495));
#32967=CARTESIAN_POINT('Ctrl Pts',(-19.3484767357831,32.5463589446091,1.59674381934693));
#32968=CARTESIAN_POINT('Ctrl Pts',(-19.3698002629981,32.5048979448427,1.15301435963395));
#32969=CARTESIAN_POINT('Ctrl Pts',(-19.3876798928005,32.4497342609156,0.635579189045957));
#32970=CARTESIAN_POINT('Ctrl Pts',(-19.5300863679201,32.3571628326458,-1.86860431100416));
#32971=CARTESIAN_POINT('Ctrl Pts',(-19.8303563485812,32.6011316569382,-3.70979114471325));
#32972=CARTESIAN_POINT('Ctrl Pts',(-20.8181792128701,33.6653932579417,-7.1701426146823));
#32973=CARTESIAN_POINT('Ctrl Pts',(-21.4883544787337,34.4835007519095,-8.73670574476775));
#32974=CARTESIAN_POINT('Ctrl Pts',(-23.1249120634605,36.565224284407,-11.3734544104973));
#32975=CARTESIAN_POINT('Ctrl Pts',(-24.074644455379,37.8183311134267,-12.4221714958561));
#32976=CARTESIAN_POINT('Ctrl Pts',(-26.1598165383431,40.5901015178423,-13.8545909095296));
#32977=CARTESIAN_POINT('Ctrl Pts',(-27.261761932141,42.0802326794198,-14.2195188100388));
#32978=CARTESIAN_POINT('Ctrl Pts',(-28.373935968085,43.577653985901,-14.2201291128083));
#32979=CARTESIAN_POINT('Ctrl Pts',(-21.4269965203139,31.138877952143,0.));
#32980=CARTESIAN_POINT('Ctrl Pts',(-21.5339728088269,31.0709121284019,-1.86858636174266));
#32981=CARTESIAN_POINT('Ctrl Pts',(-21.8327767314481,31.3125995244709,-3.7102999587262));
#32982=CARTESIAN_POINT('Ctrl Pts',(-22.8222356830406,32.3794073476566,-7.16936247490878));
#32983=CARTESIAN_POINT('Ctrl Pts',(-23.4914073530968,33.1959529508732,-8.73699595766537));
#32984=CARTESIAN_POINT('Ctrl Pts',(-24.3931251555334,34.3430070554536,-10.1890856763534));
#32985=CARTESIAN_POINT('Ctrl Pts',(-24.4777351286485,34.4511010682924,-10.3203928635226));
#32986=CARTESIAN_POINT('Ctrl Pts',(-24.5636585134689,34.561298034017,-10.4488603766072));
#32987=CARTESIAN_POINT('Ctrl Pts',(-19.4238236466307,32.4262389885814,1.66533453693773E-15));
#32988=CARTESIAN_POINT('Ctrl Pts',(-19.5300863679201,32.3571628326458,-1.86860431100416));
#32989=CARTESIAN_POINT('Ctrl Pts',(-19.8303563485812,32.6011316569382,-3.70979114471325));
#32990=CARTESIAN_POINT('Ctrl Pts',(-20.8181792128701,33.6653932579417,-7.1701426146823));
#32991=CARTESIAN_POINT('Ctrl Pts',(-21.4883544787337,34.4835007519095,-8.73670574476775));
#32992=CARTESIAN_POINT('Ctrl Pts',(-22.3944741298215,35.6360972865697,-10.1966053555694));
#32993=CARTESIAN_POINT('Ctrl Pts',(-22.4838298155454,35.7502778955871,-10.3350231942233));
#32994=CARTESIAN_POINT('Ctrl Pts',(-22.5746525783571,35.8668060412641,-10.4702558450944));
#32995=CARTESIAN_POINT('Ctrl Pts',(-26.8434139987113,35.6222452002841,1.24689101061693));
#32996=CARTESIAN_POINT('Ctrl Pts',(-26.8666072002651,35.5771488466243,0.764254780049933));
#32997=CARTESIAN_POINT('Ctrl Pts',(-26.8874341048571,35.5337649882881,0.332948714094922));
#32998=CARTESIAN_POINT('Ctrl Pts',(-27.0275488741897,35.4467644377494,-0.978870002705638));
#32999=CARTESIAN_POINT('Ctrl Pts',(-27.2416687814551,35.5421592788662,-1.98783577089888));
#33000=CARTESIAN_POINT('Ctrl Pts',(-27.8588388319486,36.0467752286497,-3.808527272826));
#33001=CARTESIAN_POINT('Ctrl Pts',(-28.2705345322819,36.4514335704433,-4.65544360715088));
#33002=CARTESIAN_POINT('Ctrl Pts',(-29.2346789285044,37.491895341034,-6.04997283350233));
#33003=CARTESIAN_POINT('Ctrl Pts',(-29.7981738696684,38.1327580456143,-6.61832169894778));
#33004=CARTESIAN_POINT('Ctrl Pts',(-30.991753607908,39.5342847195234,-7.36768403086871));
#33005=CARTESIAN_POINT('Ctrl Pts',(-31.6463688825656,40.3146623988252,-7.57138648666127));
#33006=CARTESIAN_POINT('Ctrl Pts',(-32.2772757571273,41.069207801424,-7.56962581969451));
#33007=CARTESIAN_POINT('Ctrl Pts',(-24.7365171914565,34.5390490058877,1.35489339099691));
#33008=CARTESIAN_POINT('Ctrl Pts',(-24.7591338032395,34.4950737607633,0.884255638235833));
#33009=CARTESIAN_POINT('Ctrl Pts',(-24.7790577744533,34.4480661428601,0.426397004049554));
#33010=CARTESIAN_POINT('Ctrl Pts',(-24.9199792485702,34.3594994944943,-1.25360819501069));
#33011=CARTESIAN_POINT('Ctrl Pts',(-25.1605494847682,34.5005360167157,-2.51960912781112));
#33012=CARTESIAN_POINT('Ctrl Pts',(-25.8923424652897,35.1782280533404,-4.8464758678096));
#33013=CARTESIAN_POINT('Ctrl Pts',(-26.3837498256845,35.7103931102928,-5.91572199041384));
#33014=CARTESIAN_POINT('Ctrl Pts',(-27.555565486858,37.0724433725846,-7.69376028697315));
#33015=CARTESIAN_POINT('Ctrl Pts',(-28.2382647527903,37.9022645330053,-8.41063186551349));
#33016=CARTESIAN_POINT('Ctrl Pts',(-29.7072268925448,39.7270140028106,-9.37059840625263));
#33017=CARTESIAN_POINT('Ctrl Pts',(-30.4999439048329,40.7264760905819,-9.62435378612815));
#33018=CARTESIAN_POINT('Ctrl Pts',(-31.2794573106202,41.7104427005355,-9.62320046360557));
#33019=CARTESIAN_POINT('Ctrl Pts',(-22.8820669124602,33.0655926302368,1.47293210467429));
#33020=CARTESIAN_POINT('Ctrl Pts',(-22.9040546403785,33.0228401731316,1.01538103753903));
#33021=CARTESIAN_POINT('Ctrl Pts',(-22.9230067538105,32.9718997171349,0.52858078607649));
#33022=CARTESIAN_POINT('Ctrl Pts',(-23.0650249378946,32.8819544477773,-1.55402875455868));
#33023=CARTESIAN_POINT('Ctrl Pts',(-23.3341894772259,33.0723879387897,-3.10121432125518));
#33024=CARTESIAN_POINT('Ctrl Pts',(-24.1916890819461,33.9399090096535,-5.9812914544888));
#33025=CARTESIAN_POINT('Ctrl Pts',(-24.7700354697141,34.6111514256874,-7.29389406572176));
#33026=CARTESIAN_POINT('Ctrl Pts',(-26.1690197913893,36.3249834230483,-9.49113593808477));
#33027=CARTESIAN_POINT('Ctrl Pts',(-26.981935046293,37.3612221809014,-10.370828601693));
#33028=CARTESIAN_POINT('Ctrl Pts',(-28.7521748453643,39.6489946054638,-11.5604045561491));
#33029=CARTESIAN_POINT('Ctrl Pts',(-29.6957791360119,40.8878834161158,-11.8694761540572));
#33030=CARTESIAN_POINT('Ctrl Pts',(-30.6378492234119,42.122752851181,-11.8687142284813));
#33031=CARTESIAN_POINT('Ctrl Pts',(-21.3513306581892,31.2585017743465,1.59647086199749));
#33032=CARTESIAN_POINT('Ctrl Pts',(-21.372661376489,31.2170267923722,1.15259176011769));
#33033=CARTESIAN_POINT('Ctrl Pts',(-21.390610056738,31.1619955607677,0.635573083859853));
#33034=CARTESIAN_POINT('Ctrl Pts',(-21.5339728088269,31.0709121284019,-1.86858636174266));
#33035=CARTESIAN_POINT('Ctrl Pts',(-21.8327767314481,31.3125995244709,-3.7102999587262));
#33036=CARTESIAN_POINT('Ctrl Pts',(-22.8222356830406,32.3794073476566,-7.16936247490878));
#33037=CARTESIAN_POINT('Ctrl Pts',(-23.4914073530968,33.1959529508732,-8.73699595766537));
#33038=CARTESIAN_POINT('Ctrl Pts',(-25.1283275201159,35.2782407701619,-11.3730256982543));
#33039=CARTESIAN_POINT('Ctrl Pts',(-26.0774661594586,36.5304235305538,-12.4235805192081));
#33040=CARTESIAN_POINT('Ctrl Pts',(-28.1633006172541,39.303224853823,-13.8529470821741));
#33041=CARTESIAN_POINT('Ctrl Pts',(-29.2647880381977,40.7926757902389,-14.2204718556121));
#33042=CARTESIAN_POINT('Ctrl Pts',(-30.377108830674,42.2902929581066,-14.2198708430667));
#33043=CARTESIAN_POINT('Ctrl Pts',(-19.3484767357831,32.5463589446091,1.59674381934693));
#33044=CARTESIAN_POINT('Ctrl Pts',(-19.3698002629981,32.5048979448426,1.15301435963396));
#33045=CARTESIAN_POINT('Ctrl Pts',(-19.3876798928005,32.4497342609156,0.635579189045957));
#33046=CARTESIAN_POINT('Ctrl Pts',(-19.5300863679201,32.3571628326458,-1.86860431100416));
#33047=CARTESIAN_POINT('Ctrl Pts',(-19.8303563485812,32.6011316569382,-3.70979114471445));
#33048=CARTESIAN_POINT('Ctrl Pts',(-20.8181792128701,33.6653932579417,-7.1701426146811));
#33049=CARTESIAN_POINT('Ctrl Pts',(-21.488354478736,34.4835007519095,-8.73670574476536));
#33050=CARTESIAN_POINT('Ctrl Pts',(-23.1249120634581,36.565224284407,-11.3734544104997));
#33051=CARTESIAN_POINT('Ctrl Pts',(-24.0746444553814,37.8183311134315,-12.4221714958561));
#33052=CARTESIAN_POINT('Ctrl Pts',(-26.1598165383407,40.5901015178374,-13.8545909095296));
#33053=CARTESIAN_POINT('Ctrl Pts',(-27.2617619321434,42.080232679423,-14.2195188100388));
#33054=CARTESIAN_POINT('Ctrl Pts',(-28.373935968085,43.577653985901,-14.2201291128083));
#33055=CARTESIAN_POINT('Ctrl Pts',(-20.3574113186624,34.6889740324161,1.47327617534834));
#33056=CARTESIAN_POINT('Ctrl Pts',(-20.3793899820084,34.6462392002826,1.01591373651538));
#33057=CARTESIAN_POINT('Ctrl Pts',(-20.398255055348,34.5951317842909,0.528588481841054));
#33058=CARTESIAN_POINT('Ctrl Pts',(-20.5390678245047,34.503310852838,-1.5540513801246));
#33059=CARTESIAN_POINT('Ctrl Pts',(-20.8100803726225,34.6966201504605,-3.10057294639873));
#33060=CARTESIAN_POINT('Ctrl Pts',(-21.6655176417304,35.5609316342214,-5.98227484335412));
#33061=CARTESIAN_POINT('Ctrl Pts',(-22.2451290911896,36.2341428589745,-7.29352824392187));
#33062=CARTESIAN_POINT('Ctrl Pts',(-23.6436563673474,37.9472635564085,-9.4916763423359));
#33063=CARTESIAN_POINT('Ctrl Pts',(-24.457320064637,38.984667129655,-10.3690524867921));
#33064=CARTESIAN_POINT('Ctrl Pts',(-26.2267249209685,41.2711400510057,-11.5624766483223));
#33065=CARTESIAN_POINT('Ctrl Pts',(-27.1709103277424,42.5108843176131,-11.8682745706401));
#33066=CARTESIAN_POINT('Ctrl Pts',(-28.1127915962418,43.7455088513559,-11.8690397849987));
#33067=CARTESIAN_POINT('Ctrl Pts',(-20.9284639764452,36.9876692386614,1.3554123684922));
#33068=CARTESIAN_POINT('Ctrl Pts',(-20.9510669157184,36.9437205780771,0.885059132406026));
#33069=CARTESIAN_POINT('Ctrl Pts',(-20.9708596003901,36.8964611268051,0.426408611922349));
#33070=CARTESIAN_POINT('Ctrl Pts',(-21.1099628921831,36.8050653317268,-1.25364232218402));
#33071=CARTESIAN_POINT('Ctrl Pts',(-21.3533205643391,36.9504395642519,-2.51864171285581));
#33072=CARTESIAN_POINT('Ctrl Pts',(-22.0820028299708,37.623290434238,-4.84795915809824));
#33073=CARTESIAN_POINT('Ctrl Pts',(-22.5753183406328,38.1584251351963,-5.91517020471142));
#33074=CARTESIAN_POINT('Ctrl Pts',(-23.7464446191913,39.5194025113534,-7.69457540335175));
#33075=CARTESIAN_POINT('Ctrl Pts',(-24.4302727949248,40.350980615974,-8.40795287038753));
#33076=CARTESIAN_POINT('Ctrl Pts',(-25.897975552453,42.173769985802,-9.37372383740198));
#33077=CARTESIAN_POINT('Ctrl Pts',(-26.691577151263,43.1745178860428,-9.62254086016785));
#33078=CARTESIAN_POINT('Ctrl Pts',(-27.4707976903313,44.158119610933,-9.6236915153537));
#33079=CARTESIAN_POINT('Ctrl Pts',(-21.0396888561033,39.3541045014165,1.24768196666922));
#33080=CARTESIAN_POINT('Ctrl Pts',(-21.0628612198437,39.3090486643518,0.765479358346324));
#33081=CARTESIAN_POINT('Ctrl Pts',(-21.0834880350599,39.2652809952961,0.332966405261353));
#33082=CARTESIAN_POINT('Ctrl Pts',(-21.2208317741903,39.1739686379191,-0.978922014776562));
#33083=CARTESIAN_POINT('Ctrl Pts',(-21.4391999183494,39.2759744366273,-1.9863613664762));
#33084=CARTESIAN_POINT('Ctrl Pts',(-22.0516290334592,39.773212128048,-3.81078790540083));
#33085=CARTESIAN_POINT('Ctrl Pts',(-22.4662328810889,40.1823964038332,-4.65460264921481));
#33086=CARTESIAN_POINT('Ctrl Pts',(-23.4293266125922,41.2212230249772,-6.05121512481796));
#33087=CARTESIAN_POINT('Ctrl Pts',(-23.9945420870012,41.8647634287767,-6.61423873305477));
#33088=CARTESIAN_POINT('Ctrl Pts',(-25.186202443381,43.2633027806102,-7.37244739480955));
#33089=CARTESIAN_POINT('Ctrl Pts',(-25.8421831847333,44.0456294021717,-7.56862230197604));
#33090=CARTESIAN_POINT('Ctrl Pts',(-26.4726264127402,44.7996294168197,-7.57037421505982));
#33091=CARTESIAN_POINT('Ctrl Pts',(-16.6854562787122,33.9789464595043,1.59647077610273));
#33092=CARTESIAN_POINT('Ctrl Pts',(-16.712472384757,33.9409293131097,1.1525917014065));
#33093=CARTESIAN_POINT('Ctrl Pts',(-16.7380701330052,33.8890125875519,0.635573044895123));
#33094=CARTESIAN_POINT('Ctrl Pts',(-16.8929361804277,33.8192589011608,-1.86858636178875));
#33095=CARTESIAN_POINT('Ctrl Pts',(-17.1543030074508,34.1010104999321,-3.71029995868829));
#33096=CARTESIAN_POINT('Ctrl Pts',(-17.9818681105611,35.297774448387,-7.16936247494685));
#33097=CARTESIAN_POINT('Ctrl Pts',(-18.5280220225195,36.2012418527131,-8.73699595767482));
#33098=CARTESIAN_POINT('Ctrl Pts',(-19.8519402482494,38.4952930132476,-11.373025698245));
#33099=CARTESIAN_POINT('Ctrl Pts',(-20.6132138376804,39.869806870641,-12.4235805192421));
#33100=CARTESIAN_POINT('Ctrl Pts',(-22.2832067364767,42.9112302679216,-13.8529470821403));
#33101=CARTESIAN_POINT('Ctrl Pts',(-23.1615116341977,44.5422787457965,-14.2204718557263));
#33102=CARTESIAN_POINT('Ctrl Pts',(-24.0493774600889,46.1829520838076,-14.2198708430668));
#33103=CARTESIAN_POINT('Ctrl Pts',(-15.7742431696985,33.7036465139254,1.62964621771032));
#33104=CARTESIAN_POINT('Ctrl Pts',(-15.8010338873345,33.665946534781,1.18947031172183));
#33105=CARTESIAN_POINT('Ctrl Pts',(-15.8265083724999,33.6128691890196,0.664244003017828));
#33106=CARTESIAN_POINT('Ctrl Pts',(-15.9815796560506,33.5424383800423,-1.95287905128809));
#33107=CARTESIAN_POINT('Ctrl Pts',(-16.2491518132338,33.8395682582168,-3.87337387077528));
#33108=CARTESIAN_POINT('Ctrl Pts',(-17.1037835504226,35.0934912894296,-7.48792130215042));
#33109=CARTESIAN_POINT('Ctrl Pts',(-17.6686904038385,36.039408658621,-9.12360836229767));
#33110=CARTESIAN_POINT('Ctrl Pts',(-19.041591625096,38.4400969877808,-11.8774049927335));
#33111=CARTESIAN_POINT('Ctrl Pts',(-19.8308817644157,39.8773452471795,-12.9732563608919));
#33112=CARTESIAN_POINT('Ctrl Pts',(-21.5659485894875,43.059152157502,-14.467685804543));
#33113=CARTESIAN_POINT('Ctrl Pts',(-22.4766667937812,44.7628739707804,-14.8501851005342));
#33114=CARTESIAN_POINT('Ctrl Pts',(-23.399638826952,46.4796709429187,-14.8499483202528));
#33115=CARTESIAN_POINT('Ctrl Pts',(-14.9079435927953,34.0995316375869,1.62975540065009));
#33116=CARTESIAN_POINT('Ctrl Pts',(-14.9347306673254,34.0618367850384,1.18963935152333));
#33117=CARTESIAN_POINT('Ctrl Pts',(-14.9601853534107,34.0087030668416,0.664246445087989));
#33118=CARTESIAN_POINT('Ctrl Pts',(-15.1149627251549,33.9376286808331,-1.95288623098056));
#33119=CARTESIAN_POINT('Ctrl Pts',(-15.3829854641584,34.2357452983242,-3.87317034518422));
#33120=CARTESIAN_POINT('Ctrl Pts',(-16.2371143737293,35.4885670716582,-7.48823335804566));
#33121=CARTESIAN_POINT('Ctrl Pts',(-16.8023296672983,36.4351599686395,-9.12349227713333));
#33122=CARTESIAN_POINT('Ctrl Pts',(-18.1751194544272,38.8356042401957,-11.877576477636));
#33123=CARTESIAN_POINT('Ctrl Pts',(-18.9645920738869,40.2732521647051,-12.9726927515338));
#33124=CARTESIAN_POINT('Ctrl Pts',(-20.6994553318481,43.454613198461,-14.4683433355024));
#33125=CARTESIAN_POINT('Ctrl Pts',(-21.6103158609432,45.1586304949284,-14.8498038985005));
#33126=CARTESIAN_POINT('Ctrl Pts',(-22.5332412158902,46.8753414736307,-14.8500516281495));
#33127=CARTESIAN_POINT('Ctrl Pts',(-14.5197073364542,34.9686592686579,1.59674373345215));
#33128=CARTESIAN_POINT('Ctrl Pts',(-14.5467143347313,34.9306549387464,1.15301430091079));
#33129=CARTESIAN_POINT('Ctrl Pts',(-14.5722625852828,34.878597282106,0.63557915007054));
#33130=CARTESIAN_POINT('Ctrl Pts',(-14.7263938531874,34.8072346531401,-1.86860431101993));
#33131=CARTESIAN_POINT('Ctrl Pts',(-14.9888871347659,35.0914531002031,-3.70979114470526));
#33132=CARTESIAN_POINT('Ctrl Pts',(-15.8151951688241,36.2854639039562,-7.17014261469034));
#33133=CARTESIAN_POINT('Ctrl Pts',(-16.3621201811738,37.1906201277523,-8.73670574476277));
#33134=CARTESIAN_POINT('Ctrl Pts',(-17.6857598215725,39.484061144292,-11.3734544105023));
#33135=CARTESIAN_POINT('Ctrl Pts',(-18.4474896113593,40.8595741644359,-12.4221714958421));
#33136=CARTESIAN_POINT('Ctrl Pts',(-20.116973592377,43.8998828703382,-13.8545909095436));
#33137=CARTESIAN_POINT('Ctrl Pts',(-20.995634995311,45.5316698260284,-14.2195188099103));
#33138=CARTESIAN_POINT('Ctrl Pts',(-21.8833834324344,47.1721284105875,-14.2201291128083));
#33139=CARTESIAN_POINT('Ctrl Pts',(-16.7773762111441,33.8713086176153,0.));
#33140=CARTESIAN_POINT('Ctrl Pts',(-16.8929361804277,33.8192589011608,-1.86858636178876));
#33141=CARTESIAN_POINT('Ctrl Pts',(-17.1543030074532,34.1010104999321,-3.71029995868829));
#33142=CARTESIAN_POINT('Ctrl Pts',(-17.9818681105587,35.297774448387,-7.16936247494685));
#33143=CARTESIAN_POINT('Ctrl Pts',(-18.5280220225147,36.2012418527083,-8.73699595767244));
#33144=CARTESIAN_POINT('Ctrl Pts',(-19.2573188185175,37.4649484236461,-10.1890856763525));
#33145=CARTESIAN_POINT('Ctrl Pts',(-19.3256842021482,37.5839834499338,-10.3203928635213));
#33146=CARTESIAN_POINT('Ctrl Pts',(-19.3950503474463,37.7052869420536,-10.4488603766057));
#33147=CARTESIAN_POINT('Ctrl Pts',(-14.6113821712781,34.8604849513724,9.43689570931383E-16));
#33148=CARTESIAN_POINT('Ctrl Pts',(-14.7263938531874,34.8072346531401,-1.86860431101993));
#33149=CARTESIAN_POINT('Ctrl Pts',(-14.9888871347659,35.0914531002031,-3.70979114470526));
#33150=CARTESIAN_POINT('Ctrl Pts',(-15.8151951688241,36.2854639039562,-7.17014261469034));
#33151=CARTESIAN_POINT('Ctrl Pts',(-16.3621201811738,37.1906201277523,-8.73670574476277));
#33152=CARTESIAN_POINT('Ctrl Pts',(-17.0949852513166,38.4604391632025,-10.1966053555693));
#33153=CARTESIAN_POINT('Ctrl Pts',(-17.1671818300937,38.5861742182181,-10.3350231942229));
#33154=CARTESIAN_POINT('Ctrl Pts',(-17.2404964639283,38.7144417021938,-10.4702558450934));
#33155=CARTESIAN_POINT('Ctrl Pts',(-21.5006126898292,39.0798782217544,1.24689092472207));
#33156=CARTESIAN_POINT('Ctrl Pts',(-21.5299876965042,39.038541623221,0.764254723801767));
#33157=CARTESIAN_POINT('Ctrl Pts',(-21.556776778946,38.9985633313781,0.332948693675433));
#33158=CARTESIAN_POINT('Ctrl Pts',(-21.7078468489019,38.9323887326631,-0.978870002707473));
#33159=CARTESIAN_POINT('Ctrl Pts',(-21.9062112228192,39.0572850320212,-1.98783577087692));
#33160=CARTESIAN_POINT('Ctrl Pts',(-22.4452850348575,39.6445971747049,-3.80852727284806));
#33161=CARTESIAN_POINT('Ctrl Pts',(-22.795201380093,40.1037270851767,-4.65544360716526));
#33162=CARTESIAN_POINT('Ctrl Pts',(-23.6014590279082,41.270810509,-6.04997283348821));
#33163=CARTESIAN_POINT('Ctrl Pts',(-24.0680141309618,41.9853438466691,-6.61832169902486));
#33164=CARTESIAN_POINT('Ctrl Pts',(-25.0499869064454,43.5424691073633,-7.36768403079195));
#33165=CARTESIAN_POINT('Ctrl Pts',(-25.586879818633,44.4080651337966,-7.57138648700893));
#33166=CARTESIAN_POINT('Ctrl Pts',(-26.1039819636366,45.244717762191,-7.56962581969456));
#33167=CARTESIAN_POINT('Ctrl Pts',(-19.5693159454018,37.707864724394,1.35489330510207));
#33168=CARTESIAN_POINT('Ctrl Pts',(-19.597960680827,37.6675557657844,0.884255581224363));
#33169=CARTESIAN_POINT('Ctrl Pts',(-19.6243717351814,37.6238620982378,0.426396977901309));
#33170=CARTESIAN_POINT('Ctrl Pts',(-19.7764631777463,37.5562521484254,-1.25360819501997));
#33171=CARTESIAN_POINT('Ctrl Pts',(-19.9945131659748,37.7300898365971,-2.51960912778664));
#33172=CARTESIAN_POINT('Ctrl Pts',(-20.6224119165105,38.5050289449629,-4.84647586783417));
#33173=CARTESIAN_POINT('Ctrl Pts',(-21.0330824745244,39.1017118880494,-5.91572199042815));
#33174=CARTESIAN_POINT('Ctrl Pts',(-21.999130779075,40.6166651988924,-7.69376028695902));
#33175=CARTESIAN_POINT('Ctrl Pts',(-22.5567852866311,41.5351982120077,-8.41063186556661));
#33176=CARTESIAN_POINT('Ctrl Pts',(-23.7511065841576,43.5504294726618,-9.37059840619976));
#33177=CARTESIAN_POINT('Ctrl Pts',(-24.3935165950074,44.6525338708004,-9.62435378637091));
#33178=CARTESIAN_POINT('Ctrl Pts',(-25.0250626292173,45.7374214437731,-9.6232004636056));
#33179=CARTESIAN_POINT('Ctrl Pts',(-17.9434360021528,35.9854902185572,1.47293201877948));
#33180=CARTESIAN_POINT('Ctrl Pts',(-17.9712842340148,35.9463021021744,1.01538097969612));
#33181=CARTESIAN_POINT('Ctrl Pts',(-17.9972930238973,35.8985773174081,0.528580753666282));
#33182=CARTESIAN_POINT('Ctrl Pts',(-18.1506662116607,35.829758857152,-1.5540287545829));
#33183=CARTESIAN_POINT('Ctrl Pts',(-18.389989532706,36.0565601177328,-3.10121432122698));
#33184=CARTESIAN_POINT('Ctrl Pts',(-19.1152999068524,37.0372859924728,-5.98129145451712));
#33185=CARTESIAN_POINT('Ctrl Pts',(-19.5922318064713,37.7840034012291,-7.29389406572886));
#33186=CARTESIAN_POINT('Ctrl Pts',(-20.7330727613966,39.6794872874845,-9.49113593807784));
#33187=CARTESIAN_POINT('Ctrl Pts',(-21.3902415598656,40.8208685319662,-10.370828601727));
#33188=CARTESIAN_POINT('Ctrl Pts',(-22.8168789077026,43.3372861226137,-11.5604045561153));
#33189=CARTESIAN_POINT('Ctrl Pts',(-23.5745664064031,44.6978537235883,-11.869476154219));
#33190=CARTESIAN_POINT('Ctrl Pts',(-24.3313073348068,46.0542245204214,-11.8687142284813));
#33191=CARTESIAN_POINT('Ctrl Pts',(-16.6854562787122,33.9789464595043,1.59647077610273));
#33192=CARTESIAN_POINT('Ctrl Pts',(-16.712472384757,33.9409293131097,1.1525917014065));
#33193=CARTESIAN_POINT('Ctrl Pts',(-16.7380701330052,33.8890125875519,0.635573044895126));
#33194=CARTESIAN_POINT('Ctrl Pts',(-16.8929361804277,33.8192589011608,-1.86858636178876));
#33195=CARTESIAN_POINT('Ctrl Pts',(-17.1543030074532,34.1010104999321,-3.71029995868829));
#33196=CARTESIAN_POINT('Ctrl Pts',(-17.9818681105587,35.297774448387,-7.16936247494685));
#33197=CARTESIAN_POINT('Ctrl Pts',(-18.5280220225147,36.2012418527083,-8.73699595767244));
#33198=CARTESIAN_POINT('Ctrl Pts',(-19.8519402482542,38.4952930132523,-11.3730256982474));
#33199=CARTESIAN_POINT('Ctrl Pts',(-20.6132138376827,39.869806870641,-12.4235805192421));
#33200=CARTESIAN_POINT('Ctrl Pts',(-22.2832067364743,42.9112302679216,-13.8529470821403));
#33201=CARTESIAN_POINT('Ctrl Pts',(-23.1615116342073,44.5422787457923,-14.2204718557263));
#33202=CARTESIAN_POINT('Ctrl Pts',(-24.0493774600889,46.1829520838076,-14.2198708430668));
#33203=CARTESIAN_POINT('Ctrl Pts',(-14.5197073364542,34.9686592686579,1.59674373345215));
#33204=CARTESIAN_POINT('Ctrl Pts',(-14.5467143347313,34.9306549387464,1.15301430091079));
#33205=CARTESIAN_POINT('Ctrl Pts',(-14.5722625852828,34.878597282106,0.63557915007054));
#33206=CARTESIAN_POINT('Ctrl Pts',(-14.7263938531874,34.8072346531401,-1.86860431101993));
#33207=CARTESIAN_POINT('Ctrl Pts',(-14.9888871347659,35.0914531002031,-3.70979114470526));
#33208=CARTESIAN_POINT('Ctrl Pts',(-15.8151951688241,36.2854639039562,-7.17014261469035));
#33209=CARTESIAN_POINT('Ctrl Pts',(-16.3621201811738,37.1906201277523,-8.73670574476277));
#33210=CARTESIAN_POINT('Ctrl Pts',(-17.6857598215725,39.484061144292,-11.3734544105023));
#33211=CARTESIAN_POINT('Ctrl Pts',(-18.4474896113593,40.8595741644407,-12.4221714958421));
#33212=CARTESIAN_POINT('Ctrl Pts',(-20.116973592377,43.8998828703334,-13.8545909095436));
#33213=CARTESIAN_POINT('Ctrl Pts',(-20.9956349953185,45.531669826028,-14.2195188099103));
#33214=CARTESIAN_POINT('Ctrl Pts',(-21.8833834324344,47.1721284105875,-14.2201291128083));
#33215=CARTESIAN_POINT('Ctrl Pts',(-15.21344650034,37.2330519862577,1.47327608945353));
#33216=CARTESIAN_POINT('Ctrl Pts',(-15.2412832516021,37.193880025428,1.0159136786565));
#33217=CARTESIAN_POINT('Ctrl Pts',(-15.2672296481932,37.1459775929339,0.528588449417375));
#33218=CARTESIAN_POINT('Ctrl Pts',(-15.4196766250125,37.0751310137801,-1.55405138011061));
#33219=CARTESIAN_POINT('Ctrl Pts',(-15.6604198747701,37.3050418083574,-3.10057294640882));
#33220=CARTESIAN_POINT('Ctrl Pts',(-16.3841456768375,38.2822972641546,-5.982274843344));
#33221=CARTESIAN_POINT('Ctrl Pts',(-16.8620495709161,39.031143478966,-7.29352824391929));
#33222=CARTESIAN_POINT('Ctrl Pts',(-18.0025393609276,40.9258582609531,-9.49167634233843));
#33223=CARTESIAN_POINT('Ctrl Pts',(-18.6602832132086,42.0684989791507,-10.3690524867684));
#33224=CARTESIAN_POINT('Ctrl Pts',(-20.0862790553937,44.5835114688915,-11.5624766483459));
#33225=CARTESIAN_POINT('Ctrl Pts',(-20.84442001122,45.9450085199879,-11.8682745704831));
#33226=CARTESIAN_POINT('Ctrl Pts',(-21.6010088957269,47.3011100364939,-11.8690397849987));
#33227=CARTESIAN_POINT('Ctrl Pts',(-15.45154822894,39.5896190563862,1.35541228259734));
#33228=CARTESIAN_POINT('Ctrl Pts',(-15.4801756476489,39.5493344659328,0.885059075369853));
#33229=CARTESIAN_POINT('Ctrl Pts',(-15.5064925913597,39.5053728442132,0.426408585753786));
#33230=CARTESIAN_POINT('Ctrl Pts',(-15.6571869876978,39.4347037901454,-1.25364232213566));
#33231=CARTESIAN_POINT('Ctrl Pts',(-15.877378719186,39.6132317302961,-2.51864171288877));
#33232=CARTESIAN_POINT('Ctrl Pts',(-16.5028873873638,40.3829362474577,-4.84795915806517));
#33233=CARTESIAN_POINT('Ctrl Pts',(-16.915024048968,40.9828301658262,-5.91517020469925));
#33234=CARTESIAN_POINT('Ctrl Pts',(-17.8805426754533,42.4966234016211,-7.69457540336378));
#33235=CARTESIAN_POINT('Ctrl Pts',(-18.4390645629117,43.4170561363981,-8.40795287034454));
#33236=CARTESIAN_POINT('Ctrl Pts',(-19.6324182481966,45.430168019251,-9.3737238374448));
#33237=CARTESIAN_POINT('Ctrl Pts',(-20.2755208515746,46.533671031965,-9.62254085991564));
#33238=CARTESIAN_POINT('Ctrl Pts',(-20.9068289285808,47.618155754582,-9.6236915153537));
#33239=CARTESIAN_POINT('Ctrl Pts',(-15.2248621479928,41.9477963710448,1.24768188077433));
#33240=CARTESIAN_POINT('Ctrl Pts',(-15.2542107628449,41.9064969111878,0.765479302060699));
#33241=CARTESIAN_POINT('Ctrl Pts',(-15.2808564144377,41.8661102394573,0.332966384810895));
#33242=CARTESIAN_POINT('Ctrl Pts',(-15.4297972934795,41.7952733633823,-0.978922014690554));
#33243=CARTESIAN_POINT('Ctrl Pts',(-15.6314258258816,41.9273179171967,-1.98636136653799));
#33244=CARTESIAN_POINT('Ctrl Pts',(-16.1668569942086,42.506652196413,-3.81078790533882));
#33245=CARTESIAN_POINT('Ctrl Pts',(-16.5190077783543,42.970675845735,-4.65460264919543));
#33246=CARTESIAN_POINT('Ctrl Pts',(-17.3244581617424,44.135991238422,-6.05121512483706));
#33247=CARTESIAN_POINT('Ctrl Pts',(-17.7923352091806,44.8534198776255,-6.61423873298768));
#33248=CARTESIAN_POINT('Ctrl Pts',(-18.772833279554,46.4073150662864,-7.37244739487633));
#33249=CARTESIAN_POINT('Ctrl Pts',(-19.3108003965693,47.2750345238072,-7.56862230159521));
#33250=CARTESIAN_POINT('Ctrl Pts',(-19.827521231076,48.1110813316861,-7.5703742150598));
#33251=CARTESIAN_POINT('Ctrl Pts',(-11.6799141290248,36.0076777827441,1.5964706812662));
#33252=CARTESIAN_POINT('Ctrl Pts',(-11.7120656519288,35.9738923911233,1.15259163661472));
#33253=CARTESIAN_POINT('Ctrl Pts',(-11.7447913705091,35.92614704651,0.635573001832125));
#33254=CARTESIAN_POINT('Ctrl Pts',(-11.90800808671,35.8791430893682,-1.86858636171601));
#33255=CARTESIAN_POINT('Ctrl Pts',(-12.1266171429531,36.1952232408274,-3.71029995871332));
#33256=CARTESIAN_POINT('Ctrl Pts',(-12.7754415589707,37.4975806517049,-7.16936247492168));
#33257=CARTESIAN_POINT('Ctrl Pts',(-13.1874595939467,38.4695778661641,-8.73699595765301));
#33258=CARTESIAN_POINT('Ctrl Pts',(-14.1714247212182,40.9286921018696,-11.3730256982666));
#33259=CARTESIAN_POINT('Ctrl Pts',(-14.7293359258389,42.3975559177982,-12.4235805192321));
#33260=CARTESIAN_POINT('Ctrl Pts',(-15.9494910259352,45.6456867796067,-13.85294708215));
#33261=CARTESIAN_POINT('Ctrl Pts',(-16.586733645961,47.3851293551697,-14.2204718557119));
#33262=CARTESIAN_POINT('Ctrl Pts',(-17.2320701170944,49.135459485718,-14.2198708430666));
#33263=CARTESIAN_POINT('Ctrl Pts',(-10.8171551228317,35.6055008474196,1.62964612287377));
#33264=CARTESIAN_POINT('Ctrl Pts',(-10.8490384138683,35.5719973186131,1.18947024666915));
#33265=CARTESIAN_POINT('Ctrl Pts',(-10.881807297469,35.5230856250774,0.6642439580119));
#33266=CARTESIAN_POINT('Ctrl Pts',(-11.045323525379,35.4754406456305,-1.95287905121106));
#33267=CARTESIAN_POINT('Ctrl Pts',(-11.2678861931098,35.807625658362,-3.87337387079559));
#33268=CARTESIAN_POINT('Ctrl Pts',(-11.9353671583008,37.1704123385714,-7.48792130213002));
#33269=CARTESIAN_POINT('Ctrl Pts',(-12.3599059969334,38.1870962603156,-9.1236083622735));
#33270=CARTESIAN_POINT('Ctrl Pts',(-13.3771794920611,40.7587332590992,-11.8774049927576));
#33271=CARTESIAN_POINT('Ctrl Pts',(-13.9538940422131,42.2936801020572,-12.973256360882));
#33272=CARTESIAN_POINT('Ctrl Pts',(-15.2184820528883,45.690026560441,-14.4676858045528));
#33273=CARTESIAN_POINT('Ctrl Pts',(-15.8774655648087,47.5060156561272,-14.8501851005389));
#33274=CARTESIAN_POINT('Ctrl Pts',(-16.5467173899501,49.3366907261819,-14.8499483202528));
#33275=CARTESIAN_POINT('Ctrl Pts',(-9.90333289917187,35.8740691471581,1.62975530581353));
#33276=CARTESIAN_POINT('Ctrl Pts',(-9.9352118545932,35.8405701742916,1.18963928646021));
#33277=CARTESIAN_POINT('Ctrl Pts',(-9.967969163272,35.7915998644065,0.664246400084043));
#33278=CARTESIAN_POINT('Ctrl Pts',(-10.1312860615336,35.7432760306003,-1.95288623090985));
#33279=CARTESIAN_POINT('Ctrl Pts',(-10.3541542971741,36.0765018635767,-3.87317034519018));
#33280=CARTESIAN_POINT('Ctrl Pts',(-11.0212942781335,37.4381269352497,-7.48823335803968));
#33281=CARTESIAN_POINT('Ctrl Pts',(-11.446042279824,38.4555234045252,-9.12349227710921));
#33282=CARTESIAN_POINT('Ctrl Pts',(-12.4632402080729,41.026902971114,-11.8775764776601));
#33283=CARTESIAN_POINT('Ctrl Pts',(-13.0400785027102,42.5622713808053,-12.9726927515287));
#33284=CARTESIAN_POINT('Ctrl Pts',(-14.3045284731422,45.9581475303872,-14.4683433355075));
#33285=CARTESIAN_POINT('Ctrl Pts',(-14.963610809563,47.7744493565971,-14.8498038985338));
#33286=CARTESIAN_POINT('Ctrl Pts',(-15.6328286697389,49.6050326655024,-14.8500516281495));
#33287=CARTESIAN_POINT('Ctrl Pts',(-9.39535856987515,36.6790985320904,1.59674363861559));
#33288=CARTESIAN_POINT('Ctrl Pts',(-9.42749925373957,36.6453245303234,1.15301423609216));
#33289=CARTESIAN_POINT('Ctrl Pts',(-9.46019603501697,36.5974326448294,0.635579107012493));
#33290=CARTESIAN_POINT('Ctrl Pts',(-9.62291442709551,36.5487315518023,-1.86860431096297));
#33291=CARTESIAN_POINT('Ctrl Pts',(-9.84228740311376,36.8674137538594,-3.70979114470519));
#33292=CARTESIAN_POINT('Ctrl Pts',(-10.4902593585524,38.1668671434053,-7.17014261469044));
#33293=CARTESIAN_POINT('Ctrl Pts',(-10.9028003011769,39.1406457266856,-8.73670574474349));
#33294=CARTESIAN_POINT('Ctrl Pts',(-11.8865765112442,41.599116381909,-11.3734544105216));
#33295=CARTESIAN_POINT('Ctrl Pts',(-12.4447970770804,43.0690341146661,-12.4221714958371));
#33296=CARTESIAN_POINT('Ctrl Pts',(-13.6646070765712,46.3159892044746,-13.8545909095487));
#33297=CARTESIAN_POINT('Ctrl Pts',(-14.3020974767632,48.056213477209,-14.2195188099818));
#33298=CARTESIAN_POINT('Ctrl Pts',(-14.9473483165665,49.8063143340193,-14.2201291128084));
#33299=CARTESIAN_POINT('Ctrl Pts',(-11.786216904273,35.9142171164211,0.));
#33300=CARTESIAN_POINT('Ctrl Pts',(-11.90800808671,35.8791430893682,-1.86858636171601));
#33301=CARTESIAN_POINT('Ctrl Pts',(-12.1266171429531,36.1952232408274,-3.71029995871332));
#33302=CARTESIAN_POINT('Ctrl Pts',(-12.7754415589707,37.4975806517049,-7.16936247492168));
#33303=CARTESIAN_POINT('Ctrl Pts',(-13.1874595939467,38.4695778661641,-8.73699595765301));
#33304=CARTESIAN_POINT('Ctrl Pts',(-13.7294890038794,39.8242114819232,-10.1890856763526));
#33305=CARTESIAN_POINT('Ctrl Pts',(-13.7802180759655,39.9517643117923,-10.3203928635211));
#33306=CARTESIAN_POINT('Ctrl Pts',(-13.8316148870599,40.0817049410166,-10.4488603766049));
#33307=CARTESIAN_POINT('Ctrl Pts',(-9.50149509066497,36.5850719698906,1.66533453693773E-16));
#33308=CARTESIAN_POINT('Ctrl Pts',(-9.62291442709551,36.5487315518023,-1.86860431096297));
#33309=CARTESIAN_POINT('Ctrl Pts',(-9.84228740311376,36.8674137538594,-3.70979114470519));
#33310=CARTESIAN_POINT('Ctrl Pts',(-10.4902593585524,38.1668671434053,-7.17014261469044));
#33311=CARTESIAN_POINT('Ctrl Pts',(-10.9028003011769,39.1406457266856,-8.73670574474349));
#33312=CARTESIAN_POINT('Ctrl Pts',(-11.4474917709624,40.5018374092194,-10.1966053555702));
#33313=CARTESIAN_POINT('Ctrl Pts',(-11.5010595286477,40.6365673071016,-10.3350231942242));
#33314=CARTESIAN_POINT('Ctrl Pts',(-11.555373558984,40.773962973293,-10.4702558450947));
#33315=CARTESIAN_POINT('Ctrl Pts',(-15.7201209119707,41.7419576204997,1.2468908298857));
#33316=CARTESIAN_POINT('Ctrl Pts',(-15.7550797324014,41.7052222707522,0.764254661700232));
#33317=CARTESIAN_POINT('Ctrl Pts',(-15.7872856429843,41.6694633881723,0.332948671132101));
#33318=CARTESIAN_POINT('Ctrl Pts',(-15.9462356620105,41.6254618648259,-0.978870002714873));
#33319=CARTESIAN_POINT('Ctrl Pts',(-16.1248063760318,41.7773170936202,-1.98783577091336));
#33320=CARTESIAN_POINT('Ctrl Pts',(-16.5748099612649,42.4353694480747,-3.80852727281139));
#33321=CARTESIAN_POINT('Ctrl Pts',(-16.8558236637272,42.9396243660456,-4.65544360716497));
#33322=CARTESIAN_POINT('Ctrl Pts',(-17.4877814825015,44.2095709902023,-6.0499728334881));
#33323=CARTESIAN_POINT('Ctrl Pts',(-17.8478990309217,44.9832291227819,-6.61832169900053));
#33324=CARTESIAN_POINT('Ctrl Pts',(-18.5982747098126,46.6642543902471,-7.36768403081583));
#33325=CARTESIAN_POINT('Ctrl Pts',(-19.0065156676629,47.5974477252243,-7.57138648692284));
#33326=CARTESIAN_POINT('Ctrl Pts',(-19.3992863750337,48.4991757443115,-7.56962581969423));
#33327=CARTESIAN_POINT('Ctrl Pts',(-14.0037398626874,40.1090570584213,1.35489321026565));
#33328=CARTESIAN_POINT('Ctrl Pts',(-14.0378295966248,40.0732349602049,0.88425551828651));
#33329=CARTESIAN_POINT('Ctrl Pts',(-14.0701900799515,40.0337447201284,0.426396949022747));
#33330=CARTESIAN_POINT('Ctrl Pts',(-14.2303553472444,39.9884678119799,-1.25360819500586));
#33331=CARTESIAN_POINT('Ctrl Pts',(-14.4214462185203,40.1915678318707,-2.51960912781608));
#33332=CARTESIAN_POINT('Ctrl Pts',(-14.9326685312527,41.0479784867297,-4.84647586780456));
#33333=CARTESIAN_POINT('Ctrl Pts',(-15.2542422185737,41.6970325717764,-5.91572199042071));
#33334=CARTESIAN_POINT('Ctrl Pts',(-15.9948572088948,43.3340488505561,-7.69376028696617));
#33335=CARTESIAN_POINT('Ctrl Pts',(-16.4161147204151,44.3225950330595,-8.4106318655519));
#33336=CARTESIAN_POINT('Ctrl Pts',(-17.3114822382705,46.4872837874926,-9.37059840621415));
#33337=CARTESIAN_POINT('Ctrl Pts',(-17.7905076322735,47.6695948287831,-9.62435378631354));
#33338=CARTESIAN_POINT('Ctrl Pts',(-18.2612298390048,48.8333181822474,-9.62320046360538));
#33339=CARTESIAN_POINT('Ctrl Pts',(-12.6395284821797,38.1728270004196,1.47293192394301));
#33340=CARTESIAN_POINT('Ctrl Pts',(-12.6726703073998,38.1380009815349,1.01538091584913));
#33341=CARTESIAN_POINT('Ctrl Pts',(-12.7052063084714,38.0944634070468,0.528580717859076));
#33342=CARTESIAN_POINT('Ctrl Pts',(-12.8668122636161,38.0481727007018,-1.55402875454173));
#33343=CARTESIAN_POINT('Ctrl Pts',(-13.0714224335465,38.3067247111754,-3.10121432125182));
#33344=CARTESIAN_POINT('Ctrl Pts',(-13.6497783497329,39.3806906392349,-5.98129145449214));
#33345=CARTESIAN_POINT('Ctrl Pts',(-14.0155868029731,40.1876820275718,-7.29389406571664));
#33346=CARTESIAN_POINT('Ctrl Pts',(-14.8750601592335,42.2262312169582,-9.49113593808984));
#33347=CARTESIAN_POINT('Ctrl Pts',(-15.3631044396678,43.4495197173535,-10.3708286017074));
#33348=CARTESIAN_POINT('Ctrl Pts',(-16.4170971139001,46.143355468751,-11.5604045561346));
#33349=CARTESIAN_POINT('Ctrl Pts',(-16.973443488292,47.5979046271405,-11.8694761541855));
#33350=CARTESIAN_POINT('Ctrl Pts',(-17.5294501945613,49.0481649878422,-11.8687142284811));
#33351=CARTESIAN_POINT('Ctrl Pts',(-11.6799141290248,36.0076777827441,1.5964706812662));
#33352=CARTESIAN_POINT('Ctrl Pts',(-11.7120656519288,35.9738923911234,1.15259163661472));
#33353=CARTESIAN_POINT('Ctrl Pts',(-11.7447913705091,35.92614704651,0.635573001832125));
#33354=CARTESIAN_POINT('Ctrl Pts',(-11.90800808671,35.8791430893682,-1.86858636171601));
#33355=CARTESIAN_POINT('Ctrl Pts',(-12.1266171429531,36.1952232408274,-3.71029995871332));
#33356=CARTESIAN_POINT('Ctrl Pts',(-12.7754415589707,37.4975806517049,-7.16936247492168));
#33357=CARTESIAN_POINT('Ctrl Pts',(-13.1874595939467,38.4695778661641,-8.73699595765301));
#33358=CARTESIAN_POINT('Ctrl Pts',(-14.1714247212182,40.9286921018696,-11.3730256982666));
#33359=CARTESIAN_POINT('Ctrl Pts',(-14.7293359258389,42.3975559177982,-12.4235805192321));
#33360=CARTESIAN_POINT('Ctrl Pts',(-15.9494910259353,45.6456867796067,-13.85294708215));
#33361=CARTESIAN_POINT('Ctrl Pts',(-16.5867336459564,47.3851293551714,-14.2204718557261));
#33362=CARTESIAN_POINT('Ctrl Pts',(-17.2320701170944,49.135459485718,-14.2198708430666));
#33363=CARTESIAN_POINT('Ctrl Pts',(-9.39535856987514,36.6790985320904,1.59674363861559));
#33364=CARTESIAN_POINT('Ctrl Pts',(-9.42749925373957,36.6453245303234,1.15301423609216));
#33365=CARTESIAN_POINT('Ctrl Pts',(-9.46019603501696,36.5974326448294,0.635579107012493));
#33366=CARTESIAN_POINT('Ctrl Pts',(-9.6229144270955,36.5487315518023,-1.86860431096297));
#33367=CARTESIAN_POINT('Ctrl Pts',(-9.84228740311375,36.8674137538594,-3.709791144704));
#33368=CARTESIAN_POINT('Ctrl Pts',(-10.4902593585524,38.1668671434053,-7.17014261469164));
#33369=CARTESIAN_POINT('Ctrl Pts',(-10.9028003011769,39.1406457266856,-8.7367057447411));
#33370=CARTESIAN_POINT('Ctrl Pts',(-11.8865765112442,41.599116381909,-11.373454410524));
#33371=CARTESIAN_POINT('Ctrl Pts',(-12.4447970770804,43.0690341146661,-12.4221714958419));
#33372=CARTESIAN_POINT('Ctrl Pts',(-13.6646070765712,46.3159892044746,-13.8545909095439));
#33373=CARTESIAN_POINT('Ctrl Pts',(-14.3020974767647,48.0562134772085,-14.2195188099818));
#33374=CARTESIAN_POINT('Ctrl Pts',(-14.9473483165665,49.8063143340193,-14.2201291128084));
#33375=CARTESIAN_POINT('Ctrl Pts',(-9.75977978596927,39.019172373722,1.47327599461702));
#33376=CARTESIAN_POINT('Ctrl Pts',(-9.79290794826535,38.9843607120663,1.01591361477664));
#33377=CARTESIAN_POINT('Ctrl Pts',(-9.82540747302437,38.9406384185529,0.528588413616415));
#33378=CARTESIAN_POINT('Ctrl Pts',(-9.98638527612875,38.8922084230791,-1.55405138008933));
#33379=CARTESIAN_POINT('Ctrl Pts',(-10.1919583891427,39.1540403939766,-3.1005729464026));
#33380=CARTESIAN_POINT('Ctrl Pts',(-10.7692397539852,40.2243457187347,-5.9822748433503));
#33381=CARTESIAN_POINT('Ctrl Pts',(-11.1357073475209,41.0335825742498,-7.29352824390964));
#33382=CARTESIAN_POINT('Ctrl Pts',(-11.9949425681495,43.0713205117329,-9.49167634234821));
#33383=CARTESIAN_POINT('Ctrl Pts',(-12.4833768073893,44.2959375049237,-10.3690524867635));
#33384=CARTESIAN_POINT('Ctrl Pts',(-13.5369344722799,46.9882911615409,-11.562476648351));
#33385=CARTESIAN_POINT('Ctrl Pts',(-14.0935974137202,48.4438248432674,-11.8682745705641));
#33386=CARTESIAN_POINT('Ctrl Pts',(-14.6494919462609,49.8937970264262,-11.8690397849988));
#33387=CARTESIAN_POINT('Ctrl Pts',(-9.66008352082082,41.385638397964,1.35541218776085));
#33388=CARTESIAN_POINT('Ctrl Pts',(-9.69415264634654,41.3498379554236,0.885059012381331));
#33389=CARTESIAN_POINT('Ctrl Pts',(-9.72645811078717,41.310069095201,0.426408556884646));
#33390=CARTESIAN_POINT('Ctrl Pts',(-9.88567590769772,41.2615653996593,-1.25364232215155));
#33391=CARTESIAN_POINT('Ctrl Pts',(-10.0782192299594,41.4696127334992,-2.51864171286803));
#33392=CARTESIAN_POINT('Ctrl Pts',(-10.5878207478773,42.3205019333897,-4.84795915808608));
#33393=CARTESIAN_POINT('Ctrl Pts',(-10.9103886465764,42.9729429590254,-5.91517020469687));
#33394=CARTESIAN_POINT('Ctrl Pts',(-11.6506444460607,44.6087355895508,-7.69457540336642));
#33395=CARTESIAN_POINT('Ctrl Pts',(-12.0724901502383,45.5992855983428,-8.4079528703493));
#33396=CARTESIAN_POINT('Ctrl Pts',(-12.9672015236564,47.7617388416072,-9.37372383744032));
#33397=CARTESIAN_POINT('Ctrl Pts',(-13.4467134169802,48.9455328277889,-9.62254086000153));
#33398=CARTESIAN_POINT('Ctrl Pts',(-13.9172574201603,50.1088235664895,-9.62369151535392));
#33399=CARTESIAN_POINT('Ctrl Pts',(-9.10010115416782,43.6875520748214,1.24768178593787));
#33400=CARTESIAN_POINT('Ctrl Pts',(-9.13502856601633,43.6508497297507,0.765479239882089));
#33401=CARTESIAN_POINT('Ctrl Pts',(-9.1671506241734,43.6146662116331,0.332966362281924));
#33402=CARTESIAN_POINT('Ctrl Pts',(-9.32465663562954,43.5657468507322,-0.978922014743682));
#33403=CARTESIAN_POINT('Ctrl Pts',(-9.50544098108401,43.7251421134386,-1.98636136650516));
#33404=CARTESIAN_POINT('Ctrl Pts',(-9.95297436774496,44.3747794050551,-3.81078790537194));
#33405=CARTESIAN_POINT('Ctrl Pts',(-10.2355033141481,44.8841962446583,-4.65460264920513));
#33406=CARTESIAN_POINT('Ctrl Pts',(-10.8669137023194,46.1522779478965,-6.0512151248278));
#33407=CARTESIAN_POINT('Ctrl Pts',(-11.2279276952814,46.9289900443738,-6.61423873299737));
#33408=CARTESIAN_POINT('Ctrl Pts',(-11.9773033666127,48.6066082448324,-7.3724473948671));
#33409=CARTESIAN_POINT('Ctrl Pts',(-12.3863053996918,49.5420562727389,-7.56862230169559));
#33410=CARTESIAN_POINT('Ctrl Pts',(-12.7787848949964,50.4431303715412,-7.57037421506015));
#33411=CARTESIAN_POINT('Ctrl Pts',(-6.43660260973351,37.3033966274914,1.59647061166213));
#33412=CARTESIAN_POINT('Ctrl Pts',(-6.47323503721941,37.2745307626499,1.15259158901731));
#33413=CARTESIAN_POINT('Ctrl Pts',(-6.51242252436846,37.2319287549577,0.63557297028587));
#33414=CARTESIAN_POINT('Ctrl Pts',(-6.68066728815624,37.2086313911844,-1.8685863618375));
#33415=CARTESIAN_POINT('Ctrl Pts',(-6.85206832386127,37.5526056149556,-3.71029995870329));
#33416=CARTESIAN_POINT('Ctrl Pts',(-7.30894385840923,38.9340442470357,-7.16936247493174));
#33417=CARTESIAN_POINT('Ctrl Pts',(-7.57843851743967,39.9547842114114,-8.73699595771817));
#33418=CARTESIAN_POINT('Ctrl Pts',(-8.20241985397056,42.5289010478495,-11.3730256982015));
#33419=CARTESIAN_POINT('Ctrl Pts',(-8.54561121040599,44.0622129909419,-12.4235805192329));
#33420=CARTESIAN_POINT('Ctrl Pts',(-9.29108967267749,47.4509287397322,-13.8529470821493));
#33421=CARTESIAN_POINT('Ctrl Pts',(-9.67429759304514,49.2633553782986,-14.2204718556406));
#33422=CARTESIAN_POINT('Ctrl Pts',(-10.063967519702,51.0877106274638,-14.2198708430667));
#33423=CARTESIAN_POINT('Ctrl Pts',(-5.63986099173572,36.7825298650421,1.62964605326979));
#33424=CARTESIAN_POINT('Ctrl Pts',(-5.67618780432403,36.753904820676,1.18947019887616));
#33425=CARTESIAN_POINT('Ctrl Pts',(-5.71558400588145,36.7101544788345,0.664243925045137));
#33426=CARTESIAN_POINT('Ctrl Pts',(-5.88421645976361,36.6862652424053,-1.95287905134559));
#33427=CARTESIAN_POINT('Ctrl Pts',(-6.05723890417332,37.046743060744,-3.87337387078904));
#33428=CARTESIAN_POINT('Ctrl Pts',(-6.52398110941249,38.4906509831423,-7.48792130213652));
#33429=CARTESIAN_POINT('Ctrl Pts',(-6.79950954684187,39.5574047047037,-9.1236083623219));
#33430=CARTESIAN_POINT('Ctrl Pts',(-7.44044656128092,42.2476392596818,-11.8774049927092));
#33431=CARTESIAN_POINT('Ctrl Pts',(-7.79284527697299,43.8490375949694,-12.9732563608828));
#33432=CARTESIAN_POINT('Ctrl Pts',(-8.56121110821509,47.3907837817554,-14.467685804552));
#33433=CARTESIAN_POINT('Ctrl Pts',(-8.95504492395579,49.2820718587439,-14.8501851005484));
#33434=CARTESIAN_POINT('Ctrl Pts',(-9.35695250368079,51.1893577615275,-14.8499483202528));
#33435=CARTESIAN_POINT('Ctrl Pts',(-4.69711890654725,36.9183140647621,1.62975523620955));
#33436=CARTESIAN_POINT('Ctrl Pts',(-4.73344077927283,36.8896929129394,1.18963923866306));
#33437=CARTESIAN_POINT('Ctrl Pts',(-4.77283386569913,36.8458829040853,0.664246367114009));
#33438=CARTESIAN_POINT('Ctrl Pts',(-4.94136562987182,36.8212933555072,-1.95288623103511));
#33439=CARTESIAN_POINT('Ctrl Pts',(-5.11454240778336,37.1828448868685,-3.87317034519198));
#33440=CARTESIAN_POINT('Ctrl Pts',(-5.58111241365297,38.6255544971415,-7.48823335803775));
#33441=CARTESIAN_POINT('Ctrl Pts',(-5.85674647907816,39.6930432805413,-9.12349227713124));
#33442=CARTESIAN_POINT('Ctrl Pts',(-6.4976453322125,42.3830122692843,-11.877576477638));
#33443=CARTESIAN_POINT('Ctrl Pts',(-6.85010653765407,43.9848454910637,-12.9726927515151));
#33444=CARTESIAN_POINT('Ctrl Pts',(-7.61840266562128,47.5261065109321,-14.468343335521));
#33445=CARTESIAN_POINT('Ctrl Pts',(-8.01228979377304,49.4177181994984,-14.8498038986051));
#33446=CARTESIAN_POINT('Ctrl Pts',(-8.41417681322632,51.3249084414062,-14.8500516281495));
#33447=CARTESIAN_POINT('Ctrl Pts',(-4.07974739676235,37.6428571267913,1.59674356901154));
#33448=CARTESIAN_POINT('Ctrl Pts',(-4.11636747459172,37.6140009933267,1.1530141884832));
#33449=CARTESIAN_POINT('Ctrl Pts',(-4.15554717391304,37.5712498180871,0.63557907545804));
#33450=CARTESIAN_POINT('Ctrl Pts',(-4.32354021342559,37.5462016739318,-1.86860431106127));
#33451=CARTESIAN_POINT('Ctrl Pts',(-4.49532708288728,37.8928601802523,-3.70979114471065));
#33452=CARTESIAN_POINT('Ctrl Pts',(-4.95177211900954,39.2713030320479,-7.17014261468482));
#33453=CARTESIAN_POINT('Ctrl Pts',(-5.22153084803041,40.293880650996,-8.73670574474153));
#33454=CARTESIAN_POINT('Ctrl Pts',(-5.84541678129948,42.8673335718654,-11.3734544105234));
#33455=CARTESIAN_POINT('Ctrl Pts',(-6.18876436210449,44.401732731168,-12.4221714958234));
#33456=CARTESIAN_POINT('Ctrl Pts',(-6.93406856619723,47.7892355626834,-13.8545909095623));
#33457=CARTESIAN_POINT('Ctrl Pts',(-7.31741049758119,49.602471204667,-14.2195188100911));
#33458=CARTESIAN_POINT('Ctrl Pts',(-7.70702829356578,51.4265873271605,-14.2201291128084));
#33459=CARTESIAN_POINT('Ctrl Pts',(-6.55512420987382,37.2260157227863,1.04083408558608E-14));
#33460=CARTESIAN_POINT('Ctrl Pts',(-6.68066728815625,37.2086313911844,-1.86858636183749));
#33461=CARTESIAN_POINT('Ctrl Pts',(-6.85206832386186,37.5526056149556,-3.71029995870209));
#33462=CARTESIAN_POINT('Ctrl Pts',(-7.30894385840864,38.9340442470356,-7.16936247493294));
#33463=CARTESIAN_POINT('Ctrl Pts',(-7.57843851743848,39.9547842114066,-8.73699595771578));
#33464=CARTESIAN_POINT('Ctrl Pts',(-7.92216638571018,41.3727684379706,-10.1890856763487));
#33465=CARTESIAN_POINT('Ctrl Pts',(-7.95422644864385,41.5062424636381,-10.3203928635145));
#33466=CARTESIAN_POINT('Ctrl Pts',(-7.98660763468405,41.6421750134759,-10.4488603765967));
#33467=CARTESIAN_POINT('Ctrl Pts',(-4.19818497005511,37.5648924257372,1.0547118733939E-15));
#33468=CARTESIAN_POINT('Ctrl Pts',(-4.32354021342559,37.5462016739318,-1.86860431106127));
#33469=CARTESIAN_POINT('Ctrl Pts',(-4.49532708288728,37.8928601802523,-3.70979114471065));
#33470=CARTESIAN_POINT('Ctrl Pts',(-4.95177211900954,39.2713030320479,-7.17014261468482));
#33471=CARTESIAN_POINT('Ctrl Pts',(-5.22153084803041,40.293880650996,-8.73670574474153));
#33472=CARTESIAN_POINT('Ctrl Pts',(-5.56696037000281,41.7187350432347,-10.1966053555725));
#33473=CARTESIAN_POINT('Ctrl Pts',(-5.60080882153535,41.8597170717889,-10.3350231942285));
#33474=CARTESIAN_POINT('Ctrl Pts',(-5.6350165713511,42.0034439406478,-10.4702558451009));
#33475=CARTESIAN_POINT('Ctrl Pts',(-9.61961280540192,43.5542911395532,1.24689076028089));
#33476=CARTESIAN_POINT('Ctrl Pts',(-9.65944377882146,43.5229048631143,0.764254616140159));
#33477=CARTESIAN_POINT('Ctrl Pts',(-9.69641089756402,43.4920933360794,0.332948654561765));
#33478=CARTESIAN_POINT('Ctrl Pts',(-9.86000510220709,43.4711606313009,-0.978870002647285));
#33479=CARTESIAN_POINT('Ctrl Pts',(-10.0151469714658,43.6468834551719,-1.98783577088628));
#33480=CARTESIAN_POINT('Ctrl Pts',(-10.3669195547307,44.362279972836,-3.8085272728388));
#33481=CARTESIAN_POINT('Ctrl Pts',(-10.5733099858402,44.9013947223877,-4.65544360724677));
#33482=CARTESIAN_POINT('Ctrl Pts',(-11.0181031366183,46.2483520960035,-6.04997283340668));
#33483=CARTESIAN_POINT('Ctrl Pts',(-11.2644521757368,47.065385574864,-6.61832169903466));
#33484=CARTESIAN_POINT('Ctrl Pts',(-11.7679552730498,48.836090022354,-7.36768403078205));
#33485=CARTESIAN_POINT('Ctrl Pts',(-12.0392336678225,49.8178835406777,-7.57138648668505));
#33486=CARTESIAN_POINT('Ctrl Pts',(-12.2996772587578,50.7663303683513,-7.56962581969437));
#33487=CARTESIAN_POINT('Ctrl Pts',(-8.15308801979184,41.6937446593044,1.35489314066107));
#33488=CARTESIAN_POINT('Ctrl Pts',(-8.19192878357286,41.6631386548741,0.884255472094997));
#33489=CARTESIAN_POINT('Ctrl Pts',(-8.22957992923835,41.6286557481991,0.426396927826334));
#33490=CARTESIAN_POINT('Ctrl Pts',(-8.39455851882925,41.6066335880669,-1.2536081949919));
#33491=CARTESIAN_POINT('Ctrl Pts',(-8.55480021407532,41.8348614090877,-2.51960912779828));
#33492=CARTESIAN_POINT('Ctrl Pts',(-8.93893907695677,42.7553095590112,-4.84647586782256));
#33493=CARTESIAN_POINT('Ctrl Pts',(-9.16486958068628,43.4435219166124,-5.91572199048099));
#33494=CARTESIAN_POINT('Ctrl Pts',(-9.66497447126952,45.1692762327416,-7.69376028690614));
#33495=CARTESIAN_POINT('Ctrl Pts',(-9.94125939867021,46.2077116350292,-8.41063186557169));
#33496=CARTESIAN_POINT('Ctrl Pts',(-10.5194460361915,48.4777910626842,-9.37059840619458));
#33497=CARTESIAN_POINT('Ctrl Pts',(-10.8253352376626,49.7162403038104,-9.6243537861852));
#33498=CARTESIAN_POINT('Ctrl Pts',(-11.1256510703085,50.9351093861917,-9.62320046360547));
#33499=CARTESIAN_POINT('Ctrl Pts',(-7.07831661167178,39.5830751094924,1.47293185433868));
#33500=CARTESIAN_POINT('Ctrl Pts',(-7.11607735826593,39.5533201442214,1.01538086897001));
#33501=CARTESIAN_POINT('Ctrl Pts',(-7.1544782308666,39.5148560779778,0.528580691605906));
#33502=CARTESIAN_POINT('Ctrl Pts',(-7.32102712268554,39.4920354699227,-1.55402875459162));
#33503=CARTESIAN_POINT('Ctrl Pts',(-7.48675886858976,39.7770748570026,-3.1012143212373));
#33504=CARTESIAN_POINT('Ctrl Pts',(-7.90638666804229,40.9224179890837,-5.98129145450676));
#33505=CARTESIAN_POINT('Ctrl Pts',(-8.15362486974844,41.7732553395417,-7.29389406576977));
#33506=CARTESIAN_POINT('Ctrl Pts',(-8.71423422839184,43.913370849246,-9.49113593803685));
#33507=CARTESIAN_POINT('Ctrl Pts',(-9.02321881659917,45.1936639793709,-10.3708286017225));
#33508=CARTESIAN_POINT('Ctrl Pts',(-9.68311056587086,48.0100791639859,-11.5604045561196));
#33509=CARTESIAN_POINT('Ctrl Pts',(-10.0267902081675,49.5289994535078,-11.8694761541237));
#33510=CARTESIAN_POINT('Ctrl Pts',(-10.3707439991144,51.0436262593385,-11.8687142284812));
#33511=CARTESIAN_POINT('Ctrl Pts',(-6.43660260973353,37.3033966274914,1.59647061166213));
#33512=CARTESIAN_POINT('Ctrl Pts',(-6.47323503721941,37.2745307626499,1.15259158901731));
#33513=CARTESIAN_POINT('Ctrl Pts',(-6.51242252436846,37.2319287549577,0.63557297028587));
#33514=CARTESIAN_POINT('Ctrl Pts',(-6.68066728815625,37.2086313911843,-1.8685863618375));
#33515=CARTESIAN_POINT('Ctrl Pts',(-6.85206832386186,37.5526056149556,-3.71029995870209));
#33516=CARTESIAN_POINT('Ctrl Pts',(-7.30894385840864,38.9340442470356,-7.16936247493294));
#33517=CARTESIAN_POINT('Ctrl Pts',(-7.57843851743848,39.9547842114066,-8.73699595771578));
#33518=CARTESIAN_POINT('Ctrl Pts',(-8.20241985397175,42.5289010478543,-11.3730256982039));
#33519=CARTESIAN_POINT('Ctrl Pts',(-8.545611210406,44.0622129909466,-12.423580519233));
#33520=CARTESIAN_POINT('Ctrl Pts',(-9.2910896726775,47.4509287397274,-13.8529470821493));
#33521=CARTESIAN_POINT('Ctrl Pts',(-9.67429759304181,49.2633553783029,-14.2204718556406));
#33522=CARTESIAN_POINT('Ctrl Pts',(-10.063967519702,51.0877106274638,-14.2198708430667));
#33523=CARTESIAN_POINT('Ctrl Pts',(-4.07974739676235,37.6428571267913,1.59674356901154));
#33524=CARTESIAN_POINT('Ctrl Pts',(-4.11636747459172,37.6140009933267,1.15301418848321));
#33525=CARTESIAN_POINT('Ctrl Pts',(-4.15554717391304,37.5712498180871,0.635579075458043));
#33526=CARTESIAN_POINT('Ctrl Pts',(-4.32354021342559,37.5462016739318,-1.86860431106127));
#33527=CARTESIAN_POINT('Ctrl Pts',(-4.49532708288667,37.8928601802523,-3.70979114470945));
#33528=CARTESIAN_POINT('Ctrl Pts',(-4.95177211901013,39.2713030320479,-7.17014261468602));
#33529=CARTESIAN_POINT('Ctrl Pts',(-5.2215308480298,40.2938806509912,-8.73670574474154));
#33530=CARTESIAN_POINT('Ctrl Pts',(-5.84541678130007,42.8673335718702,-11.3734544105235));
#33531=CARTESIAN_POINT('Ctrl Pts',(-6.18876436210508,44.4017327311728,-12.4221714958234));
#33532=CARTESIAN_POINT('Ctrl Pts',(-6.93406856619663,47.7892355626786,-13.8545909095623));
#33533=CARTESIAN_POINT('Ctrl Pts',(-7.31741049758291,49.6024712046703,-14.2195188100911));
#33534=CARTESIAN_POINT('Ctrl Pts',(-7.70702829356578,51.4265873271605,-14.2201291128084));
#33535=CARTESIAN_POINT('Ctrl Pts',(-4.10743210000917,40.0109749372548,1.4732759250127));
#33536=CARTESIAN_POINT('Ctrl Pts',(-4.1451772795017,39.9812322386711,1.01591356788184));
#33537=CARTESIAN_POINT('Ctrl Pts',(-4.18356833531979,39.9425801423931,0.528588387352919));
#33538=CARTESIAN_POINT('Ctrl Pts',(-4.34979992137163,39.9175526247723,-1.55405138010999));
#33539=CARTESIAN_POINT('Ctrl Pts',(-4.51601802194056,40.2059756280482,-3.10057294640714));
#33540=CARTESIAN_POINT('Ctrl Pts',(-4.93510316561713,41.3475424919709,-5.98227484334561));
#33541=CARTESIAN_POINT('Ctrl Pts',(-5.1826742352202,42.2006962594516,-7.29352824388366));
#33542=CARTESIAN_POINT('Ctrl Pts',(-5.74316333527953,44.3399748842767,-9.491676342374));
#33543=CARTESIAN_POINT('Ctrl Pts',(-6.05234484884677,45.6216384820463,-10.3690524867497));
#33544=CARTESIAN_POINT('Ctrl Pts',(-6.71201694061643,48.4365247491691,-11.5624766483647));
#33545=CARTESIAN_POINT('Ctrl Pts',(-7.0558698155059,49.9564645931987,-11.8682745706829));
#33546=CARTESIAN_POINT('Ctrl Pts',(-7.39975358641498,51.4707901907297,-11.8690397849987));
#33547=CARTESIAN_POINT('Ctrl Pts',(-3.67196736957042,42.3391654916811,1.35541211815631));
#33548=CARTESIAN_POINT('Ctrl Pts',(-3.71078465278244,42.3085779896597,0.885058966166922));
#33549=CARTESIAN_POINT('Ctrl Pts',(-3.74842099134597,42.2738114687004,0.426408535672664));
#33550=CARTESIAN_POINT('Ctrl Pts',(-3.91292097417315,42.2484605261848,-1.25364232209351));
#33551=CARTESIAN_POINT('Ctrl Pts',(-4.07389626035039,42.4817920098841,-2.51864171287881));
#33552=CARTESIAN_POINT('Ctrl Pts',(-4.45721661076271,43.39654424226,-4.84795915807511));
#33553=CARTESIAN_POINT('Ctrl Pts',(-4.68364919433047,44.0882505573392,-5.91517020463728));
#33554=CARTESIAN_POINT('Ctrl Pts',(-5.18357269340369,45.8127425618219,-7.69457540342575));
#33555=CARTESIAN_POINT('Ctrl Pts',(-5.46015465230814,46.8532451029886,-8.40795287033531));
#33556=CARTESIAN_POINT('Ctrl Pts',(-6.03800997040064,49.121018394627,-9.37372383745409));
#33557=CARTESIAN_POINT('Ctrl Pts',(-6.34416967429387,50.3610047225046,-9.62254086018695));
#33558=CARTESIAN_POINT('Ctrl Pts',(-6.64437068472167,51.5794202324977,-9.62369151535378));
#33559=CARTESIAN_POINT('Ctrl Pts',(-2.79008834334092,44.5379552064474,1.24768171633309));
#33560=CARTESIAN_POINT('Ctrl Pts',(-2.82988353081818,44.5065971288888,0.765479194287426));
#33561=CARTESIAN_POINT('Ctrl Pts',(-2.86682808255848,44.4753533549302,0.332966345687857));
#33562=CARTESIAN_POINT('Ctrl Pts',(-3.02969285881549,44.449347365471,-0.978922014608904));
#33563=CARTESIAN_POINT('Ctrl Pts',(-3.18595276920677,44.632848509067,-1.98636136651854));
#33564=CARTESIAN_POINT('Ctrl Pts',(-3.53647788529618,45.3395640713889,-3.8107879053583));
#33565=CARTESIAN_POINT('Ctrl Pts',(-3.74363351930891,45.8840038433944,-4.65460264909516));
#33566=CARTESIAN_POINT('Ctrl Pts',(-4.18815021742049,47.2290373705107,-6.05121512493738));
#33567=CARTESIAN_POINT('Ctrl Pts',(-4.43495195221376,48.0492213058477,-6.61423873296882));
#33568=CARTESIAN_POINT('Ctrl Pts',(-4.93795009678085,49.8164110493997,-7.37244739489531));
#33569=CARTESIAN_POINT('Ctrl Pts',(-5.20966094389456,50.8005446234645,-7.56862230199518));
#33570=CARTESIAN_POINT('Ctrl Pts',(-5.46990934942758,51.7483027430073,-7.57037421505994));
#33571=CARTESIAN_POINT('Ctrl Pts',(-1.06226042837003,37.8397258902528,1.59647049649061));
#33572=CARTESIAN_POINT('Ctrl Pts',(-1.1026280281322,37.8163671782172,1.15259151032668));
#33573=CARTESIAN_POINT('Ctrl Pts',(-1.14747953738506,37.7797757625757,0.635572917996464));
#33574=CARTESIAN_POINT('Ctrl Pts',(-1.31732736909556,37.7806592587273,-1.86858636177033));
#33575=CARTESIAN_POINT('Ctrl Pts',(-1.43803115336731,38.1455252315354,-3.71029995869598));
#33576=CARTESIAN_POINT('Ctrl Pts',(-1.69365713820691,39.5779229780087,-7.16936247493924));
#33577=CARTESIAN_POINT('Ctrl Pts',(-1.81514228728896,40.6266263701707,-8.73699595770183));
#33578=CARTESIAN_POINT('Ctrl Pts',(-2.06643737216329,43.2633442117449,-11.373025698218));
#33579=CARTESIAN_POINT('Ctrl Pts',(-2.18792249430895,44.8298904725309,-12.4235805192224));
#33580=CARTESIAN_POINT('Ctrl Pts',(-2.44354852690307,48.2902066278842,-13.85294708216));
#33581=CARTESIAN_POINT('Ctrl Pts',(-2.56492073910889,50.1387215498278,-14.2204718556691));
#33582=CARTESIAN_POINT('Ctrl Pts',(-2.69099156569461,51.9999633056261,-14.2198708430667));
#33583=CARTESIAN_POINT('Ctrl Pts',(-0.347755560296872,37.2107726459064,
1.62964593809825));
#33584=CARTESIAN_POINT('Ctrl Pts',(-0.387786383582009,37.1876088095763,
1.18947011987008));
#33585=CARTESIAN_POINT('Ctrl Pts',(-0.433007907800631,37.1499104513488,
0.664243870396088));
#33586=CARTESIAN_POINT('Ctrl Pts',(-0.603323715733815,37.150263273314,-1.95287905127288));
#33587=CARTESIAN_POINT('Ctrl Pts',(-0.723283698713102,37.5316956084199,
-3.87337387078179));
#33588=CARTESIAN_POINT('Ctrl Pts',(-0.979785618814999,39.027330971542,-7.48792130214399));
#33589=CARTESIAN_POINT('Ctrl Pts',(-1.10069469072641,40.1224384633822,-9.12360836231754));
#33590=CARTESIAN_POINT('Ctrl Pts',(-1.35224759480685,42.8765051571252,-11.8774049927137));
#33591=CARTESIAN_POINT('Ctrl Pts',(-1.47315665468807,44.5117551326448,-12.9732563608769));
#33592=CARTESIAN_POINT('Ctrl Pts',(-1.72965859378935,48.1268013089941,-14.4676858045579));
#33593=CARTESIAN_POINT('Ctrl Pts',(-1.85032539219324,50.0548871962143,-14.8501851005342));
#33594=CARTESIAN_POINT('Ctrl Pts',(-1.97670704765985,51.9999570907662,-14.8499483202528));
#33595=CARTESIAN_POINT('Ctrl Pts',(0.604714876209436,37.2110085708708,1.62975512103804));
#33596=CARTESIAN_POINT('Ctrl Pts',(0.564689496472757,37.1878478844499,1.18963915964465));
#33597=CARTESIAN_POINT('Ctrl Pts',(0.519462564176599,37.1500900231906,0.664246312466032));
#33598=CARTESIAN_POINT('Ctrl Pts',(0.34914675626714,37.1497353315388,-1.95288623096613));
#33599=CARTESIAN_POINT('Ctrl Pts',(0.229186815972868,37.5322524147635,-3.87317034518712));
#33600=CARTESIAN_POINT('Ctrl Pts',(-0.0273151950961962,39.0266771563424,
-7.48823335804281));
#33601=CARTESIAN_POINT('Ctrl Pts',(-0.148224209656999,40.1225272605589,
-9.12349227713644));
#33602=CARTESIAN_POINT('Ctrl Pts',(-0.399777134874554,42.8763256602578,
-11.8775764776329));
#33603=CARTESIAN_POINT('Ctrl Pts',(-0.520686157648164,44.5120149889529,
-12.9726927515284));
#33604=CARTESIAN_POINT('Ctrl Pts',(-0.777188149407516,48.1265710168792,
-14.4683433355078));
#33605=CARTESIAN_POINT('Ctrl Pts',(-0.897861662853957,50.0549848089201,
-14.8498038985528));
#33606=CARTESIAN_POINT('Ctrl Pts',(-1.02423658127914,51.9999570902567,-14.8500516281495));
#33607=CARTESIAN_POINT('Ctrl Pts',(1.31891566289573,37.8403157026637,1.59674345384007));
#33608=CARTESIAN_POINT('Ctrl Pts',(1.27856167200511,37.816964865386,1.15301410976404));
#33609=CARTESIAN_POINT('Ctrl Pts',(1.233696642558,37.7802246921785,0.635579023171323));
#33610=CARTESIAN_POINT('Ctrl Pts',(1.06384881090688,37.7793394042942,-1.86860431100347));
#33611=CARTESIAN_POINT('Ctrl Pts',(0.943145133347886,38.1469172473993,-3.70979114470452));
#33612=CARTESIAN_POINT('Ctrl Pts',(0.687518921089835,39.5762884400051,-7.17014261469109));
#33613=CARTESIAN_POINT('Ctrl Pts',(0.566033915384876,40.6268483631173,-8.73670574474909));
#33614=CARTESIAN_POINT('Ctrl Pts',(0.314738777667144,43.2628954695716,-11.373454410516));
#33615=CARTESIAN_POINT('Ctrl Pts',(0.193253748290465,44.8305401132961,-12.4221714958367));
#33616=CARTESIAN_POINT('Ctrl Pts',(-0.062372415948142,48.2896308976019,
-13.8545909095489));
#33617=CARTESIAN_POINT('Ctrl Pts',(-0.183762141934923,50.1389656602283,
-14.2195188100007));
#33618=CARTESIAN_POINT('Ctrl Pts',(-0.309815399742848,51.9999633043523,
-14.2201291128083));
#33619=CARTESIAN_POINT('Ctrl Pts',(-1.19058808997908,37.7800000000001,0.));
#33620=CARTESIAN_POINT('Ctrl Pts',(-1.31732736909556,37.7806592587273,-1.86858636177033));
#33621=CARTESIAN_POINT('Ctrl Pts',(-1.43803115336732,38.1455252315354,-3.71029995869598));
#33622=CARTESIAN_POINT('Ctrl Pts',(-1.69365713820691,39.5779229780087,-7.16936247493924));
#33623=CARTESIAN_POINT('Ctrl Pts',(-1.81514228728896,40.6266263701707,-8.73699595770183));
#33624=CARTESIAN_POINT('Ctrl Pts',(-1.95357130555243,42.0790951378326,-10.1890856763505));
#33625=CARTESIAN_POINT('Ctrl Pts',(-1.96630970889271,42.2157732130427,-10.3203928635177));
#33626=CARTESIAN_POINT('Ctrl Pts',(-1.9790160823007,42.3549304887752,-10.4488603766009));
#33627=CARTESIAN_POINT('Ctrl Pts',(1.19058808997906,37.78,-4.44089209850063E-16));
#33628=CARTESIAN_POINT('Ctrl Pts',(1.06384881090688,37.7793394042942,-1.86860431100347));
#33629=CARTESIAN_POINT('Ctrl Pts',(0.943145133347886,38.1469172473993,-3.70979114470452));
#33630=CARTESIAN_POINT('Ctrl Pts',(0.687518921089835,39.5762884400051,-7.17014261469109));
#33631=CARTESIAN_POINT('Ctrl Pts',(0.566033915384876,40.6268483631173,-8.73670574474909));
#33632=CARTESIAN_POINT('Ctrl Pts',(0.42689829031798,42.0863595386748,-10.1966053555719));
#33633=CARTESIAN_POINT('Ctrl Pts',(0.413458201812741,42.2307237103642,-10.3350231942277));
#33634=CARTESIAN_POINT('Ctrl Pts',(0.400053103665672,42.3778559173188,-10.4702558451));
#33635=CARTESIAN_POINT('Ctrl Pts',(-3.32327712822014,44.4799848904464,1.24689064510954));
#33636=CARTESIAN_POINT('Ctrl Pts',(-3.36716940899972,44.4545866217131,0.764254540719014));
#33637=CARTESIAN_POINT('Ctrl Pts',(-3.40814518985254,44.429349685102,0.332948627185768));
#33638=CARTESIAN_POINT('Ctrl Pts',(-3.5730532724122,44.4319119278293,-0.97887000265947));
#33639=CARTESIAN_POINT('Ctrl Pts',(-3.70160805588082,44.6279251367563,-1.98783577088437));
#33640=CARTESIAN_POINT('Ctrl Pts',(-3.94798856176874,45.38610240764,-3.80852727284065));
#33641=CARTESIAN_POINT('Ctrl Pts',(-4.07555420744412,45.9491021672715,-4.65544360722303));
#33642=CARTESIAN_POINT('Ctrl Pts',(-4.32412798456521,47.3456501222045,-6.04997283343043));
#33643=CARTESIAN_POINT('Ctrl Pts',(-4.4516935582032,48.1894265020396,-6.61832169899101));
#33644=CARTESIAN_POINT('Ctrl Pts',(-4.6980742029572,50.0137636932261,-7.36768403082578));
#33645=CARTESIAN_POINT('Ctrl Pts',(-4.82686758916904,51.0241709100527,-7.57138648682318));
#33646=CARTESIAN_POINT('Ctrl Pts',(-4.94968218283415,52.0000289040989,-7.56962581969448));
#33647=CARTESIAN_POINT('Ctrl Pts',(-2.13646282181017,42.4296678529921,1.35489302548968));
#33648=CARTESIAN_POINT('Ctrl Pts',(-2.17926392766629,42.4049009926309,0.884255395658553));
#33649=CARTESIAN_POINT('Ctrl Pts',(-2.2214392647697,42.3761273929605,0.426396892757908));
#33650=CARTESIAN_POINT('Ctrl Pts',(-2.38787268687498,42.3778082879602,-1.25360819498149));
#33651=CARTESIAN_POINT('Ctrl Pts',(-2.51400314727613,42.6265178497758,-2.51960912779656));
#33652=CARTESIAN_POINT('Ctrl Pts',(-2.76323860082849,43.5922658248206,-4.8464758678243));
#33653=CARTESIAN_POINT('Ctrl Pts',(-2.88892662741111,44.3056264360907,-5.91572199046689));
#33654=CARTESIAN_POINT('Ctrl Pts',(-3.13834072492098,46.0849874081721,-7.69376028692028));
#33655=CARTESIAN_POINT('Ctrl Pts',(-3.26402870377777,47.1521724801729,-8.41063186554706));
#33656=CARTESIAN_POINT('Ctrl Pts',(-3.51326424840902,49.4814303102183,-9.37059840621927));
#33657=CARTESIAN_POINT('Ctrl Pts',(-3.63979023544687,50.7508064960244,-9.62435378625662));
#33658=CARTESIAN_POINT('Ctrl Pts',(-3.7635861295493,52.0000086477592,-9.62320046360554));
#33659=CARTESIAN_POINT('Ctrl Pts',(-1.37301063256245,40.1875259567355,1.47293173916723));
#33660=CARTESIAN_POINT('Ctrl Pts',(-1.4146215988499,40.1634477706497,1.01538079142922));
#33661=CARTESIAN_POINT('Ctrl Pts',(-1.45810560976051,40.1308402311943,0.52858064812525));
#33662=CARTESIAN_POINT('Ctrl Pts',(-1.62620698164421,40.1319542826288,-1.55402875455442));
#33663=CARTESIAN_POINT('Ctrl Pts',(-1.74968648306504,40.4376784663506,-3.10121432123458));
#33664=CARTESIAN_POINT('Ctrl Pts',(-2.00204375396079,41.6310829191854,-5.98129145450958));
#33665=CARTESIAN_POINT('Ctrl Pts',(-2.1256786473503,42.5084456369459,-7.29389406576053));
#33666=CARTESIAN_POINT('Ctrl Pts',(-2.37601161837514,44.7065608867208,-9.49113593804617));
#33667=CARTESIAN_POINT('Ctrl Pts',(-2.49964647926794,46.0177955705498,-10.3708286017073));
#33668=CARTESIAN_POINT('Ctrl Pts',(-2.75200381047716,48.8994560970608,-11.5604045561349));
#33669=CARTESIAN_POINT('Ctrl Pts',(-2.87602039417758,50.4518266808844,-11.8694761541618));
#33670=CARTESIAN_POINT('Ctrl Pts',(-3.00091936260203,51.9999864978575,-11.8687142284813));
#33671=CARTESIAN_POINT('Ctrl Pts',(-1.06226042837003,37.8397258902528,1.59647049649061));
#33672=CARTESIAN_POINT('Ctrl Pts',(-1.1026280281322,37.8163671782172,1.15259151032668));
#33673=CARTESIAN_POINT('Ctrl Pts',(-1.14747953738506,37.7797757625757,0.635572917996464));
#33674=CARTESIAN_POINT('Ctrl Pts',(-1.31732736909556,37.7806592587273,-1.86858636177033));
#33675=CARTESIAN_POINT('Ctrl Pts',(-1.43803115336732,38.1455252315354,-3.71029995869598));
#33676=CARTESIAN_POINT('Ctrl Pts',(-1.69365713820691,39.5779229780087,-7.16936247493924));
#33677=CARTESIAN_POINT('Ctrl Pts',(-1.81514228728896,40.6266263701707,-8.73699595770183));
#33678=CARTESIAN_POINT('Ctrl Pts',(-2.06643737216329,43.2633442117449,-11.373025698218));
#33679=CARTESIAN_POINT('Ctrl Pts',(-2.18792249430954,44.8298904725309,-12.4235805192224));
#33680=CARTESIAN_POINT('Ctrl Pts',(-2.44354852690247,48.2902066278842,-13.85294708216));
#33681=CARTESIAN_POINT('Ctrl Pts',(-2.5649207391089,50.1387215498278,-14.2204718556691));
#33682=CARTESIAN_POINT('Ctrl Pts',(-2.69099156569462,51.9999633056261,-14.2198708430667));
#33683=CARTESIAN_POINT('Ctrl Pts',(1.31891566289574,37.8403157026637,1.59674345384007));
#33684=CARTESIAN_POINT('Ctrl Pts',(1.27856167200497,37.816964865386,1.15301410976406));
#33685=CARTESIAN_POINT('Ctrl Pts',(1.233696642558,37.7802246921785,0.635579023171323));
#33686=CARTESIAN_POINT('Ctrl Pts',(1.06384881090688,37.7793394042942,-1.86860431100347));
#33687=CARTESIAN_POINT('Ctrl Pts',(0.943145133347893,38.1469172473993,-3.70979114470452));
#33688=CARTESIAN_POINT('Ctrl Pts',(0.687518921089845,39.5762884400051,-7.1701426146911));
#33689=CARTESIAN_POINT('Ctrl Pts',(0.566033915384876,40.6268483631173,-8.73670574475149));
#33690=CARTESIAN_POINT('Ctrl Pts',(0.314738777667144,43.2628954695716,-11.3734544105136));
#33691=CARTESIAN_POINT('Ctrl Pts',(0.193253748290465,44.8305401133009,-12.4221714958367));
#33692=CARTESIAN_POINT('Ctrl Pts',(-0.0623724159481351,48.2896308975971,
-13.8545909095489));
#33693=CARTESIAN_POINT('Ctrl Pts',(-0.183762141935176,50.1389656602319,
-14.2195188100007));
#33694=CARTESIAN_POINT('Ctrl Pts',(-0.309815399742848,51.9999633043523,
-14.2201291128083));
#33695=CARTESIAN_POINT('Ctrl Pts',(1.62853105321834,40.1882694324258,1.47327580984132));
#33696=CARTESIAN_POINT('Ctrl Pts',(1.58693724130861,40.1642011727047,1.01591349030511));
#33697=CARTESIAN_POINT('Ctrl Pts',(1.54343618780061,40.1314061200099,0.528588343875644));
#33698=CARTESIAN_POINT('Ctrl Pts',(1.37533481599181,40.1302905677455,-1.55405138008459));
#33699=CARTESIAN_POINT('Ctrl Pts',(1.25185544908535,40.4394331428107,-3.10057294640679));
#33700=CARTESIAN_POINT('Ctrl Pts',(0.99949789152226,41.6290225365179,-5.982274843346));
#33701=CARTESIAN_POINT('Ctrl Pts',(0.875863178863669,42.5087254655101,-7.29352824389351));
#33702=CARTESIAN_POINT('Ctrl Pts',(0.625530141228094,44.7059952341645,-9.49167634236414));
#33703=CARTESIAN_POINT('Ctrl Pts',(0.501895397273555,46.0186144616128,-10.369052486768));
#33704=CARTESIAN_POINT('Ctrl Pts',(0.249537900122171,48.8987303723102,-11.5624766483463));
#33705=CARTESIAN_POINT('Ctrl Pts',(0.12549494483352,50.4521347865942,-11.8682745705925));
#33706=CARTESIAN_POINT('Ctrl Pts',(0.00062241732267218,51.9999864962518,
-11.8690397849987));
#33707=CARTESIAN_POINT('Ctrl Pts',(2.3908994428123,42.4307892712954,1.35541200298501));
#33708=CARTESIAN_POINT('Ctrl Pts',(2.34812421168708,42.4060373833274,0.885058889676137));
#33709=CARTESIAN_POINT('Ctrl Pts',(2.30592316845608,42.3769809488797,0.426408500609331));
#33710=CARTESIAN_POINT('Ctrl Pts',(2.13948974646398,42.3752988308948,-1.2536423221009));
#33711=CARTESIAN_POINT('Ctrl Pts',(2.01335948895661,42.6291645083452,-2.51864171288184));
#33712=CARTESIAN_POINT('Ctrl Pts',(1.76412360301129,43.5891580556313,-4.84795915807201));
#33713=CARTESIAN_POINT('Ctrl Pts',(1.63843584903305,44.306048514286,-5.915170204659));
#33714=CARTESIAN_POINT('Ctrl Pts',(1.38902165105131,46.0841342086093,-7.69457540340395));
#33715=CARTESIAN_POINT('Ctrl Pts',(1.26333384857794,47.1534076509294,-8.40795287035374));
#33716=CARTESIAN_POINT('Ctrl Pts',(1.01409805364822,49.4803356664615,-9.37372383743554));
#33717=CARTESIAN_POINT('Ctrl Pts',(0.887523067773743,50.7512717901712,-9.62254086006318));
#33718=CARTESIAN_POINT('Ctrl Pts',(0.763776277074716,52.0000086453373,-9.62369151535372));
#33719=CARTESIAN_POINT('Ctrl Pts',(3.57672261477347,44.4816940061638,1.24768160116189));
#33720=CARTESIAN_POINT('Ctrl Pts',(3.532869768796,44.4563185563517,0.765479118782403));
#33721=CARTESIAN_POINT('Ctrl Pts',(3.49185481010396,44.4306505608144,0.332966318319628));
#33722=CARTESIAN_POINT('Ctrl Pts',(3.32694672771567,44.4280873491762,-0.978922014648203));
#33723=CARTESIAN_POINT('Ctrl Pts',(3.19839225347182,44.631958819594,-1.98636136652616));
#33724=CARTESIAN_POINT('Ctrl Pts',(2.95201108858767,45.3813659616981,-3.81078790535049));
#33725=CARTESIAN_POINT('Ctrl Pts',(2.82444585837898,45.9497454423788,-4.65460264912874));
#33726=CARTESIAN_POINT('Ctrl Pts',(2.57587192813369,47.3443497895988,-6.05121512490362));
#33727=CARTESIAN_POINT('Ctrl Pts',(2.44830662331527,48.1913089840266,-6.61423873300174));
#33728=CARTESIAN_POINT('Ctrl Pts',(2.20192559708917,50.0120953836876,-7.37244739486218));
#33729=CARTESIAN_POINT('Ctrl Pts',(2.07303718495312,51.024880382195,-7.56862230180471));
#33730=CARTESIAN_POINT('Ctrl Pts',(1.95031777657921,52.0000289004077,-7.57037421505985));
#33731=CARTESIAN_POINT('Ctrl Pts',(4.33370633274505,37.6057474666452,1.59647061166167));
#33732=CARTESIAN_POINT('Ctrl Pts',(4.29042532206453,37.588371419626,1.15259158904763));
#33733=CARTESIAN_POINT('Ctrl Pts',(4.2408228309336,37.5585354835147,0.635572970243792));
#33734=CARTESIAN_POINT('Ctrl Pts',(4.07282953636148,37.5835818541665,-1.86858636171414));
#33735=CARTESIAN_POINT('Ctrl Pts',(4.00528018450669,37.9619119569889,-3.71029995870983));
#33736=CARTESIAN_POINT('Ctrl Pts',(3.95610755718974,39.4161093304775,-7.16936247492528));
#33737=CARTESIAN_POINT('Ctrl Pts',(3.98510500545029,40.4714275735081,-8.73699595768472));
#33738=CARTESIAN_POINT('Ctrl Pts',(4.11161181537177,43.1170704487122,-11.3730256982351));
#33739=CARTESIAN_POINT('Ctrl Pts',(4.21430601437353,44.6849606628027,-12.423580519233));
#33740=CARTESIAN_POINT('Ctrl Pts',(4.45373622021968,48.1464351665736,-13.8529470821494));
#33741=CARTESIAN_POINT('Ctrl Pts',(4.59667050422672,49.9934079386823,-14.2204718556644));
#33742=CARTESIAN_POINT('Ctrl Pts',(4.73676521641214,51.8536466863969,-14.2198708430668));
#33743=CARTESIAN_POINT('Ctrl Pts',(4.9514291922416,36.8815114147052,1.6296460532693));
#33744=CARTESIAN_POINT('Ctrl Pts',(4.90850926387593,36.8642803315734,1.1894701989116));
#33745=CARTESIAN_POINT('Ctrl Pts',(4.85838298962156,36.8334013785589,0.664243924996268));
#33746=CARTESIAN_POINT('Ctrl Pts',(4.68985095932913,36.8579890764766,-1.95287905120227));
#33747=CARTESIAN_POINT('Ctrl Pts',(4.62539547711762,37.252611065952,-3.87337387079324));
#33748=CARTESIAN_POINT('Ctrl Pts',(4.58435548147172,38.7695270469185,-7.48792130213237));
#33749=CARTESIAN_POINT('Ctrl Pts',(4.62052713521612,39.8706950784794,-9.12360836229799));
#33750=CARTESIAN_POINT('Ctrl Pts',(4.76347923307348,42.6325290552246,-11.8774049927332));
#33751=CARTESIAN_POINT('Ctrl Pts',(4.87652118891077,44.2683416970959,-12.9732563608876));
#33752=CARTESIAN_POINT('Ctrl Pts',(5.13710478162637,47.8830959478414,-14.4676858045473));
#33753=CARTESIAN_POINT('Ctrl Pts',(5.29206142838226,49.8087293766846,-14.8501851005056));
#33754=CARTESIAN_POINT('Ctrl Pts',(5.44377846349978,51.7519872491301,-14.8499483202528));
#33755=CARTESIAN_POINT('Ctrl Pts',(5.89423842867639,36.7461942621622,1.62975523620908));
#33756=CARTESIAN_POINT('Ctrl Pts',(5.85132433673285,36.7289655221871,1.18963923869757));
#33757=CARTESIAN_POINT('Ctrl Pts',(5.80118424128265,36.6980284414522,0.664246367065471));
#33758=CARTESIAN_POINT('Ctrl Pts',(5.6325515213262,36.7219158272082,-1.95288623089274));
#33759=CARTESIAN_POINT('Ctrl Pts',(5.56825045711999,37.117611517565,-3.87317034519377));
#33760=CARTESIAN_POINT('Ctrl Pts',(5.52703808201953,38.6333292122907,-7.48823335803598));
#33761=CARTESIAN_POINT('Ctrl Pts',(5.56331547729456,39.7352322893592,-9.12349227711209));
#33762=CARTESIAN_POINT('Ctrl Pts',(5.70622937200357,42.4968007059074,-11.8775764776571));
#33763=CARTESIAN_POINT('Ctrl Pts',(5.81933389104879,44.1330482236871,-12.9726927515247));
#33764=CARTESIAN_POINT('Ctrl Pts',(6.07984767624782,47.7473173225239,-14.4683433355115));
#33765=CARTESIAN_POINT('Ctrl Pts',(6.23484434203113,49.6732762742259,-14.8498038985576));
#33766=CARTESIAN_POINT('Ctrl Pts',(6.38655415380922,51.6164365682427,-14.8500516281495));
#33767=CARTESIAN_POINT('Ctrl Pts',(6.69072942383202,37.2674545852876,1.59674356901112));
#33768=CARTESIAN_POINT('Ctrl Pts',(6.64746300420534,37.2500843961589,1.15301418851277));
#33769=CARTESIAN_POINT('Ctrl Pts',(6.59782596008604,37.2201031407487,0.635579075416795));
#33770=CARTESIAN_POINT('Ctrl Pts',(6.42958094135504,37.2433987309931,-1.86860431094034));
#33771=CARTESIAN_POINT('Ctrl Pts',(6.36241763451085,37.6244130860142,-3.70979114470994));
#33772=CARTESIAN_POINT('Ctrl Pts',(6.31281405856107,39.0756147439152,-7.1701426146855));
#33773=CARTESIAN_POINT('Ctrl Pts',(6.34207586064458,40.1327706007196,-8.73670574472715));
#33774=CARTESIAN_POINT('Ctrl Pts',(6.46848716269878,42.7777495754072,-11.3734544105378));
#33775=CARTESIAN_POINT('Ctrl Pts',(6.57133776971646,44.3467269792927,-12.4221714958377));
#33776=CARTESIAN_POINT('Ctrl Pts',(6.8105934567754,47.806988603268,-13.8545909095479));
#33777=CARTESIAN_POINT('Ctrl Pts',(6.95362708075977,49.6547753637287,-14.2195188100197));
#33778=CARTESIAN_POINT('Ctrl Pts',(7.09370444218574,51.5147699841784,-14.2201291128083));
#33779=CARTESIAN_POINT('Ctrl Pts',(4.19818497005567,37.5648924257371,0.));
#33780=CARTESIAN_POINT('Ctrl Pts',(4.07282953636148,37.5835818541665,-1.86858636171414));
#33781=CARTESIAN_POINT('Ctrl Pts',(4.00528018450669,37.9619119569889,-3.71029995870983));
#33782=CARTESIAN_POINT('Ctrl Pts',(3.95610755718974,39.4161093304775,-7.16936247492528));
#33783=CARTESIAN_POINT('Ctrl Pts',(3.98510500545029,40.4714275735081,-8.73699595768472));
#33784=CARTESIAN_POINT('Ctrl Pts',(4.05479285274666,41.9288128067805,-10.1890856763504));
#33785=CARTESIAN_POINT('Ctrl Pts',(4.06163542615305,42.0659125600701,-10.3203928635173));
#33786=CARTESIAN_POINT('Ctrl Pts',(4.06886253049489,42.2054617208602,-10.4488603766));
#33787=CARTESIAN_POINT('Ctrl Pts',(6.55512420987433,37.2260157227862,1.49880108324396E-15));
#33788=CARTESIAN_POINT('Ctrl Pts',(6.42958094135504,37.2433987309931,-1.86860431094034));
#33789=CARTESIAN_POINT('Ctrl Pts',(6.36241763451085,37.6244130860142,-3.70979114470994));
#33790=CARTESIAN_POINT('Ctrl Pts',(6.31281405856107,39.0756147439152,-7.1701426146855));
#33791=CARTESIAN_POINT('Ctrl Pts',(6.34207586064458,40.1327706007196,-8.73670574472715));
#33792=CARTESIAN_POINT('Ctrl Pts',(6.41206653251571,41.5972271209445,-10.1966053555726));
#33793=CARTESIAN_POINT('Ctrl Pts',(6.41930840847768,41.7420345975434,-10.3350231942287));
#33794=CARTESIAN_POINT('Ctrl Pts',(6.42697885113783,41.8895769551519,-10.470255845101));
#33795=CARTESIAN_POINT('Ctrl Pts',(3.04071090848719,44.5001944306519,1.24689076028073));
#33796=CARTESIAN_POINT('Ctrl Pts',(2.99365083345139,44.4813012009376,0.764254616115602));
#33797=CARTESIAN_POINT('Ctrl Pts',(2.94950053246457,44.4621525981064,0.332948654593303));
#33798=CARTESIAN_POINT('Ctrl Pts',(2.78663561816042,44.488157628525,-0.978870002740165));
#33799=CARTESIAN_POINT('Ctrl Pts',(2.68728492513176,44.7004709588125,-1.98783577089924));
#33800=CARTESIAN_POINT('Ctrl Pts',(2.5513120932872,45.4859946801884,-3.808527272826));
#33801=CARTESIAN_POINT('Ctrl Pts',(2.5051681016477,46.0614183982245,-4.65544360722295));
#33802=CARTESIAN_POINT('Ctrl Pts',(2.45787394353962,47.4791272455719,-6.04997283343073));
#33803=CARTESIAN_POINT('Ctrl Pts',(2.45168870251787,48.3324696724334,-6.61832169901082));
#33804=CARTESIAN_POINT('Ctrl Pts',(2.4674461098152,50.1733013631196,-7.36768403080617));
#33805=CARTESIAN_POINT('Ctrl Pts',(2.48375959427411,51.191753301279,-7.57138648675178));
#33806=CARTESIAN_POINT('Ctrl Pts',(2.50107414862808,52.1751568070596,-7.56962581969456));
#33807=CARTESIAN_POINT('Ctrl Pts',(3.92365461890876,42.3018453782487,1.35489314066083));
#33808=CARTESIAN_POINT('Ctrl Pts',(3.87776447109268,42.2834218397552,0.8842554720871));
#33809=CARTESIAN_POINT('Ctrl Pts',(3.83192350390653,42.2609432866046,0.426396927835306));
#33810=CARTESIAN_POINT('Ctrl Pts',(3.66742334692479,42.286293018581,-1.2536081950185));
#33811=CARTESIAN_POINT('Ctrl Pts',(3.57797177380375,42.5504213117328,-2.51960912780668));
#33812=CARTESIAN_POINT('Ctrl Pts',(3.46871344470325,43.5418092681868,-4.84647586781428));
#33813=CARTESIAN_POINT('Ctrl Pts',(3.44582654101155,44.2657961681553,-5.91572199046192));
#33814=CARTESIAN_POINT('Ctrl Pts',(3.45218058837109,46.0625411381523,-7.69376028692537));
#33815=CARTESIAN_POINT('Ctrl Pts',(3.47964820283096,47.1367510692278,-8.41063186556218));
#33816=CARTESIAN_POINT('Ctrl Pts',(3.56443746806616,49.4777703293277,-9.37059840620427));
#33817=CARTESIAN_POINT('Ctrl Pts',(3.61985039974726,50.7522326212106,-9.62435378621384));
#33818=CARTESIAN_POINT('Ctrl Pts',(3.67509457152212,52.0063376889004,-9.6232004636056));
#33819=CARTESIAN_POINT('Ctrl Pts',(4.36024590432577,39.9738746787522,1.47293185433834));
#33820=CARTESIAN_POINT('Ctrl Pts',(4.31563179085076,39.9559634303423,1.01538086898097));
#33821=CARTESIAN_POINT('Ctrl Pts',(4.26794984367479,39.9298762050513,0.528580691590028));
#33822=CARTESIAN_POINT('Ctrl Pts',(4.10171804395774,39.9549022371194,-1.55402875454521));
#33823=CARTESIAN_POINT('Ctrl Pts',(4.0230044735859,40.2750875547253,-3.10121432124596));
#33824=CARTESIAN_POINT('Ctrl Pts',(3.943054997525,41.4922590552153,-5.98129145449819));
#33825=CARTESIAN_POINT('Ctrl Pts',(3.94554026237911,42.3782865653749,-7.29389406574829));
#33826=CARTESIAN_POINT('Ctrl Pts',(4.01057973631905,44.5896542676588,-9.49113593805846));
#33827=CARTESIAN_POINT('Ctrl Pts',(4.07481145201547,45.9051375482497,-10.3708286017178));
#33828=CARTESIAN_POINT('Ctrl Pts',(4.2351258063561,48.7933811184128,-11.5604045561245));
#33829=CARTESIAN_POINT('Ctrl Pts',(4.33329690121476,50.3476002080609,-11.8694761541191));
#33830=CARTESIAN_POINT('Ctrl Pts',(4.42999533819688,51.8977769668582,-11.8687142284813));
#33831=CARTESIAN_POINT('Ctrl Pts',(4.33370633274505,37.6057474666452,1.59647061166167));
#33832=CARTESIAN_POINT('Ctrl Pts',(4.29042532206453,37.588371419626,1.15259158904763));
#33833=CARTESIAN_POINT('Ctrl Pts',(4.2408228309336,37.5585354835147,0.635572970243792));
#33834=CARTESIAN_POINT('Ctrl Pts',(4.07282953636148,37.5835818541665,-1.86858636171414));
#33835=CARTESIAN_POINT('Ctrl Pts',(4.00528018450669,37.9619119569889,-3.71029995870983));
#33836=CARTESIAN_POINT('Ctrl Pts',(3.95610755718974,39.4161093304775,-7.16936247492528));
#33837=CARTESIAN_POINT('Ctrl Pts',(3.98510500545029,40.4714275735081,-8.73699595768472));
#33838=CARTESIAN_POINT('Ctrl Pts',(4.11161181537177,43.1170704487122,-11.3730256982351));
#33839=CARTESIAN_POINT('Ctrl Pts',(4.21430601437353,44.6849606628027,-12.423580519233));
#33840=CARTESIAN_POINT('Ctrl Pts',(4.45373622021968,48.1464351665736,-13.8529470821494));
#33841=CARTESIAN_POINT('Ctrl Pts',(4.59667050422672,49.9934079386823,-14.2204718556644));
#33842=CARTESIAN_POINT('Ctrl Pts',(4.73676521641214,51.8536466863969,-14.2198708430668));
#33843=CARTESIAN_POINT('Ctrl Pts',(6.69072942383202,37.2674545852876,1.59674356901112));
#33844=CARTESIAN_POINT('Ctrl Pts',(6.64746300420528,37.2500843961589,1.15301418851278));
#33845=CARTESIAN_POINT('Ctrl Pts',(6.59782596008604,37.2201031407487,0.635579075416795));
#33846=CARTESIAN_POINT('Ctrl Pts',(6.42958094135505,37.2433987309931,-1.86860431094034));
#33847=CARTESIAN_POINT('Ctrl Pts',(6.36241763451087,37.6244130860142,-3.70979114471114));
#33848=CARTESIAN_POINT('Ctrl Pts',(6.31281405856107,39.0756147439152,-7.1701426146843));
#33849=CARTESIAN_POINT('Ctrl Pts',(6.34207586064459,40.1327706007148,-8.73670574472715));
#33850=CARTESIAN_POINT('Ctrl Pts',(6.46848716269878,42.777749575412,-11.3734544105378));
#33851=CARTESIAN_POINT('Ctrl Pts',(6.57133776971646,44.3467269792927,-12.4221714958329));
#33852=CARTESIAN_POINT('Ctrl Pts',(6.8105934567754,47.806988603268,-13.8545909095527));
#33853=CARTESIAN_POINT('Ctrl Pts',(6.95362708075977,49.6547753637287,-14.2195188100198));
#33854=CARTESIAN_POINT('Ctrl Pts',(7.09370444218574,51.5147699841784,-14.2201291128083));
#33855=CARTESIAN_POINT('Ctrl Pts',(7.33134203123371,39.5474466673498,1.47327592501241));
#33856=CARTESIAN_POINT('Ctrl Pts',(7.28674631020699,39.5295428029873,1.01591356789178));
#33857=CARTESIAN_POINT('Ctrl Pts',(7.23902080798441,39.5032723984885,0.528588387338081));
#33858=CARTESIAN_POINT('Ctrl Pts',(7.07247170264534,39.526091520959,-1.55405138006663));
#33859=CARTESIAN_POINT('Ctrl Pts',(6.99424475323468,39.8496604164912,-3.10057294640973));
#33860=CARTESIAN_POINT('Ctrl Pts',(6.91375205389164,41.0630557303986,-5.98227484334297));
#33861=CARTESIAN_POINT('Ctrl Pts',(6.91657054442664,41.9513996061356,-7.29352824387643));
#33862=CARTESIAN_POINT('Ctrl Pts',(6.98148962792165,44.1619304425256,-9.49167634238116));
#33863=CARTESIAN_POINT('Ctrl Pts',(7.04591850046981,45.4787841574542,-10.369052486764));
#33864=CARTESIAN_POINT('Ctrl Pts',(7.20601286880595,48.365498857377,-11.5624766483503));
#33865=CARTESIAN_POINT('Ctrl Pts',(7.30430498991546,49.9207450076545,-11.8682745706115));
#33866=CARTESIAN_POINT('Ctrl Pts',(7.40098575043927,51.4706130322883,-11.8690397849987));
#33867=CARTESIAN_POINT('Ctrl Pts',(8.40509445805923,41.6586445536367,1.35541211815614));
#33868=CARTESIAN_POINT('Ctrl Pts',(8.35923205241223,41.6402321528243,0.88505896615835));
#33869=CARTESIAN_POINT('Ctrl Pts',(8.31332538916191,41.6174773021325,0.42640853568319));
#33870=CARTESIAN_POINT('Ctrl Pts',(8.14834662563443,41.6394982516744,-1.25364232212472));
#33871=CARTESIAN_POINT('Ctrl Pts',(8.05962904511026,41.9087301497828,-2.51864171287991));
#33872=CARTESIAN_POINT('Ctrl Pts',(7.94955134754913,42.8944223117342,-4.84795915807392));
#33873=CARTESIAN_POINT('Ctrl Pts',(7.92716706335442,43.621903091586,-5.91517020464439));
#33874=CARTESIAN_POINT('Ctrl Pts',(7.93333952031455,45.4173857785675,-7.69457540341853));
#33875=CARTESIAN_POINT('Ctrl Pts',(7.96110451544885,46.4936627982892,-8.40795287034961));
#33876=CARTESIAN_POINT('Ctrl Pts',(8.04556196575565,48.8323759936388,-9.37372383743963));
#33877=CARTESIAN_POINT('Ctrl Pts',(8.10114839964667,50.1083893187776,-9.62254086010123));
#33878=CARTESIAN_POINT('Ctrl Pts',(8.15637495641955,51.3620268377998,-9.62369151535369));
#33879=CARTESIAN_POINT('Ctrl Pts',(9.87072183560219,43.5199138025263,1.24768171633307));
#33880=CARTESIAN_POINT('Ctrl Pts',(9.82370404146588,43.5010375473779,0.765479194261124));
#33881=CARTESIAN_POINT('Ctrl Pts',(9.77945361533133,43.4814678488037,0.332966345721785));
#33882=CARTESIAN_POINT('Ctrl Pts',(9.61585927297428,43.5023995944714,-0.978922014708797));
#33883=CARTESIAN_POINT('Ctrl Pts',(9.51762723324188,43.7224911565099,-1.98636136651937));
#33884=CARTESIAN_POINT('Ctrl Pts',(9.3804056296356,44.4993341100647,-3.81078790535733));
#33885=CARTESIAN_POINT('Ctrl Pts',(9.33502766337594,45.080082732299,-4.65460264911418));
#33886=CARTESIAN_POINT('Ctrl Pts',(9.28745674947728,46.4958677767823,-6.05121512491815));
#33887=CARTESIAN_POINT('Ctrl Pts',(9.28172473628772,47.3523605835541,-6.61423873299266));
#33888=CARTESIAN_POINT('Ctrl Pts',(9.29697643567208,49.189677678933,-7.37244739487121));
#33889=CARTESIAN_POINT('Ctrl Pts',(9.31353425504065,50.2104967199909,-7.56862230187133));
#33890=CARTESIAN_POINT('Ctrl Pts',(9.33084205690769,51.1931844250963,-7.57037421505979));
#33891=CARTESIAN_POINT('Ctrl Pts',(9.64145132693361,36.6062244663074,1.59647068126639));
#33892=CARTESIAN_POINT('Ctrl Pts',(9.59613798296502,36.5951848118766,1.15259163662228));
#33893=CARTESIAN_POINT('Ctrl Pts',(9.54279427443722,36.5727117312896,0.63557300182231));
#33894=CARTESIAN_POINT('Ctrl Pts',(9.38007537755078,36.6214111051439,-1.86858636168713));
#33895=CARTESIAN_POINT('Ctrl Pts',(9.36705556809957,37.0055036281237,-3.71029995871696));
#33896=CARTESIAN_POINT('Ctrl Pts',(9.52533731119175,38.4518973636396,-7.16936247491812));
#33897=CARTESIAN_POINT('Ctrl Pts',(9.70422705225016,39.4923472214852,-8.73699595765307));
#33898=CARTESIAN_POINT('Ctrl Pts',(10.2059604433763,42.0930574706308,-11.3730256982666));
#33899=CARTESIAN_POINT('Ctrl Pts',(10.5307434056703,43.6303739147712,-12.4235805192466));
#33900=CARTESIAN_POINT('Ctrl Pts',(11.2603557414003,47.0225411281197,-13.8529470821357));
#33901=CARTESIAN_POINT('Ctrl Pts',(11.6646867918734,48.8303727110007,-14.2204718556644));
#33902=CARTESIAN_POINT('Ctrl Pts',(12.0680951184149,50.6517393542017,-14.2198708430667));
#33903=CARTESIAN_POINT('Ctrl Pts',(10.1498171217998,35.8014489642672,1.629646122874));
#33904=CARTESIAN_POINT('Ctrl Pts',(10.1048818153817,35.7905014108269,1.18947024667978));
#33905=CARTESIAN_POINT('Ctrl Pts',(10.0508712182893,35.7670704718624,0.664243957997926));
#33906=CARTESIAN_POINT('Ctrl Pts',(9.88755379330354,35.8153925116915,-1.95287905116997));
#33907=CARTESIAN_POINT('Ctrl Pts',(9.8799149395762,36.2151707898526,-3.8733738708004));
#33908=CARTESIAN_POINT('Ctrl Pts',(10.055172324341,37.7224873536916,-7.48792130212525));
#33909=CARTESIAN_POINT('Ctrl Pts',(10.2476883530401,38.8072993194235,-9.12360836227592));
#33910=CARTESIAN_POINT('Ctrl Pts',(10.7822353606524,41.5206776037667,-11.8774049927552));
#33911=CARTESIAN_POINT('Ctrl Pts',(11.1269271238415,43.1237524839494,-12.9732563608916));
#33912=CARTESIAN_POINT('Ctrl Pts',(11.8992915178615,46.6646288366373,-14.4676858045432));
#33913=CARTESIAN_POINT('Ctrl Pts',(12.3267171394111,48.5486094635681,-14.8501851005151));
#33914=CARTESIAN_POINT('Ctrl Pts',(12.7534443437026,50.4504961875092,-14.8499483202528));
#33915=CARTESIAN_POINT('Ctrl Pts',(11.0637722809467,35.5333334012201,1.62975530581378));
#33916=CARTESIAN_POINT('Ctrl Pts',(11.0188430850089,35.5223873364705,1.18963928647272));
#33917=CARTESIAN_POINT('Ctrl Pts',(10.9648105349674,35.4989008284142,0.664246400067514));
#33918=CARTESIAN_POINT('Ctrl Pts',(10.801293780378,35.5465440138904,-1.95288623086123));
#33919=CARTESIAN_POINT('Ctrl Pts',(10.7939605764728,35.9473630882236,-3.87317034519856));
#33920=CARTESIAN_POINT('Ctrl Pts',(10.9688768024414,37.4535180947963,-7.48823335803128));
#33921=CARTESIAN_POINT('Ctrl Pts',(11.1616021042532,38.5390425757264,-9.12349227711398));
#33922=CARTESIAN_POINT('Ctrl Pts',(11.6960735044253,41.2521634398075,-11.8775764776553));
#33923=CARTESIAN_POINT('Ctrl Pts',(12.0408890833104,42.8556598657977,-12.9726927515335));
#33924=CARTESIAN_POINT('Ctrl Pts',(12.8131153360331,46.3960659393659,-14.4683433355026));
#33925=CARTESIAN_POINT('Ctrl Pts',(13.2406268960164,48.2803630805025,-14.8498038985528));
#33926=CARTESIAN_POINT('Ctrl Pts',(13.6673330636266,50.1821542472109,-14.8500516281495));
#33927=CARTESIAN_POINT('Ctrl Pts',(11.9263392248006,35.9359355586898,1.59674363861582));
#33928=CARTESIAN_POINT('Ctrl Pts',(11.881041157038,35.9248996259739,1.1530142361046));
#33929=CARTESIAN_POINT('Ctrl Pts',(11.8276425661301,35.9022876226716,0.635579106996277));
#33930=CARTESIAN_POINT('Ctrl Pts',(11.664425345244,35.9492898606342,-1.86860431091527));
#33931=CARTESIAN_POINT('Ctrl Pts',(11.652169660341,36.335984374051,-3.70979114470996));
#33932=CARTESIAN_POINT('Ctrl Pts',(11.8095985064428,37.7794742164015,-7.17014261468561));
#33933=CARTESIAN_POINT('Ctrl Pts',(11.9890114302846,38.8217053622519,-8.73670574474104));
#33934=CARTESIAN_POINT('Ctrl Pts',(12.4905558028067,41.4217720607234,-11.373454410524));
#33935=CARTESIAN_POINT('Ctrl Pts',(12.8156483043377,42.9601423694015,-12.422171495837));
#33936=CARTESIAN_POINT('Ctrl Pts',(13.544915286834,46.3511338849317,-13.8545909095487));
#33937=CARTESIAN_POINT('Ctrl Pts',(13.9494605087747,48.1597570333862,-14.2195188100198));
#33938=CARTESIAN_POINT('Ctrl Pts',(14.3528169182251,49.980884503456,-14.2201291128084));
#33939=CARTESIAN_POINT('Ctrl Pts',(9.50149509066547,36.5850719698904,1.04083408558608E-14));
#33940=CARTESIAN_POINT('Ctrl Pts',(9.38007537755078,36.6214111051439,-1.86858636168712));
#33941=CARTESIAN_POINT('Ctrl Pts',(9.36705556810076,37.0055036281238,-3.71029995871695));
#33942=CARTESIAN_POINT('Ctrl Pts',(9.52533731119055,38.4518973636396,-7.16936247491812));
#33943=CARTESIAN_POINT('Ctrl Pts',(9.70422705225135,39.4923472214804,-8.73699595765307));
#33944=CARTESIAN_POINT('Ctrl Pts',(9.98061312163222,40.924980759688,-10.189085676353));
#33945=CARTESIAN_POINT('Ctrl Pts',(10.0068973767326,41.0597112354387,-10.320392863522));
#33946=CARTESIAN_POINT('Ctrl Pts',(10.0339108358286,41.1968114627961,-10.4488603766063));
#33947=CARTESIAN_POINT('Ctrl Pts',(11.7862169042735,35.9142171164209,-6.66133814775094E-16));
#33948=CARTESIAN_POINT('Ctrl Pts',(11.664425345244,35.9492898606342,-1.86860431091527));
#33949=CARTESIAN_POINT('Ctrl Pts',(11.652169660341,36.335984374051,-3.70979114470996));
#33950=CARTESIAN_POINT('Ctrl Pts',(11.8095985064428,37.7794742164015,-7.17014261468561));
#33951=CARTESIAN_POINT('Ctrl Pts',(11.9890114302846,38.8217053622519,-8.73670574474104));
#33952=CARTESIAN_POINT('Ctrl Pts',(12.2667035909977,40.2612951155291,-10.1966053555703));
#33953=CARTESIAN_POINT('Ctrl Pts',(12.2944800077272,40.4035980344044,-10.3350231942244));
#33954=CARTESIAN_POINT('Ctrl Pts',(12.3230698431103,40.5485470057436,-10.470255845095));
#33955=CARTESIAN_POINT('Ctrl Pts',(9.34279883641518,43.6145083358835,1.24689082988549));
#33956=CARTESIAN_POINT('Ctrl Pts',(9.29352897570236,43.6025047583975,0.764254661684727));
#33957=CARTESIAN_POINT('Ctrl Pts',(9.24710292815239,43.5898343019112,0.33294867115195));
#33958=CARTESIAN_POINT('Ctrl Pts',(9.08959664351103,43.6387527331524,-0.978870002773219));
#33959=CARTESIAN_POINT('Ctrl Pts',(9.02147253455122,43.8630440976867,-1.98783577090387));
#33960=CARTESIAN_POINT('Ctrl Pts',(8.99867539150743,44.6599232717994,-3.80852727282109));
#33961=CARTESIAN_POINT('Ctrl Pts',(9.03489241262212,45.2360569808332,-4.65544360715076));
#33962=CARTESIAN_POINT('Ctrl Pts',(9.18984064595293,46.6460662566343,-6.04997283350261));
#33963=CARTESIAN_POINT('Ctrl Pts',(9.30516165133522,47.4916031396421,-6.61832169903423));
#33964=CARTESIAN_POINT('Ctrl Pts',(9.58273633532526,49.3114553051003,-7.3676840307824));
#33965=CARTESIAN_POINT('Ctrl Pts',(9.74382459487429,50.3172192201186,-7.57138648675638));
#33966=CARTESIAN_POINT('Ctrl Pts',(9.90091582292632,51.2881489781559,-7.56962581969435));
#33967=CARTESIAN_POINT('Ctrl Pts',(9.90389776310351,41.3128793157232,1.35489321026558));
#33968=CARTESIAN_POINT('Ctrl Pts',(9.85585276553219,41.3011741506697,0.884255518279171));
#33969=CARTESIAN_POINT('Ctrl Pts',(9.80727935893699,41.2854482448526,0.426396949032127));
#33970=CARTESIAN_POINT('Ctrl Pts',(9.64806121734291,41.3339507669448,-1.25360819503341));
#33971=CARTESIAN_POINT('Ctrl Pts',(9.59710950758293,41.6081209010766,-2.51960912781136));
#33972=CARTESIAN_POINT('Ctrl Pts',(9.63005248744851,42.6049670390508,-4.84647586780943));
#33973=CARTESIAN_POINT('Ctrl Pts',(9.71043261804921,43.3248419422994,-5.91572199041364));
#33974=CARTESIAN_POINT('Ctrl Pts',(9.97242546010331,45.1023943639113,-7.69376028697345));
#33975=CARTESIAN_POINT('Ctrl Pts',(10.1524895065065,46.1617613376918,-8.41063186557115));
#33976=CARTESIAN_POINT('Ctrl Pts',(10.56957751668,48.4668856266258,-9.37059840619505));
#33977=CARTESIAN_POINT('Ctrl Pts',(10.8058013195624,49.72048964759,-9.62435378622801));
#33978=CARTESIAN_POINT('Ctrl Pts',(11.0389609452146,50.9539676685888,-9.62320046360545));
#33979=CARTESIAN_POINT('Ctrl Pts',(10.004740405144,38.9464705831154,1.47293192394307));
#33980=CARTESIAN_POINT('Ctrl Pts',(9.95803136027274,38.9350908951691,1.01538091585011));
#33981=CARTESIAN_POINT('Ctrl Pts',(9.90712214456362,38.9160550470416,0.528580717858437));
#33982=CARTESIAN_POINT('Ctrl Pts',(9.74614391856815,38.9644836024815,-1.55402875453983));
#33983=CARTESIAN_POINT('Ctrl Pts',(9.71379866054205,39.2926120042599,-3.10121432125187));
#33984=CARTESIAN_POINT('Ctrl Pts',(9.80788452009142,40.5087724506632,-5.98129145449219));
#33985=CARTESIAN_POINT('Ctrl Pts',(9.93643935032803,41.3854277882792,-7.29389406570713));
#33986=CARTESIAN_POINT('Ctrl Pts',(10.3155272531748,43.5650308735924,-9.49113593809946));
#33987=CARTESIAN_POINT('Ctrl Pts',(10.5663179729254,44.857983304954,-10.3708286017267));
#33988=CARTESIAN_POINT('Ctrl Pts',(11.1360404748616,47.694013608684,-11.5604045561154));
#33989=CARTESIAN_POINT('Ctrl Pts',(11.4544007679174,49.218441785495,-11.8694761541142));
#33990=CARTESIAN_POINT('Ctrl Pts',(11.7707281089612,50.7390783576437,-11.8687142284812));
#33991=CARTESIAN_POINT('Ctrl Pts',(9.64145132693361,36.6062244663074,1.59647068126639));
#33992=CARTESIAN_POINT('Ctrl Pts',(9.59613798296502,36.5951848118766,1.15259163662228));
#33993=CARTESIAN_POINT('Ctrl Pts',(9.5427942744372,36.5727117312896,0.63557300182231));
#33994=CARTESIAN_POINT('Ctrl Pts',(9.38007537755078,36.6214111051439,-1.86858636168713));
#33995=CARTESIAN_POINT('Ctrl Pts',(9.36705556810076,37.0055036281238,-3.71029995871696));
#33996=CARTESIAN_POINT('Ctrl Pts',(9.52533731119055,38.4518973636396,-7.16936247491812));
#33997=CARTESIAN_POINT('Ctrl Pts',(9.70422705225135,39.4923472214804,-8.73699595765307));
#33998=CARTESIAN_POINT('Ctrl Pts',(10.2059604433751,42.0930574706355,-11.3730256982666));
#33999=CARTESIAN_POINT('Ctrl Pts',(10.5307434056679,43.6303739147712,-12.4235805192466));
#34000=CARTESIAN_POINT('Ctrl Pts',(11.2603557414027,47.0225411281197,-13.8529470821357));
#34001=CARTESIAN_POINT('Ctrl Pts',(11.6646867918773,48.8303727109994,-14.2204718556643));
#34002=CARTESIAN_POINT('Ctrl Pts',(12.0680951184149,50.6517393542017,-14.2198708430667));
#34003=CARTESIAN_POINT('Ctrl Pts',(11.9263392248006,35.9359355586898,1.59674363861582));
#34004=CARTESIAN_POINT('Ctrl Pts',(11.881041157038,35.9248996259739,1.1530142361046));
#34005=CARTESIAN_POINT('Ctrl Pts',(11.8276425661301,35.9022876226716,0.635579106996277));
#34006=CARTESIAN_POINT('Ctrl Pts',(11.664425345244,35.9492898606342,-1.86860431091527));
#34007=CARTESIAN_POINT('Ctrl Pts',(11.652169660341,36.335984374051,-3.70979114470996));
#34008=CARTESIAN_POINT('Ctrl Pts',(11.8095985064428,37.7794742164015,-7.17014261468561));
#34009=CARTESIAN_POINT('Ctrl Pts',(11.9890114302846,38.8217053622519,-8.73670574474104));
#34010=CARTESIAN_POINT('Ctrl Pts',(12.4905558028067,41.4217720607234,-11.373454410524));
#34011=CARTESIAN_POINT('Ctrl Pts',(12.8156483043377,42.9601423694015,-12.422171495837));
#34012=CARTESIAN_POINT('Ctrl Pts',(13.544915286834,46.3511338849317,-13.8545909095487));
#34013=CARTESIAN_POINT('Ctrl Pts',(13.9494605087747,48.1597570333862,-14.2195188100198));
#34014=CARTESIAN_POINT('Ctrl Pts',(14.3528169182251,49.980884503456,-14.2201291128084));
#34015=CARTESIAN_POINT('Ctrl Pts',(12.884908023969,38.1015519292155,1.47327599461714));
#34016=CARTESIAN_POINT('Ctrl Pts',(12.8382182352008,38.0901769325995,1.01591361478258));
#34017=CARTESIAN_POINT('Ctrl Pts',(12.7872398386552,38.0709659683536,0.528588413607706));
#34018=CARTESIAN_POINT('Ctrl Pts',(12.6256334607693,38.1172552346519,-1.5540513800637));
#34019=CARTESIAN_POINT('Ctrl Pts',(12.5942514039498,38.4486635210362,-3.10057294640495));
#34020=CARTESIAN_POINT('Ctrl Pts',(12.687262162052,39.6611635256693,-5.98227484334785));
#34021=CARTESIAN_POINT('Ctrl Pts',(12.8164764793945,40.5400642286032,-7.29352824390238));
#34022=CARTESIAN_POINT('Ctrl Pts',(13.1953261187963,42.7188560995912,-9.4916763423553));
#34023=CARTESIAN_POINT('Ctrl Pts',(13.4465070217538,44.0131369578426,-10.3690524867682));
#34024=CARTESIAN_POINT('Ctrl Pts',(14.0157941958988,46.8476852602796,-11.5624766483461));
#34025=CARTESIAN_POINT('Ctrl Pts',(14.334420449299,48.3731128199111,-11.8682745706068));
#34026=CARTESIAN_POINT('Ctrl Pts',(14.6506863563569,49.8934463159785,-11.8690397849987));
#34027=CARTESIAN_POINT('Ctrl Pts',(14.2481859850623,40.0384499621469,1.35541218776088));
#34028=CARTESIAN_POINT('Ctrl Pts',(14.2001700323452,40.0267518732536,0.885059012382522));
#34029=CARTESIAN_POINT('Ctrl Pts',(14.1514922771427,40.0107618317912,0.426408556881842));
#34030=CARTESIAN_POINT('Ctrl Pts',(13.9913266653942,40.0560375664774,-1.25364232214331));
#34031=CARTESIAN_POINT('Ctrl Pts',(13.9418277959592,40.3351549001892,-2.51864171286796));
#34032=CARTESIAN_POINT('Ctrl Pts',(13.9731491512604,41.3264798268487,-4.847959158086));
#34033=CARTESIAN_POINT('Ctrl Pts',(14.0545240163496,42.0497415170473,-5.91517020468957));
#34034=CARTESIAN_POINT('Ctrl Pts',(14.3161574747839,43.8260703470736,-7.69457540337348));
#34035=CARTESIAN_POINT('Ctrl Pts',(14.496810052318,44.8874410477419,-8.40795287034439));
#34036=CARTESIAN_POINT('Ctrl Pts',(14.9132414377212,47.1903299665148,-9.37372383744498));
#34037=CARTESIAN_POINT('Ctrl Pts',(15.1498577118613,48.4454445415257,-9.62254086010132));
#34038=CARTESIAN_POINT('Ctrl Pts',(15.3829333626944,49.678462279699,-9.62369151535379));
#34039=CARTESIAN_POINT('Ctrl Pts',(15.9637816213007,41.6721936506076,1.24768178593782));
#34040=CARTESIAN_POINT('Ctrl Pts',(15.9145560268702,41.6602008576429,0.765479239879168));
#34041=CARTESIAN_POINT('Ctrl Pts',(15.867970945133,41.6471278409651,0.332966362283221));
#34042=CARTESIAN_POINT('Ctrl Pts',(15.7090206532706,41.6911284346328,-0.978922014747478));
#34043=CARTESIAN_POINT('Ctrl Pts',(15.6431107691165,41.9229596587602,-1.98636136649785));
#34044=CARTESIAN_POINT('Ctrl Pts',(15.617842162917,42.7114241414042,-3.81078790537901));
#34045=CARTESIAN_POINT('Ctrl Pts',(15.6555752252284,43.2927195379046,-4.6546026491858));
#34046=CARTESIAN_POINT('Ctrl Pts',(15.8099757341297,44.700863979149,-6.05121512484675));
#34047=CARTESIAN_POINT('Ctrl Pts',(15.9261936999128,45.5494546745556,-6.6142387329828));
#34048=CARTESIAN_POINT('Ctrl Pts',(16.2027676442909,47.3658999879282,-7.37244739488131));
#34049=CARTESIAN_POINT('Ctrl Pts',(16.3644346256526,48.373972139694,-7.568622301862));
#34050=CARTESIAN_POINT('Ctrl Pts',(16.5214173008838,49.3441943438429,-7.57037421505997));
#34051=CARTESIAN_POINT('Ctrl Pts',(14.7529241788871,34.8615042977019,1.59647077610305));
#34052=CARTESIAN_POINT('Ctrl Pts',(14.7414705295773,34.8603993451984,1.48695587718898));
#34053=CARTESIAN_POINT('Ctrl Pts',(14.7300185573965,34.8592949433739,1.37746402257732));
#34054=CARTESIAN_POINT('Ctrl Pts',(14.6812048800314,34.8545841497086,0.910698635115021));
#34055=CARTESIAN_POINT('Ctrl Pts',(14.6413232655056,34.8466226370598,0.486448413022977));
#34056=CARTESIAN_POINT('Ctrl Pts',(14.4963699339431,34.9137340334406,-1.86858636180158));
#34057=CARTESIAN_POINT('Ctrl Pts',(14.5381447126007,35.295769960475,-3.71029995870877));
#34058=CARTESIAN_POINT('Ctrl Pts',(14.9006586664256,36.7049156525685,-7.1693624749265));
#34059=CARTESIAN_POINT('Ctrl Pts',(15.2257990211744,37.7093165664604,-8.73699595770112));
#34060=CARTESIAN_POINT('Ctrl Pts',(16.092545148085,40.2121512288987,-11.3730256982186));
#34061=CARTESIAN_POINT('Ctrl Pts',(16.6328052294138,41.6875985734161,-12.4235805192612));
#34062=CARTESIAN_POINT('Ctrl Pts',(17.8377468918407,44.9414037541357,-13.852947082121));
#34063=CARTESIAN_POINT('Ctrl Pts',(18.4952436947549,46.6732919100289,-14.2204718556643));
#34064=CARTESIAN_POINT('Ctrl Pts',(19.1537534053194,48.4187086763094,-14.2198708430666));
#34065=CARTESIAN_POINT('Ctrl Pts',(15.1415840475454,33.9925722540019,1.62964621771062));
#34066=CARTESIAN_POINT('Ctrl Pts',(15.1301302752951,33.9914672896363,1.52013014329455));
#34067=CARTESIAN_POINT('Ctrl Pts',(15.1186784705797,33.9903629797961,1.41064104113887));
#34068=CARTESIAN_POINT('Ctrl Pts',(15.0698646034485,33.985651844648,0.943868932657884));
#34069=CARTESIAN_POINT('Ctrl Pts',(15.0295355352143,33.9768575866064,0.50839229845091));
#34070=CARTESIAN_POINT('Ctrl Pts',(14.8839745453764,34.0436978384353,-1.95287905129925));
#34071=CARTESIAN_POINT('Ctrl Pts',(14.9333078250828,34.440494072426,-3.873373870797));
#34072=CARTESIAN_POINT('Ctrl Pts',(15.3212948555137,35.9075266005885,-7.48792130212892));
#34073=CARTESIAN_POINT('Ctrl Pts',(15.666236188169,36.9538988571697,-9.12360836230967));
#34074=CARTESIAN_POINT('Ctrl Pts',(16.5814962694078,39.5635848921074,-11.8774049927216));
#34075=CARTESIAN_POINT('Ctrl Pts',(17.1508209099836,41.1012880288429,-12.9732563609015));
#34076=CARTESIAN_POINT('Ctrl Pts',(18.4192429934717,44.4962044520163,-14.4676858045334));
#34077=CARTESIAN_POINT('Ctrl Pts',(19.1104364369632,46.3001798643402,-14.8501851004961));
#34078=CARTESIAN_POINT('Ctrl Pts',(19.8034868749641,48.1219785107276,-14.8499483202528));
#34079=CARTESIAN_POINT('Ctrl Pts',(16.0080796379931,33.597116340133,1.62975540065037));
#34080=CARTESIAN_POINT('Ctrl Pts',(15.9966258649005,33.5960113756869,1.52023931818545));
#34081=CARTESIAN_POINT('Ctrl Pts',(15.9851740659138,33.5949070766372,1.41075023429468));
#34082=CARTESIAN_POINT('Ctrl Pts',(15.9363601779561,33.5901958958426,0.943978082272566));
#34083=CARTESIAN_POINT('Ctrl Pts',(15.8959902453333,33.5813120719146,0.508394167536556));
#34084=CARTESIAN_POINT('Ctrl Pts',(15.750152846408,33.6475470722109,-1.9528862309875));
#34085=CARTESIAN_POINT('Ctrl Pts',(15.7999367855882,34.0453300100471,-3.87317034519758));
#34086=CARTESIAN_POINT('Ctrl Pts',(16.1874208229068,35.5112613559129,-7.48823335803259));
#34087=CARTESIAN_POINT('Ctrl Pts',(16.5326707000659,36.5583090926536,-9.12349227712147));
#34088=CARTESIAN_POINT('Ctrl Pts',(17.4478193086935,39.1677510875088,-11.877576477648));
#34089=CARTESIAN_POINT('Ctrl Pts',(18.0173264969392,40.7058538585587,-12.9726927515291));
#34090=CARTESIAN_POINT('Ctrl Pts',(19.2855449175038,44.100324448888,-14.4683433355072));
#34091=CARTESIAN_POINT('Ctrl Pts',(19.9768684693761,45.9046009234835,-14.8498038984958));
#34092=CARTESIAN_POINT('Ctrl Pts',(20.6698844856026,47.7263079790887,-14.8500516281495));
#34093=CARTESIAN_POINT('Ctrl Pts',(16.9191631550062,33.8728645130296,1.59674373345244));
#34094=CARTESIAN_POINT('Ctrl Pts',(16.9077095035907,33.8717595603211,1.48722881441631));
#34095=CARTESIAN_POINT('Ctrl Pts',(16.8962575457316,33.8706551854753,1.37773700546685));
#34096=CARTESIAN_POINT('Ctrl Pts',(16.8474438163014,33.8659442776997,0.910971509151797));
#34097=CARTESIAN_POINT('Ctrl Pts',(16.8074600408045,33.8577588503297,0.486453085737103));
#34098=CARTESIAN_POINT('Ctrl Pts',(16.6618156865167,33.923357117882,-1.8686043110222));
#34099=CARTESIAN_POINT('Ctrl Pts',(16.7047171138624,34.3078598045423,-3.70979114471382));
#34100=CARTESIAN_POINT('Ctrl Pts',(17.06597358491,35.714252540865,-7.17014261468207));
#34101=CARTESIAN_POINT('Ctrl Pts',(17.3918853009178,36.7203421551748,-8.73670574472941));
#34102=CARTESIAN_POINT('Ctrl Pts',(18.2583527462983,39.2225667173974,-11.3734544105359));
#34103=CARTESIAN_POINT('Ctrl Pts',(18.7990691968002,40.6990131476935,-12.422171495823));
#34104=CARTESIAN_POINT('Ctrl Pts',(20.0035017019234,43.951703746327,-13.8545909095629));
#34105=CARTESIAN_POINT('Ctrl Pts',(20.6613231478903,45.6843449310794,-14.2195188099295));
#34106=CARTESIAN_POINT('Ctrl Pts',(21.3197474319156,47.4295323472121,-14.2201291128084));
#34107=CARTESIAN_POINT('Ctrl Pts',(14.6113821712786,34.8604849513722,0.));
#34108=CARTESIAN_POINT('Ctrl Pts',(14.4963699339431,34.9137340334406,-1.86858636180158));
#34109=CARTESIAN_POINT('Ctrl Pts',(14.5381447126019,35.295769960475,-3.71029995870877));
#34110=CARTESIAN_POINT('Ctrl Pts',(14.9006586664244,36.7049156525685,-7.16936247492651));
#34111=CARTESIAN_POINT('Ctrl Pts',(15.2257990211768,37.7093165664651,-8.73699595770352));
#34112=CARTESIAN_POINT('Ctrl Pts',(15.7032568890503,39.0880341222379,-10.1890856763496));
#34113=CARTESIAN_POINT('Ctrl Pts',(15.7484477541909,39.2176525965029,-10.3203928635164));
#34114=CARTESIAN_POINT('Ctrl Pts',(15.7946976519012,39.3495129251702,-10.4488603765994));
#34115=CARTESIAN_POINT('Ctrl Pts',(16.7773762106053,33.8713086176789,-4.87766425512972E-9));
#34116=CARTESIAN_POINT('Ctrl Pts',(16.6618156863912,33.9233571184906,-1.86860431424824));
#34117=CARTESIAN_POINT('Ctrl Pts',(16.7047171138587,34.3078598051085,-3.7097911462516));
#34118=CARTESIAN_POINT('Ctrl Pts',(16.8853453492635,35.0110561726706,-5.43996687972851));
#34119=CARTESIAN_POINT('Ctrl Pts',(17.065973584826,35.7142525408467,-7.17014261471587));
#34120=CARTESIAN_POINT('Ctrl Pts',(17.3918853008714,36.7203421551681,-8.73670574475316));
#34121=CARTESIAN_POINT('Ctrl Pts',(17.8251190235963,37.9714544362846,-10.0550800776389));
#34122=CARTESIAN_POINT('Ctrl Pts',(17.8716259385837,38.1057592455494,-10.1966053555778));
#34123=CARTESIAN_POINT('Ctrl Pts',(17.9193714483196,38.2426607296427,-10.3350231942325));
#34124=CARTESIAN_POINT('Ctrl Pts',(17.9682986698117,38.3820655716568,-10.4702558451031));
#34125=CARTESIAN_POINT('Ctrl Pts',(15.4546943255724,41.8409566234847,1.24689092472248));
#34126=CARTESIAN_POINT('Ctrl Pts',(15.4432419692995,41.8398517957221,1.13738838925848));
#34127=CARTESIAN_POINT('Ctrl Pts',(15.4317882611895,41.8387464827965,1.02786758221446));
#34128=CARTESIAN_POINT('Ctrl Pts',(15.382976471443,41.8340390406186,0.561172897424529));
#34129=CARTESIAN_POINT('Ctrl Pts',(15.347591406502,41.8343710194829,0.25482887444235));
#34130=CARTESIAN_POINT('Ctrl Pts',(15.2075196934412,41.9009886759109,-0.978870002714429));
#34131=CARTESIAN_POINT('Ctrl Pts',(15.1720089790472,42.1326921493308,-1.98783577087912));
#34132=CARTESIAN_POINT('Ctrl Pts',(15.2628516086919,42.9247046141549,-3.80852727284543));
#34133=CARTESIAN_POINT('Ctrl Pts',(15.3806923683066,43.4898198932174,-4.65544360724633));
#34134=CARTESIAN_POINT('Ctrl Pts',(15.7347286943739,44.8634258749693,-6.04997283340658));
#34135=CARTESIAN_POINT('Ctrl Pts',(15.9692083427511,45.6839445213788,-6.61832169907737));
#34136=CARTESIAN_POINT('Ctrl Pts',(16.5029496834282,47.4457702195862,-7.36768403073895));
#34137=CARTESIAN_POINT('Ctrl Pts',(16.8055334254904,48.4183716585177,-7.57138648686101));
#34138=CARTESIAN_POINT('Ctrl Pts',(17.0992034029532,49.3570623388651,-7.5696258196942));
#34139=CARTESIAN_POINT('Ctrl Pts',(15.6825261124558,39.4829021650676,1.35489330510245));
#34140=CARTESIAN_POINT('Ctrl Pts',(15.6710733564754,39.4817972987448,1.24538694781347));
#34141=CARTESIAN_POINT('Ctrl Pts',(15.6596201873396,39.4806922726925,1.13587509032859));
#34142=CARTESIAN_POINT('Ctrl Pts',(15.6108078040348,39.4759837721979,0.669158551002801));
#34143=CARTESIAN_POINT('Ctrl Pts',(15.5740132903312,39.47370886399,0.326351368868663));
#34144=CARTESIAN_POINT('Ctrl Pts',(15.4322923840901,39.5401684749661,-1.25360819502657));
#34145=CARTESIAN_POINT('Ctrl Pts',(15.4208777676068,39.8187991368093,-2.51960912779614));
#34146=CARTESIAN_POINT('Ctrl Pts',(15.5953514322868,40.8008105435563,-4.84647586782445));
#34147=CARTESIAN_POINT('Ctrl Pts',(15.777362289462,41.501918872964,-5.91572199048063));
#34148=CARTESIAN_POINT('Ctrl Pts',(16.2896605076648,43.2240929050472,-7.69376028690621));
#34149=CARTESIAN_POINT('Ctrl Pts',(16.6186554011661,44.247051264828,-8.41063186560482));
#34150=CARTESIAN_POINT('Ctrl Pts',(17.3595514472245,46.4693548995415,-9.37059840616123));
#34151=CARTESIAN_POINT('Ctrl Pts',(17.7717772858494,47.6765808867826,-9.62435378627074));
#34152=CARTESIAN_POINT('Ctrl Pts',(18.178105907797,48.8643218056537,-9.62320046360536));
#34153=CARTESIAN_POINT('Ctrl Pts',(15.445567245734,37.1262286569851,1.47293201877982));
#34154=CARTESIAN_POINT('Ctrl Pts',(15.4341140531483,37.1251237485405,1.36342148686314));
#34155=CARTESIAN_POINT('Ctrl Pts',(15.4226614701644,37.1240190301314,1.25391940542181));
#34156=CARTESIAN_POINT('Ctrl Pts',(15.3738484494878,37.1193093979778,0.787178992716546));
#34157=CARTESIAN_POINT('Ctrl Pts',(15.3355356362411,37.1142341193648,0.404559744690755));
#34158=CARTESIAN_POINT('Ctrl Pts',(15.192166408545,37.1808604459796,-1.55402875459149));
#34159=CARTESIAN_POINT('Ctrl Pts',(15.2068479190282,37.5102521839538,-3.10121432124018));
#34160=CARTESIAN_POINT('Ctrl Pts',(15.4730537974558,38.7006440566388,-5.98129145450389));
#34161=CARTESIAN_POINT('Ctrl Pts',(15.7250611874973,39.5500810470602,-7.29389406576467));
#34162=CARTESIAN_POINT('Ctrl Pts',(16.410480382612,41.6535490821868,-9.49113593804184));
#34163=CARTESIAN_POINT('Ctrl Pts',(16.8427247306588,42.8976498812959,-10.3708286017556));
#34164=CARTESIAN_POINT('Ctrl Pts',(17.8102574729806,45.6237335200753,-11.5604045560864));
#34165=CARTESIAN_POINT('Ctrl Pts',(18.342326066798,47.0873378224161,-11.869476154138));
#34166=CARTESIAN_POINT('Ctrl Pts',(18.871842799404,48.547478432487,-11.8687142284811));
#34167=CARTESIAN_POINT('Ctrl Pts',(14.7529241788871,34.8615042977019,1.59647077610305));
#34168=CARTESIAN_POINT('Ctrl Pts',(14.7414705295773,34.8603993451984,1.48695587718898));
#34169=CARTESIAN_POINT('Ctrl Pts',(14.7300185573965,34.8592949433739,1.37746402257732));
#34170=CARTESIAN_POINT('Ctrl Pts',(14.6812048800314,34.8545841497086,0.910698635115021));
#34171=CARTESIAN_POINT('Ctrl Pts',(14.6413232655056,34.8466226370598,0.486448413022977));
#34172=CARTESIAN_POINT('Ctrl Pts',(14.4963699339431,34.9137340334406,-1.86858636180158));
#34173=CARTESIAN_POINT('Ctrl Pts',(14.5381447126019,35.295769960475,-3.71029995870877));
#34174=CARTESIAN_POINT('Ctrl Pts',(14.9006586664244,36.7049156525685,-7.16936247492651));
#34175=CARTESIAN_POINT('Ctrl Pts',(15.2257990211768,37.7093165664651,-8.73699595770352));
#34176=CARTESIAN_POINT('Ctrl Pts',(16.0925451480826,40.212151228894,-11.3730256982162));
#34177=CARTESIAN_POINT('Ctrl Pts',(16.6328052294162,41.6875985734161,-12.4235805192612));
#34178=CARTESIAN_POINT('Ctrl Pts',(17.8377468918383,44.9414037541357,-13.852947082121));
#34179=CARTESIAN_POINT('Ctrl Pts',(18.4952436947468,46.6732919100327,-14.2204718556786));
#34180=CARTESIAN_POINT('Ctrl Pts',(19.1537534053194,48.4187086763094,-14.2198708430666));
#34181=CARTESIAN_POINT('Ctrl Pts',(16.9191631550062,33.8728645130296,1.59674373345244));
#34182=CARTESIAN_POINT('Ctrl Pts',(16.9077095035907,33.8717595603211,1.48722881441631));
#34183=CARTESIAN_POINT('Ctrl Pts',(16.8962575457316,33.8706551854753,1.37773700546685));
#34184=CARTESIAN_POINT('Ctrl Pts',(16.8474438163014,33.8659442776997,0.910971509151797));
#34185=CARTESIAN_POINT('Ctrl Pts',(16.8074600408045,33.8577588503297,0.486453085737103));
#34186=CARTESIAN_POINT('Ctrl Pts',(16.6618156865167,33.923357117882,-1.8686043110222));
#34187=CARTESIAN_POINT('Ctrl Pts',(16.7047171138649,34.3078598045423,-3.70979114471382));
#34188=CARTESIAN_POINT('Ctrl Pts',(17.0659735849076,35.714252540865,-7.17014261468207));
#34189=CARTESIAN_POINT('Ctrl Pts',(17.3918853009202,36.7203421551748,-8.73670574472701));
#34190=CARTESIAN_POINT('Ctrl Pts',(18.2583527462959,39.2225667173974,-11.3734544105383));
#34191=CARTESIAN_POINT('Ctrl Pts',(18.7990691968002,40.6990131476983,-12.422171495823));
#34192=CARTESIAN_POINT('Ctrl Pts',(20.0035017019234,43.9517037463222,-13.8545909095629));
#34193=CARTESIAN_POINT('Ctrl Pts',(20.6613231478936,45.6843449310818,-14.2195188099295));
#34194=CARTESIAN_POINT('Ctrl Pts',(21.3197474319156,47.4295323472121,-14.2201291128084));
#34195=CARTESIAN_POINT('Ctrl Pts',(18.1761744494743,35.8800194678369,1.47327608945381));
#34196=CARTESIAN_POINT('Ctrl Pts',(18.1647212542343,35.8789145591374,1.36376553217266));
#34197=CARTESIAN_POINT('Ctrl Pts',(18.1532686893033,35.8778098747331,1.25426350828991));
#34198=CARTESIAN_POINT('Ctrl Pts',(18.1044556029977,35.8731000987367,0.787522958372509));
#34199=CARTESIAN_POINT('Ctrl Pts',(18.0660140128755,35.8677425691122,0.404565634782747));
#34200=CARTESIAN_POINT('Ctrl Pts',(17.9217737309507,35.9324615528443,-1.55405138010588));
#34201=CARTESIAN_POINT('Ctrl Pts',(17.9378754148555,36.2649627130355,-3.10057294640892));
#34202=CARTESIAN_POINT('Ctrl Pts',(18.2024961996828,37.4518844049553,-5.98227484334405));
#34203=CARTESIAN_POINT('Ctrl Pts',(18.4554759130143,38.3034500513362,-7.29352824387394));
#34204=CARTESIAN_POINT('Ctrl Pts',(19.1405438219643,40.4061490374087,-9.49167634238395));
#34205=CARTESIAN_POINT('Ctrl Pts',(19.5733634366175,41.6515092131842,-10.3690524867446));
#34206=CARTESIAN_POINT('Ctrl Pts',(20.5402543713576,44.3761878888422,-11.56247664837));
#34207=CARTESIAN_POINT('Ctrl Pts',(21.0727284454705,45.8407435516782,-11.8682745705118));
#34208=CARTESIAN_POINT('Ctrl Pts',(21.6021412371498,47.3005929134933,-11.8690397849988));
#34209=CARTESIAN_POINT('Ctrl Pts',(19.8012255369165,37.603187989015,1.35541228259764));
#34210=CARTESIAN_POINT('Ctrl Pts',(19.7897727769317,37.6020831223044,1.24590588705036));
#34211=CARTESIAN_POINT('Ctrl Pts',(19.7783196350271,37.6009781475457,1.13639411638362));
#34212=CARTESIAN_POINT('Ctrl Pts',(19.7295071527289,37.5962694300892,0.66967737009454));
#34213=CARTESIAN_POINT('Ctrl Pts',(19.6925183989912,37.5935687898023,0.326360253163144));
#34214=CARTESIAN_POINT('Ctrl Pts',(19.5494836419133,37.6571514684844,-1.25364232212218));
#34215=CARTESIAN_POINT('Ctrl Pts',(19.5402111377983,37.940472213727,-2.51864171287444));
#34216=CARTESIAN_POINT('Ctrl Pts',(19.7122939334821,38.9172493884975,-4.84795915807957));
#34217=CARTESIAN_POINT('Ctrl Pts',(19.8957713902382,39.6215684668099,-5.91517020463239));
#34218=CARTESIAN_POINT('Ctrl Pts',(20.4075397474896,41.3425825071161,-7.69457540343085));
#34219=CARTESIAN_POINT('Ctrl Pts',(20.7374023418622,42.3674404421722,-8.40795287031109));
#34220=CARTESIAN_POINT('Ctrl Pts',(21.4773303202594,44.5876249069278,-9.37372383747847));
#34221=CARTESIAN_POINT('Ctrl Pts',(21.8901596096332,45.7962902185517,-9.62254085996823));
#34222=CARTESIAN_POINT('Ctrl Pts',(22.2963396064214,46.9835874904387,-9.6236915153539));
#34223=CARTESIAN_POINT('Ctrl Pts',(21.7318648520659,38.9761478068776,1.24768188077462));
#34224=CARTESIAN_POINT('Ctrl Pts',(21.7204124896902,38.975042978526,1.13817928700242));
#34225=CARTESIAN_POINT('Ctrl Pts',(21.7089588230816,38.9739377437727,1.02865861227501));
#34226=CARTESIAN_POINT('Ctrl Pts',(21.6601468824651,38.9692299709329,0.561963612059301));
#34227=CARTESIAN_POINT('Ctrl Pts',(21.6244657828545,38.9689131059274,0.254842414695162));
#34228=CARTESIAN_POINT('Ctrl Pts',(21.4823916741561,39.0311461271326,-0.978922014666903));
#34229=CARTESIAN_POINT('Ctrl Pts',(21.4501456807868,39.2699975980546,-1.98636136650924));
#34230=CARTESIAN_POINT('Ctrl Pts',(21.5373444678502,40.0540327469369,-3.81078790536759));
#34231=CARTESIAN_POINT('Ctrl Pts',(21.6574204222861,40.6240414198376,-4.65460264909511));
#34232=CARTESIAN_POINT('Ctrl Pts',(22.0106492052001,41.9958794973213,-6.05121512493767));
#34233=CARTESIAN_POINT('Ctrl Pts',(22.246451287129,42.8192932221962,-6.6142387329399));
#34234=CARTESIAN_POINT('Ctrl Pts',(22.7787172286239,44.5778891651125,-7.37244739492444));
#34235=CARTESIAN_POINT('Ctrl Pts',(23.0822022983367,45.5526929856933,-7.56862230168617));
#34236=CARTESIAN_POINT('Ctrl Pts',(23.3756641324471,46.4906987626548,-7.57037421506013));
#34237=CARTESIAN_POINT('Ctrl Pts',(19.5640700378123,32.4071044310924,1.59647086199746));
#34238=CARTESIAN_POINT('Ctrl Pts',(19.5525757159953,32.407640749801,1.48695593443964));
#34239=CARTESIAN_POINT('Ctrl Pts',(19.541083132609,32.4081773749034,1.37746405122481));
#34240=CARTESIAN_POINT('Ctrl Pts',(19.4920958892454,32.4104614410692,0.910698635070352));
#34241=CARTESIAN_POINT('Ctrl Pts',(19.4514871706788,32.4082567106452,0.486448412994875));
#34242=CARTESIAN_POINT('Ctrl Pts',(19.3175602025089,32.4953140197786,-1.8685863617208));
#34243=CARTESIAN_POINT('Ctrl Pts',(19.4132791554013,32.8675162009675,-3.71029995872154));
#34244=CARTESIAN_POINT('Ctrl Pts',(19.9726455810625,34.2107277071049,-7.16936247491371));
#34245=CARTESIAN_POINT('Ctrl Pts',(20.4374176293853,35.1586329709741,-8.7369959576679));
#34246=CARTESIAN_POINT('Ctrl Pts',(21.6515320408687,37.5126415502708,-11.373025698252));
#34247=CARTESIAN_POINT('Ctrl Pts',(22.3962711035792,38.8961839423097,-12.4235805192226));
#34248=CARTESIAN_POINT('Ctrl Pts',(24.0520129555351,41.9453889999262,-13.8529470821599));
#34249=CARTESIAN_POINT('Ctrl Pts',(24.949290771548,43.5660774805884,-14.2204718555979));
#34250=CARTESIAN_POINT('Ctrl Pts',(25.8494965077559,45.2000127177925,-14.2198708430668));
#34251=CARTESIAN_POINT('Ctrl Pts',(19.8251119861394,31.4917047963493,1.62964630360506));
#34252=CARTESIAN_POINT('Ctrl Pts',(19.8136175409443,31.4922411208174,1.52013020054019));
#34253=CARTESIAN_POINT('Ctrl Pts',(19.8021251364111,31.4927778131311,1.41064106979313));
#34254=CARTESIAN_POINT('Ctrl Pts',(19.7531376566116,31.4950615682937,0.943868932592553));
#34255=CARTESIAN_POINT('Ctrl Pts',(19.7119675267496,31.4920962479327,0.508392298420167));
#34256=CARTESIAN_POINT('Ctrl Pts',(19.5774004974823,31.5789716511435,-1.95287905120954));
#34257=CARTESIAN_POINT('Ctrl Pts',(19.6827016275074,31.9647082138112,-3.87337387080853));
#34258=CARTESIAN_POINT('Ctrl Pts',(20.2755200062621,33.3615921547092,-7.48792130211721));
#34259=CARTESIAN_POINT('Ctrl Pts',(20.7658646319223,34.3482235805455,-9.1236083622931));
#34260=CARTESIAN_POINT('Ctrl Pts',(22.043205731485,36.8010916838837,-11.8774049927381));
#34261=CARTESIAN_POINT('Ctrl Pts',(22.8255734410865,38.2421198758929,-12.9732563608867));
#34262=CARTESIAN_POINT('Ctrl Pts',(24.5642317986417,41.4219656611118,-14.4676858045482));
#34263=CARTESIAN_POINT('Ctrl Pts',(25.5051223581969,43.1092121219442,-14.8501851004724));
#34264=CARTESIAN_POINT('Ctrl Pts',(26.4503875219925,44.8138361237935,-14.8499483202529));
#34265=CARTESIAN_POINT('Ctrl Pts',(20.6265086564333,30.9769588736642,1.62975548654484));
#34266=CARTESIAN_POINT('Ctrl Pts',(20.615014210394,30.9774951981734,1.52023937542784));
#34267=CARTESIAN_POINT('Ctrl Pts',(20.603521813066,30.978031900352,1.41075026295318));
#34268=CARTESIAN_POINT('Ctrl Pts',(20.5545343061555,30.9803156132948,0.943978082193564));
#34269=CARTESIAN_POINT('Ctrl Pts',(20.513310981293,30.9772674543119,0.508394167507573));
#34270=CARTESIAN_POINT('Ctrl Pts',(20.3783842201005,31.0635831036799,-1.95288623090451));
#34271=CARTESIAN_POINT('Ctrl Pts',(20.4842718451503,31.450232191471,-3.87317034520782));
#34272=CARTESIAN_POINT('Ctrl Pts',(21.0764356359399,32.846097741863,-7.48823335802198));
#34273=CARTESIAN_POINT('Ctrl Pts',(21.56718179641,33.8333538619857,-9.1234922771287));
#34274=CARTESIAN_POINT('Ctrl Pts',(22.8443778274949,36.2859962734605,-11.8775764776405));
#34275=CARTESIAN_POINT('Ctrl Pts',(23.6269831005624,37.7273940528029,-12.9726927515381));
#34276=CARTESIAN_POINT('Ctrl Pts',(25.3653764195812,40.906827527409,-14.4683433354979));
#34277=CARTESIAN_POINT('Ctrl Pts',(26.3064386088075,42.5943534697472,-14.8498038985242));
#34278=CARTESIAN_POINT('Ctrl Pts',(27.2516566664772,44.2988917118185,-14.8500516281494));
#34279=CARTESIAN_POINT('Ctrl Pts',(21.5675617135471,31.1202396243797,1.59674381934692));
#34280=CARTESIAN_POINT('Ctrl Pts',(21.5560673896166,31.1207759431929,1.48722887165912));
#34281=CARTESIAN_POINT('Ctrl Pts',(21.5445748242466,31.1213125929552,1.37773703412493));
#34282=CARTESIAN_POINT('Ctrl Pts',(21.4955875131045,31.123596553574,0.91097150907293));
#34283=CARTESIAN_POINT('Ctrl Pts',(21.4548458070374,31.1211847265943,0.486453085713372));
#34284=CARTESIAN_POINT('Ctrl Pts',(21.3200195090543,31.2068426511148,-1.86860431095823));
#34285=CARTESIAN_POINT('Ctrl Pts',(21.4172046995109,31.5813261451026,-3.70979114472278));
#34286=CARTESIAN_POINT('Ctrl Pts',(21.9749346552545,32.9219916750036,-7.17014261467265));
#34287=CARTESIAN_POINT('Ctrl Pts',(22.4407105406093,33.871458674577,-8.73670574475808));
#34288=CARTESIAN_POINT('Ctrl Pts',(23.6544622808885,36.2249030242105,-11.3734544105068));
#34289=CARTESIAN_POINT('Ctrl Pts',(24.3997952522761,37.6093693845942,-12.4221714958608));
#34290=CARTESIAN_POINT('Ctrl Pts',(26.0548745078767,40.6575436656595,-13.8545909095247));
#34291=CARTESIAN_POINT('Ctrl Pts',(26.952580829692,42.2789313088625,-14.2195188100196));
#34292=CARTESIAN_POINT('Ctrl Pts',(27.8526693689676,43.9126516878549,-14.2201291128082));
#34293=CARTESIAN_POINT('Ctrl Pts',(19.4238236466312,32.4262389885811,0.));
#34294=CARTESIAN_POINT('Ctrl Pts',(19.3175602025089,32.4953140197786,-1.8685863617208));
#34295=CARTESIAN_POINT('Ctrl Pts',(19.4132791554013,32.8675162009675,-3.71029995872154));
#34296=CARTESIAN_POINT('Ctrl Pts',(19.9726455810625,34.2107277071049,-7.16936247491372));
#34297=CARTESIAN_POINT('Ctrl Pts',(20.4374176293853,35.1586329709693,-8.73699595766551));
#34298=CARTESIAN_POINT('Ctrl Pts',(21.1062276306836,36.455367830626,-10.1890856763532));
#34299=CARTESIAN_POINT('Ctrl Pts',(21.169405150186,36.5772356450468,-10.3203928635223));
#34300=CARTESIAN_POINT('Ctrl Pts',(21.2339499719776,36.7011717789779,-10.4488603766068));
#34301=CARTESIAN_POINT('Ctrl Pts',(21.4269965197897,31.1388779522826,-4.87765838243573E-9));
#34302=CARTESIAN_POINT('Ctrl Pts',(21.3200195090168,31.2068426517351,-1.86860431418425));
#34303=CARTESIAN_POINT('Ctrl Pts',(21.4172046995881,31.5813261456637,-3.70979114626052));
#34304=CARTESIAN_POINT('Ctrl Pts',(21.6960696772569,32.251658910038,-5.43996687972819));
#34305=CARTESIAN_POINT('Ctrl Pts',(21.9749346551692,32.9219916749975,-7.17014261470629));
#34306=CARTESIAN_POINT('Ctrl Pts',(22.440710540563,33.871458674577,-8.73670574478158));
#34307=CARTESIAN_POINT('Ctrl Pts',(23.0475864107378,35.0481808493939,-10.0550800776383));
#34308=CARTESIAN_POINT('Ctrl Pts',(23.1127335196115,35.1745000052616,-10.1966053555741));
#34309=CARTESIAN_POINT('Ctrl Pts',(23.179476161479,35.3032131351426,-10.3350231942268));
#34310=CARTESIAN_POINT('Ctrl Pts',(23.2477447519554,35.434235967254,-10.4702558450963));
#34311=CARTESIAN_POINT('Ctrl Pts',(21.2519768052529,39.2156436908075,1.24689101061695));
#34312=CARTESIAN_POINT('Ctrl Pts',(21.2404837810657,39.2161799489647,1.13738844654561));
#34313=CARTESIAN_POINT('Ctrl Pts',(21.22898934975,39.2167159192913,1.02786761081392));
#34314=CARTESIAN_POINT('Ctrl Pts',(21.1800044517766,39.2190030341997,0.561172897522604));
#34315=CARTESIAN_POINT('Ctrl Pts',(21.1450268012714,39.2243674537804,0.254828874451871));
#34316=CARTESIAN_POINT('Ctrl Pts',(21.0158614973502,39.3102413217381,-0.978870002765215));
#34317=CARTESIAN_POINT('Ctrl Pts',(21.0136870730547,39.5446400894209,-1.98783577088475));
#34318=CARTESIAN_POINT('Ctrl Pts',(21.2163201816873,40.3156627552368,-3.80852727284064));
#34319=CARTESIAN_POINT('Ctrl Pts',(21.4133857819021,40.8582554869398,-4.65544360715122));
#34320=CARTESIAN_POINT('Ctrl Pts',(21.959303041511,42.1674955178466,-6.04997283350267));
#34321=CARTESIAN_POINT('Ctrl Pts',(22.3081680038698,42.9462925342929,-6.61832169897219));
#34322=CARTESIAN_POINT('Ctrl Pts',(23.0872105663855,44.6142260746892,-7.36768403084516));
#34323=CARTESIAN_POINT('Ctrl Pts',(23.5251300589823,45.5338656769717,-7.57138648667118));
#34324=CARTESIAN_POINT('Ctrl Pts',(23.9494005117261,46.4212082443696,-7.56962581969484));
#34325=CARTESIAN_POINT('Ctrl Pts',(21.141903454163,36.8491669828396,1.35489339099692));
#34326=CARTESIAN_POINT('Ctrl Pts',(21.1304100288482,36.8497032597153,1.24538700508779));
#34327=CARTESIAN_POINT('Ctrl Pts',(21.1189161718497,36.8502394372903,1.13587511894501));
#34328=CARTESIAN_POINT('Ctrl Pts',(21.0699305357382,36.8525255891216,0.669158551049937));
#34329=CARTESIAN_POINT('Ctrl Pts',(21.0331867839281,36.8555102414576,0.326351368867465));
#34330=CARTESIAN_POINT('Ctrl Pts',(20.9023665809823,36.9414623773007,-1.25360819504018));
#34331=CARTESIAN_POINT('Ctrl Pts',(20.9307214263708,37.2188814500163,-2.51960912780411));
#34332=CARTESIAN_POINT('Ctrl Pts',(21.2431739952935,38.1660672052508,-4.84647586781696));
#34333=CARTESIAN_POINT('Ctrl Pts',(21.5231103629303,38.8341364170866,-5.91572199041885));
#34334=CARTESIAN_POINT('Ctrl Pts',(22.2752850426782,40.4658735625663,-7.69376028696859));
#34335=CARTESIAN_POINT('Ctrl Pts',(22.7465133961687,41.4315988262065,-8.41063186553296));
#34336=CARTESIAN_POINT('Ctrl Pts',(23.7961349710495,43.5258421132212,-9.37059840623374));
#34337=CARTESIAN_POINT('Ctrl Pts',(24.3759711162347,44.6621144270458,-9.62435378613789));
#34338=CARTESIAN_POINT('Ctrl Pts',(24.9471970554252,45.7799392638234,-9.62320046360578));
#34339=CARTESIAN_POINT('Ctrl Pts',(20.5719668778723,34.5502037758216,1.47293210467427));
#34340=CARTESIAN_POINT('Ctrl Pts',(20.5604730144019,34.5507400731433,1.36342154412501));
#34341=CARTESIAN_POINT('Ctrl Pts',(20.5489797813727,34.5512764718092,1.25391943405454));
#34342=CARTESIAN_POINT('Ctrl Pts',(20.4999933533187,34.5535615942045,0.787178992715231));
#34343=CARTESIAN_POINT('Ctrl Pts',(20.461348221816,34.5539904564244,0.404559744676866));
#34344=CARTESIAN_POINT('Ctrl Pts',(20.3289202010264,34.6403421915839,-1.55402875456067));
#34345=CARTESIAN_POINT('Ctrl Pts',(20.3903296068372,34.9642917997669,-3.10121432125053));
#34346=CARTESIAN_POINT('Ctrl Pts',(20.8232363200805,36.1046821531124,-5.98129145449374));
#34347=CARTESIAN_POINT('Ctrl Pts',(21.1935661261622,36.9096087088253,-7.29389406572193));
#34348=CARTESIAN_POINT('Ctrl Pts',(22.1713634554357,38.8941211502969,-9.49113593808493));
#34349=CARTESIAN_POINT('Ctrl Pts',(22.7762621832304,40.0640440127247,-10.3708286017076));
#34350=CARTESIAN_POINT('Ctrl Pts',(24.1219089895441,42.6246857849171,-11.5604045561349));
#34351=CARTESIAN_POINT('Ctrl Pts',(24.8568545017351,43.9976714500213,-11.8694761540621));
#34352=CARTESIAN_POINT('Ctrl Pts',(25.5887811923518,45.3675918458115,-11.8687142284814));
#34353=CARTESIAN_POINT('Ctrl Pts',(19.5640700378123,32.4071044310924,1.59647086199746));
#34354=CARTESIAN_POINT('Ctrl Pts',(19.5525757159953,32.407640749801,1.48695593443965));
#34355=CARTESIAN_POINT('Ctrl Pts',(19.541083132609,32.4081773749034,1.37746405122479));
#34356=CARTESIAN_POINT('Ctrl Pts',(19.4920958892454,32.4104614410692,0.910698635070432));
#34357=CARTESIAN_POINT('Ctrl Pts',(19.4514871706788,32.4082567106452,0.486448412994875));
#34358=CARTESIAN_POINT('Ctrl Pts',(19.3175602025089,32.4953140197786,-1.8685863617208));
#34359=CARTESIAN_POINT('Ctrl Pts',(19.4132791554013,32.8675162009675,-3.71029995872154));
#34360=CARTESIAN_POINT('Ctrl Pts',(19.9726455810625,34.2107277071049,-7.16936247491372));
#34361=CARTESIAN_POINT('Ctrl Pts',(20.4374176293853,35.1586329709693,-8.73699595766551));
#34362=CARTESIAN_POINT('Ctrl Pts',(21.6515320408687,37.5126415502755,-11.3730256982544));
#34363=CARTESIAN_POINT('Ctrl Pts',(22.3962711035816,38.8961839423097,-12.4235805192178));
#34364=CARTESIAN_POINT('Ctrl Pts',(24.0520129555327,41.9453889999262,-13.8529470821647));
#34365=CARTESIAN_POINT('Ctrl Pts',(24.9492907715565,43.5660774805847,-14.2204718556122));
#34366=CARTESIAN_POINT('Ctrl Pts',(25.849496507756,45.2000127177926,-14.2198708430668));
#34367=CARTESIAN_POINT('Ctrl Pts',(21.5675617135471,31.1202396243797,1.59674381934692));
#34368=CARTESIAN_POINT('Ctrl Pts',(21.5560673896166,31.1207759431929,1.48722887165912));
#34369=CARTESIAN_POINT('Ctrl Pts',(21.5445748242466,31.1213125929552,1.37773703412493));
#34370=CARTESIAN_POINT('Ctrl Pts',(21.4955875131045,31.123596553574,0.91097150907293));
#34371=CARTESIAN_POINT('Ctrl Pts',(21.4548458070375,31.1211847265943,0.486453085713372));
#34372=CARTESIAN_POINT('Ctrl Pts',(21.3200195090543,31.2068426511148,-1.86860431095823));
#34373=CARTESIAN_POINT('Ctrl Pts',(21.4172046995109,31.5813261451074,-3.70979114472278));
#34374=CARTESIAN_POINT('Ctrl Pts',(21.9749346552545,32.9219916749988,-7.17014261467265));
#34375=CARTESIAN_POINT('Ctrl Pts',(22.440710540607,33.8714586745723,-8.73670574475808));
#34376=CARTESIAN_POINT('Ctrl Pts',(23.6544622808909,36.2249030242152,-11.3734544105068));
#34377=CARTESIAN_POINT('Ctrl Pts',(24.3997952522713,37.609369384599,-12.4221714958608));
#34378=CARTESIAN_POINT('Ctrl Pts',(26.0548745078815,40.6575436656547,-13.8545909095247));
#34379=CARTESIAN_POINT('Ctrl Pts',(26.9525808296926,42.2789313088637,-14.2195188100053));
#34380=CARTESIAN_POINT('Ctrl Pts',(27.8526693689676,43.9126516878549,-14.2201291128082));
#34381=CARTESIAN_POINT('Ctrl Pts',(23.0974263782809,32.9280732767457,1.47327617534837));
#34382=CARTESIAN_POINT('Ctrl Pts',(23.0859325121477,32.9286095741995,1.36376558942454));
#34383=CARTESIAN_POINT('Ctrl Pts',(23.0744393018274,32.9291460039488,1.25426353693597));
#34384=CARTESIAN_POINT('Ctrl Pts',(23.0254527883363,32.9314309933027,0.787522958328138));
#34385=CARTESIAN_POINT('Ctrl Pts',(22.9866400222227,32.9315988042883,0.404565634774376));
#34386=CARTESIAN_POINT('Ctrl Pts',(22.8530783700626,33.0161865744744,-1.55405138009626));
#34387=CARTESIAN_POINT('Ctrl Pts',(22.9163360109425,33.3430118437575,-3.1005729464118));
#34388=CARTESIAN_POINT('Ctrl Pts',(23.3471799062865,34.480192920029,-5.98227484334081));
#34389=CARTESIAN_POINT('Ctrl Pts',(23.7187750781269,35.2870880890085,-7.29352824391455));
#34390=CARTESIAN_POINT('Ctrl Pts',(24.696115249804,37.2708893025804,-9.49167634234292));
#34391=CARTESIAN_POINT('Ctrl Pts',(25.3017626167546,38.4419768539684,-10.369052486792));
#34392=CARTESIAN_POINT('Ctrl Pts',(26.6465742010944,41.0013193023568,-11.5624766483221));
#34393=CARTESIAN_POINT('Ctrl Pts',(27.3820564590451,42.3751889385584,-11.8682745706114));
#34394=CARTESIAN_POINT('Ctrl Pts',(28.1138388177857,43.7448358429351,-11.8690397849985));
#34395=CARTESIAN_POINT('Ctrl Pts',(24.9511692381921,34.4024335442869,1.35541236849225));
#34396=CARTESIAN_POINT('Ctrl Pts',(24.9396758088609,34.4029698213615,1.24590594430949));
#34397=CARTESIAN_POINT('Ctrl Pts',(24.9281819861154,34.4035060458225,1.13639414502018));
#34398=CARTESIAN_POINT('Ctrl Pts',(24.8791962211348,34.4057919969771,0.669677370076627));
#34399=CARTESIAN_POINT('Ctrl Pts',(24.842199618394,34.4083828938322,0.326360253170264));
#34400=CARTESIAN_POINT('Ctrl Pts',(24.7096695075292,34.4916743608159,-1.25364232216775));
#34401=CARTESIAN_POINT('Ctrl Pts',(24.7408121301953,34.7734309243714,-2.5186417128748));
#34402=CARTESIAN_POINT('Ctrl Pts',(25.050153256772,35.7157759805858,-4.84795915807885));
#34403=CARTESIAN_POINT('Ctrl Pts',(25.3319982333083,36.3868145416154,-5.91517020469683));
#34404=CARTESIAN_POINT('Ctrl Pts',(26.0834833614016,38.0174789096184,-7.69457540336587));
#34405=CARTESIAN_POINT('Ctrl Pts',(26.5558409214786,38.9849609267486,-8.40795287038243));
#34406=CARTESIAN_POINT('Ctrl Pts',(27.6042026929608,41.0772443843887,-9.37372383740648));
#34407=CARTESIAN_POINT('Ctrl Pts',(28.1848409838016,42.2148554922686,-9.62254086011052));
#34408=CARTESIAN_POINT('Ctrl Pts',(28.7558566730953,43.3322623493509,-9.62369151535347));
#34409=CARTESIAN_POINT('Ctrl Pts',(27.0575499833001,35.4866599889488,1.2476819666693));
#34410=CARTESIAN_POINT('Ctrl Pts',(27.0460569529913,35.4871962474067,1.13817934426647));
#34411=CARTESIAN_POINT('Ctrl Pts',(27.0345625738794,35.4877322891927,1.02865864090515));
#34412=CARTESIAN_POINT('Ctrl Pts',(26.9855774795026,35.4900190982578,0.561963612058281));
#34413=CARTESIAN_POINT('Ctrl Pts',(26.9502144674433,35.4947834084228,0.254842414717359));
#34414=CARTESIAN_POINT('Ctrl Pts',(26.8184431506756,35.5766022409397,-0.978922014766397));
#34415=CARTESIAN_POINT('Ctrl Pts',(26.8205174834718,35.817611631747,-1.98636136650704));
#34416=CARTESIAN_POINT('Ctrl Pts',(27.0184085480269,36.5812567518629,-3.81078790536934));
#34417=CARTESIAN_POINT('Ctrl Pts',(27.2183829945314,37.128374968267,-4.65460264919051));
#34418=CARTESIAN_POINT('Ctrl Pts',(27.7632493317807,38.4359800153026,-6.05121512484151));
#34419=CARTESIAN_POINT('Ctrl Pts',(28.1138352797144,39.2174544403461,-6.61423873304951));
#34420=CARTESIAN_POINT('Ctrl Pts',(28.8909578184702,40.8824010710446,-7.37244739481389));
#34421=CARTESIAN_POINT('Ctrl Pts',(29.3300828960074,41.8040923654821,-7.56862230188999));
#34422=CARTESIAN_POINT('Ctrl Pts',(29.7540498521219,42.6907866227634,-7.57037421505949));
#34423=CARTESIAN_POINT('Ctrl Pts',(23.9769478445539,29.2929893708796,1.59647090706345));
#34424=CARTESIAN_POINT('Ctrl Pts',(23.9311433314981,29.301771192775,1.15259179090668));
#34425=CARTESIAN_POINT('Ctrl Pts',(23.8732845217093,29.3034887354955,0.635573104324147));
#34426=CARTESIAN_POINT('Ctrl Pts',(23.745500652653,29.4153831213306,-1.86858636177993));
#34427=CARTESIAN_POINT('Ctrl Pts',(23.8932152177665,29.7701745938172,-3.71029995869774));
#34428=CARTESIAN_POINT('Ctrl Pts',(24.6380470281269,31.0201080009988,-7.16936247493752));
#34429=CARTESIAN_POINT('Ctrl Pts',(25.232989351462,31.8922209971783,-8.73699595769178));
#34430=CARTESIAN_POINT('Ctrl Pts',(26.7697561790069,34.0494826673513,-11.373025698228));
#34431=CARTESIAN_POINT('Ctrl Pts',(27.703813483812,35.3129551733154,-12.4235805192707));
#34432=CARTESIAN_POINT('Ctrl Pts',(29.7766493955075,38.0954870863474,-13.8529470821116));
#34433=CARTESIAN_POINT('Ctrl Pts',(30.8954422364859,39.571983347561,-14.2204718557262));
#34434=CARTESIAN_POINT('Ctrl Pts',(32.019018405086,41.061174846415,-14.2198708430667));
#34435=CARTESIAN_POINT('Ctrl Pts',(24.1050578112645,28.3497570418623,1.62964634867101));
#34436=CARTESIAN_POINT('Ctrl Pts',(24.0596354334595,28.3584655992891,1.18947040158512));
#34437=CARTESIAN_POINT('Ctrl Pts',(24.0007720917071,28.359588878909,0.664244065124536));
#34438=CARTESIAN_POINT('Ctrl Pts',(23.8722870320971,28.4713886672015,-1.95287905126951));
#34439=CARTESIAN_POINT('Ctrl Pts',(24.031412384867,28.8382130746775,-3.87337387078473));
#34440=CARTESIAN_POINT('Ctrl Pts',(24.8169940396062,30.1365118993409,-7.48792130214111));
#34441=CARTESIAN_POINT('Ctrl Pts',(25.4427599557747,31.0433175237852,-9.12360836231226));
#34442=CARTESIAN_POINT('Ctrl Pts',(27.0561790920272,33.2894343746957,-11.877404992719));
#34443=CARTESIAN_POINT('Ctrl Pts',(28.0356631207126,34.6044524432662,-12.9732563609014));
#34444=CARTESIAN_POINT('Ctrl Pts',(30.2091636815192,37.5044951006041,-14.4676858045335));
#34445=CARTESIAN_POINT('Ctrl Pts',(31.380597539451,39.0406651371208,-14.8501851005532));
#34446=CARTESIAN_POINT('Ctrl Pts',(32.558834555691,40.5934132658113,-14.8499483202528));
#34447=CARTESIAN_POINT('Ctrl Pts',(24.8250414362346,27.7261998529422,1.62975553161075));
#34448=CARTESIAN_POINT('Ctrl Pts',(24.7796252351451,27.7349072261548,1.18963944140105));
#34449=CARTESIAN_POINT('Ctrl Pts',(24.7207188400682,27.7359890779467,0.664246507192925));
#34450=CARTESIAN_POINT('Ctrl Pts',(24.591770457568,27.8472541630883,-1.9528862309561));
#34451=CARTESIAN_POINT('Ctrl Pts',(24.7516062015319,28.2148983405182,-3.87317034518888));
#34452=CARTESIAN_POINT('Ctrl Pts',(25.5363949990201,29.5122822980524,-7.48823335804114));
#34453=CARTESIAN_POINT('Ctrl Pts',(26.1626472662176,30.419649113926,-9.12349227713835));
#34454=CARTESIAN_POINT('Ctrl Pts',(27.7758906912504,32.6655632155555,-11.877576477631));
#34455=CARTESIAN_POINT('Ctrl Pts',(28.7556624631346,33.9809133008155,-12.9726927515241));
#34456=CARTESIAN_POINT('Ctrl Pts',(30.9288420051759,36.8805855631592,-14.4683433355121));
#34457=CARTESIAN_POINT('Ctrl Pts',(32.1004855202045,38.4170078110479,-14.849803898529));
#34458=CARTESIAN_POINT('Ctrl Pts',(33.2786637049095,39.969677756751,-14.8500516281494));
#34459=CARTESIAN_POINT('Ctrl Pts',(25.7769069069792,27.7340963985794,1.59674386441279));
#34460=CARTESIAN_POINT('Ctrl Pts',(25.731117835711,27.7428752599414,1.15301439044677));
#34461=CARTESIAN_POINT('Ctrl Pts',(25.6731513926117,27.7444892330921,0.63557920949513));
#34462=CARTESIAN_POINT('Ctrl Pts',(25.5442092163314,27.8550468610404,-1.86860431099641));
#34463=CARTESIAN_POINT('Ctrl Pts',(25.6936997594266,28.2118877584239,-3.7097911447099));
#34464=CARTESIAN_POINT('Ctrl Pts',(26.4365494266639,29.4595339977728,-7.1701426146858));
#34465=CARTESIAN_POINT('Ctrl Pts',(27.0327076275608,30.3330499725183,-8.73670574475581));
#34466=CARTESIAN_POINT('Ctrl Pts',(28.5690351770732,32.4898047695127,-11.3734544105093));
#34467=CARTESIAN_POINT('Ctrl Pts',(29.5038118398612,33.7541073171817,-12.4221714958132));
#34468=CARTESIAN_POINT('Ctrl Pts',(31.5758452046551,36.5357132427424,-13.8545909095725));
#34469=CARTESIAN_POINT('Ctrl Pts',(32.6951616911097,38.012840567309,-14.2195188099579));
#34470=CARTESIAN_POINT('Ctrl Pts',(33.8185912781324,39.5018360737641,-14.2201291128083));
#34471=CARTESIAN_POINT('Ctrl Pts',(23.8408520862202,29.3318883095339,0.));
#34472=CARTESIAN_POINT('Ctrl Pts',(23.745500652653,29.4153831213306,-1.86858636177993));
#34473=CARTESIAN_POINT('Ctrl Pts',(23.8932152177665,29.7701745938172,-3.71029995869894));
#34474=CARTESIAN_POINT('Ctrl Pts',(24.6380470281269,31.0201080009988,-7.16936247493632));
#34475=CARTESIAN_POINT('Ctrl Pts',(25.232989351462,31.8922209971783,-8.73699595769657));
#34476=CARTESIAN_POINT('Ctrl Pts',(26.0795364430743,33.0805753785968,-10.1890856763504));
#34477=CARTESIAN_POINT('Ctrl Pts',(26.15941450482,33.1922116559193,-10.3203928635178));
#34478=CARTESIAN_POINT('Ctrl Pts',(26.2409403042474,33.3057006128359,-10.4488603766015));
#34479=CARTESIAN_POINT('Ctrl Pts',(25.6404249706861,27.7725495286735,-4.44089209850063E-16));
#34480=CARTESIAN_POINT('Ctrl Pts',(25.5442092163314,27.8550468610404,-1.86860431099641));
#34481=CARTESIAN_POINT('Ctrl Pts',(25.6936997594266,28.2118877584239,-3.7097911447099));
#34482=CARTESIAN_POINT('Ctrl Pts',(26.4365494266639,29.4595339977728,-7.1701426146858));
#34483=CARTESIAN_POINT('Ctrl Pts',(27.0327076275608,30.3330499725183,-8.73670574475581));
#34484=CARTESIAN_POINT('Ctrl Pts',(27.8833324977841,31.5271893797555,-10.1966053555712));
#34485=CARTESIAN_POINT('Ctrl Pts',(27.9677135840473,31.6450939272834,-10.3350231942261));
#34486=CARTESIAN_POINT('Ctrl Pts',(28.0539337918646,31.7650675024726,-10.4702558450975));
#34487=CARTESIAN_POINT('Ctrl Pts',(26.6166303184858,35.7920133394052,1.246891055683));
#34488=CARTESIAN_POINT('Ctrl Pts',(26.5668264024408,35.8015619425913,0.764254809540097));
#34489=CARTESIAN_POINT('Ctrl Pts',(26.5193322761004,35.8093225655949,0.332948724830185));
#34490=CARTESIAN_POINT('Ctrl Pts',(26.3963809658133,35.9192508155907,-0.978870002769003));
#34491=CARTESIAN_POINT('Ctrl Pts',(26.4275870969047,36.1515731946735,-1.98783577087676));
#34492=CARTESIAN_POINT('Ctrl Pts',(26.73788565842,36.8859102633353,-3.80852727284811));
#34493=CARTESIAN_POINT('Ctrl Pts',(27.010164411852,37.3949348243697,-4.65544360718925));
#34494=CARTESIAN_POINT('Ctrl Pts',(27.7368493043565,38.6131565530536,-6.04997283346413));
#34495=CARTESIAN_POINT('Ctrl Pts',(28.1929976956625,39.33437787813,-6.61832169910145));
#34496=CARTESIAN_POINT('Ctrl Pts',(29.2014824204412,40.8744649436741,-7.36768403071517));
#34497=CARTESIAN_POINT('Ctrl Pts',(29.7658228849981,41.7224214991986,-7.57138648699933));
#34498=CARTESIAN_POINT('Ctrl Pts',(30.3120568904488,42.5403522177283,-7.56962581969453));
#34499=CARTESIAN_POINT('Ctrl Pts',(26.1708926054255,33.4652890233053,1.35489343606293));
#34500=CARTESIAN_POINT('Ctrl Pts',(26.122326829298,33.4746002454361,0.884255668131405));
#34501=CARTESIAN_POINT('Ctrl Pts',(26.071610116799,33.4804735791579,0.426397017785922));
#34502=CARTESIAN_POINT('Ctrl Pts',(25.9469288716926,33.5907346359619,-1.25360819505675));
#34503=CARTESIAN_POINT('Ctrl Pts',(26.0144759561813,33.8612946673471,-2.51960912779128));
#34504=CARTESIAN_POINT('Ctrl Pts',(26.4585467959407,34.754372800441,-4.84647586782949));
#34505=CARTESIAN_POINT('Ctrl Pts',(26.8307099768296,35.3758029321005,-5.91572199044501));
#34506=CARTESIAN_POINT('Ctrl Pts',(27.8074490109455,36.8838857283533,-7.6937602869421));
#34507=CARTESIAN_POINT('Ctrl Pts',(28.4113179738729,37.7727185143267,-8.41063186561923));
#34508=CARTESIAN_POINT('Ctrl Pts',(29.7482978093313,39.6962686996606,-9.37059840614699));
#34509=CARTESIAN_POINT('Ctrl Pts',(30.4839404690741,40.7384561124946,-9.62435378637083));
#34510=CARTESIAN_POINT('Ctrl Pts',(31.2084352127806,41.7636091770244,-9.62320046360557));
#34511=CARTESIAN_POINT('Ctrl Pts',(25.279580584698,31.2708363785843,1.47293214974027));
#34512=CARTESIAN_POINT('Ctrl Pts',(25.232365242191,31.2798886902605,1.01538106787277));
#34513=CARTESIAN_POINT('Ctrl Pts',(25.1781488031011,31.283721524738,0.528580803097958));
#34514=CARTESIAN_POINT('Ctrl Pts',(25.0518358019869,31.3946464646171,-1.55402875459593));
#34515=CARTESIAN_POINT('Ctrl Pts',(25.1587229846854,31.7065592633067,-3.10121432123402));
#34516=CARTESIAN_POINT('Ctrl Pts',(25.7495178005035,32.7737330381764,-5.98129145451011));
#34517=CARTESIAN_POINT('Ctrl Pts',(26.2306311757221,33.5177631757119,-7.29389406574337));
#34518=CARTESIAN_POINT('Ctrl Pts',(27.480901505213,35.3429210732599,-9.4911359380633));
#34519=CARTESIAN_POINT('Ctrl Pts',(28.2461406191471,36.414849743132,-10.3708286017604));
#34520=CARTESIAN_POINT('Ctrl Pts',(29.942508000842,38.7579223667066,-11.5604045560817));
#34521=CARTESIAN_POINT('Ctrl Pts',(30.8653690604319,40.0123393655871,-11.8694761542142));
#34522=CARTESIAN_POINT('Ctrl Pts',(31.7848057921743,41.2641519184869,-11.8687142284813));
#34523=CARTESIAN_POINT('Ctrl Pts',(23.9769478445539,29.2929893708796,1.59647090706345));
#34524=CARTESIAN_POINT('Ctrl Pts',(23.9311433314981,29.301771192775,1.15259179090668));
#34525=CARTESIAN_POINT('Ctrl Pts',(23.8732845217093,29.3034887354955,0.635573104324147));
#34526=CARTESIAN_POINT('Ctrl Pts',(23.7455006526529,29.4153831213306,-1.86858636177993));
#34527=CARTESIAN_POINT('Ctrl Pts',(23.8932152177665,29.7701745938172,-3.71029995869894));
#34528=CARTESIAN_POINT('Ctrl Pts',(24.6380470281269,31.0201080009988,-7.16936247493632));
#34529=CARTESIAN_POINT('Ctrl Pts',(25.232989351462,31.8922209971783,-8.73699595769657));
#34530=CARTESIAN_POINT('Ctrl Pts',(26.7697561790069,34.0494826673513,-11.3730256982232));
#34531=CARTESIAN_POINT('Ctrl Pts',(27.7038134838072,35.3129551733154,-12.423580519266));
#34532=CARTESIAN_POINT('Ctrl Pts',(29.7766493955123,38.0954870863474,-13.8529470821163));
#34533=CARTESIAN_POINT('Ctrl Pts',(30.895442236499,39.5719833475484,-14.220471855731));
#34534=CARTESIAN_POINT('Ctrl Pts',(32.019018405086,41.061174846415,-14.2198708430667));
#34535=CARTESIAN_POINT('Ctrl Pts',(25.7769069069792,27.7340963985794,1.59674386441279));
#34536=CARTESIAN_POINT('Ctrl Pts',(25.731117835711,27.7428752599414,1.15301439044677));
#34537=CARTESIAN_POINT('Ctrl Pts',(25.6731513926117,27.7444892330921,0.63557920949513));
#34538=CARTESIAN_POINT('Ctrl Pts',(25.5442092163314,27.8550468610404,-1.86860431099641));
#34539=CARTESIAN_POINT('Ctrl Pts',(25.6936997594266,28.2118877584239,-3.70979114470751));
#34540=CARTESIAN_POINT('Ctrl Pts',(26.4365494266639,29.4595339977728,-7.1701426146882));
#34541=CARTESIAN_POINT('Ctrl Pts',(27.0327076275608,30.3330499725231,-8.73670574475342));
#34542=CARTESIAN_POINT('Ctrl Pts',(28.5690351770732,32.4898047695079,-11.3734544105117));
#34543=CARTESIAN_POINT('Ctrl Pts',(29.5038118398636,33.7541073171817,-12.422171495818));
#34544=CARTESIAN_POINT('Ctrl Pts',(31.5758452046528,36.5357132427424,-13.8545909095677));
#34545=CARTESIAN_POINT('Ctrl Pts',(32.6951616911013,38.0128405673168,-14.2195188099532));
#34546=CARTESIAN_POINT('Ctrl Pts',(33.8185912781324,39.5018360737641,-14.2201291128083));
#34547=CARTESIAN_POINT('Ctrl Pts',(27.5484813091701,29.3058064687037,1.47327622041421));
#34548=CARTESIAN_POINT('Ctrl Pts',(27.501285431483,29.3148550485427,1.01591376687871));
#34549=CARTESIAN_POINT('Ctrl Pts',(27.4469333174788,29.3185573305647,0.528588498843467));
#34550=CARTESIAN_POINT('Ctrl Pts',(27.3191602364349,29.4277972482694,-1.5540513801051));
#34551=CARTESIAN_POINT('Ctrl Pts',(27.4282860910127,29.7422934066244,-3.10057294640986));
#34552=CARTESIAN_POINT('Ctrl Pts',(28.0165823577943,30.8065841399386,-5.98227484334298));
#34553=CARTESIAN_POINT('Ctrl Pts',(28.4992283820343,31.5523827727542,-7.29352824390031));
#34554=CARTESIAN_POINT('Ctrl Pts',(29.7489449887858,33.3769017419141,-9.49167634235738));
#34555=CARTESIAN_POINT('Ctrl Pts',(30.5150908743753,34.4498767034893,-10.3690524867348));
#34556=CARTESIAN_POINT('Ctrl Pts',(32.2104466223682,36.7917820929403,-11.5624766483796));
#34557=CARTESIAN_POINT('Ctrl Pts',(33.1339647666548,38.0469976785123,-11.8682745705069));
#34558=CARTESIAN_POINT('Ctrl Pts',(34.0532197137074,39.2985600643045,-11.8690397849987));
#34559=CARTESIAN_POINT('Ctrl Pts',(29.5931790826756,30.5013447592648,1.35541241355804));
#34560=CARTESIAN_POINT('Ctrl Pts',(29.5446426662243,30.5106503524935,0.88505916234556));
#34561=CARTESIAN_POINT('Ctrl Pts',(29.4937213090621,30.5163267679927,0.426408625629975));
#34562=CARTESIAN_POINT('Ctrl Pts',(29.3668377587824,30.624046228974,-1.25364232214448));
#34563=CARTESIAN_POINT('Ctrl Pts',(29.437761534203,30.8985028595929,-2.51864171288381));
#34564=CARTESIAN_POINT('Ctrl Pts',(29.8780636984596,31.7872323695978,-4.84795915807006));
#34565=CARTESIAN_POINT('Ctrl Pts',(30.2525386437882,32.4113300033619,-5.91517020466588));
#34566=CARTESIAN_POINT('Ctrl Pts',(31.2284424726404,33.9184490747759,-7.69457540339711));
#34567=CARTESIAN_POINT('Ctrl Pts',(31.8336791606301,34.8088600302697,-8.40795287029653));
#34568=CARTESIAN_POINT('Ctrl Pts',(33.1691331028056,36.7306496231043,-9.37372383749281));
#34569=CARTESIAN_POINT('Ctrl Pts',(33.9057602738327,37.7740480458422,-9.62254085997281));
#34570=CARTESIAN_POINT('Ctrl Pts',(34.6299874229482,38.798817306756,-9.62369151535367));
#34571=CARTESIAN_POINT('Ctrl Pts',(31.8324214200722,31.2747661069636,1.24768201173503));
#34572=CARTESIAN_POINT('Ctrl Pts',(31.7826622501159,31.2843061313282,0.765479387903577));
#34573=CARTESIAN_POINT('Ctrl Pts',(31.7348562317645,31.2917666379315,0.332966415952804));
#34574=CARTESIAN_POINT('Ctrl Pts',(31.6085484626321,31.3978213276647,-0.978922014709456));
#34575=CARTESIAN_POINT('Ctrl Pts',(31.6449008941903,31.6360823818921,-1.98636136652822));
#34576=CARTESIAN_POINT('Ctrl Pts',(31.949455744811,32.3637918611397,-3.81078790534844));
#34577=CARTESIAN_POINT('Ctrl Pts',(32.2252577802499,32.8768818719365,-4.65460264913809));
#34578=CARTESIAN_POINT('Ctrl Pts',(32.9506697646596,34.0936348201821,-6.05121512489433));
#34579=CARTESIAN_POINT('Ctrl Pts',(33.4089026594735,34.8172613800546,-6.61423873291092));
#34580=CARTESIAN_POINT('Ctrl Pts',(34.4150618219131,36.3546651861137,-7.37244739495311));
#34581=CARTESIAN_POINT('Ctrl Pts',(34.9808875866065,37.2044809779791,-7.56862230166205));
#34582=CARTESIAN_POINT('Ctrl Pts',(35.5267289204026,38.0218131772948,-7.57037421505979));
#34583=CARTESIAN_POINT('Ctrl Pts',(27.9017241322581,25.5825535213022,1.59647090706387));
#34584=CARTESIAN_POINT('Ctrl Pts',(27.8576356266577,25.5977646187872,1.15259179090232));
#34585=CARTESIAN_POINT('Ctrl Pts',(27.8006101679621,25.6076988465176,0.635573104328414));
#34586=CARTESIAN_POINT('Ctrl Pts',(27.6900511858084,25.7366398496321,-1.86858636179196));
#34587=CARTESIAN_POINT('Ctrl Pts',(27.8867543207108,26.066798081921,-3.71029995868804));
#34588=CARTESIAN_POINT('Ctrl Pts',(28.8018888878892,27.1980083507072,-7.16936247494692));
#34589=CARTESIAN_POINT('Ctrl Pts',(29.5148901762539,27.9765753734475,-8.73699595770123));
#34590=CARTESIAN_POINT('Ctrl Pts',(31.343025278964,29.8931745079276,-11.3730256982183));
#34591=CARTESIAN_POINT('Ctrl Pts',(32.4473861126917,31.0108564710822,-12.4235805193185));
#34592=CARTESIAN_POINT('Ctrl Pts',(34.8951191225769,33.4700709140672,-13.8529470820634));
#34593=CARTESIAN_POINT('Ctrl Pts',(36.212651592373,34.7723177498292,-14.220471855745));
#34594=CARTESIAN_POINT('Ctrl Pts',(37.5367254229124,36.0864498658149,-14.2198708430665));
#34595=CARTESIAN_POINT('Ctrl Pts',(27.8942941678687,24.6306899881718,1.62964634867146));
#34596=CARTESIAN_POINT('Ctrl Pts',(27.8505734813074,24.6457741833924,1.1894704015781));
#34597=CARTESIAN_POINT('Ctrl Pts',(27.7924691428913,24.6552631565739,0.664244065131922));
#34598=CARTESIAN_POINT('Ctrl Pts',(27.6812026446259,24.7842103148325,-1.9528790512907));
#34599=CARTESIAN_POINT('Ctrl Pts',(27.8909128870511,25.1246550797834,-3.87337387077626));
#34600=CARTESIAN_POINT('Ctrl Pts',(28.853265640495,26.2979391683251,-7.48792130214933));
#34601=CARTESIAN_POINT('Ctrl Pts',(29.6017140577639,27.1064590437666,-9.1236083623074));
#34602=CARTESIAN_POINT('Ctrl Pts',(31.5183666698576,29.1001001804498,-11.8774049927236));
#34603=CARTESIAN_POINT('Ctrl Pts',(32.6750275473655,30.2623381498283,-12.9732563609205));
#34604=CARTESIAN_POINT('Ctrl Pts',(35.2391241078866,32.8235411739476,-14.4676858045142));
#34605=CARTESIAN_POINT('Ctrl Pts',(36.6172542487155,34.1773627941932,-14.8501851005341));
#34606=CARTESIAN_POINT('Ctrl Pts',(38.0044776097607,35.5466255754747,-14.8499483202527));
#34607=CARTESIAN_POINT('Ctrl Pts',(28.518207957172,23.9110153591927,1.62975553161122));
#34608=CARTESIAN_POINT('Ctrl Pts',(28.4744932159205,23.9260975032119,1.18963944139232));
#34609=CARTESIAN_POINT('Ctrl Pts',(28.4163403666156,23.9355515973761,0.664246507202821));
#34610=CARTESIAN_POINT('Ctrl Pts',(28.3045391652058,24.0640354326903,-1.95288623098466));
#34611=CARTESIAN_POINT('Ctrl Pts',(28.5150692335159,24.4051905243397,-3.87317034518165));
#34612=CARTESIAN_POINT('Ctrl Pts',(29.4765070006746,25.5776818931087,-7.48823335804822));
#34613=CARTESIAN_POINT('Ctrl Pts',(30.2255166845004,26.386688032904,-9.12349227711924));
#34614=CARTESIAN_POINT('Ctrl Pts',(32.1419665196151,28.3801534903142,-11.8775764776501));
#34615=CARTESIAN_POINT('Ctrl Pts',(33.2989594624334,29.5426791468127,-12.9726927515002));
#34616=CARTESIAN_POINT('Ctrl Pts',(35.8626855589669,32.1035612317429,-14.4683433355361));
#34617=CARTESIAN_POINT('Ctrl Pts',(37.2410591163412,33.4576026588985,-14.8498038984768));
#34618=CARTESIAN_POINT('Ctrl Pts',(38.628213118051,34.8267964255888,-14.8500516281495));
#34619=CARTESIAN_POINT('Ctrl Pts',(29.4615086055164,23.7833669488543,1.59674386441327));
#34620=CARTESIAN_POINT('Ctrl Pts',(29.4174349631896,23.7985729183272,1.15301439043766));
#34621=CARTESIAN_POINT('Ctrl Pts',(29.3602882272755,23.8084199485255,0.63557920950567));
#34622=CARTESIAN_POINT('Ctrl Pts',(29.248392487251,23.9362026442694,-1.86860431102687));
#34623=CARTESIAN_POINT('Ctrl Pts',(29.447145186874,24.2681366933022,-3.70979114470513));
#34624=CARTESIAN_POINT('Ctrl Pts',(30.3599922883371,25.3973651626758,-7.17014261469054));
#34625=CARTESIAN_POINT('Ctrl Pts',(31.0743967430845,26.1771478462959,-8.73670574472719));
#34626=CARTESIAN_POINT('Ctrl Pts',(32.9020249033686,28.0933077825839,-11.373454410538));
#34627=CARTESIAN_POINT('Ctrl Pts',(34.0072159003542,29.2117089635432,-12.422171495751));
#34628=CARTESIAN_POINT('Ctrl Pts',(36.4540227502848,31.6701210585555,-13.8545909096349));
#34629=CARTESIAN_POINT('Ctrl Pts',(37.7721633453246,32.9729180118925,-14.2195188098725));
#34630=CARTESIAN_POINT('Ctrl Pts',(39.0960641936379,34.2868769911002,-14.2201291128085));
#34631=CARTESIAN_POINT('Ctrl Pts',(27.7725495286739,25.6404249706856,0.));
#34632=CARTESIAN_POINT('Ctrl Pts',(27.6900511858084,25.7366398496321,-1.86858636179196));
#34633=CARTESIAN_POINT('Ctrl Pts',(27.8867543207108,26.066798081921,-3.71029995868804));
#34634=CARTESIAN_POINT('Ctrl Pts',(28.8018888878892,27.1980083507072,-7.16936247494692));
#34635=CARTESIAN_POINT('Ctrl Pts',(29.5148901762515,27.9765753734499,-8.73699595769884));
#34636=CARTESIAN_POINT('Ctrl Pts',(30.5219411006583,29.0323578083609,-10.1890856763493));
#34637=CARTESIAN_POINT('Ctrl Pts',(30.6168936176608,29.1314899559103,-10.3203928635164));
#34638=CARTESIAN_POINT('Ctrl Pts',(30.7137407645493,29.2322214279229,-10.4488603766001));
#34639=CARTESIAN_POINT('Ctrl Pts',(29.3318883095343,23.8408520862197,1.66533453693773E-15));
#34640=CARTESIAN_POINT('Ctrl Pts',(29.248392487251,23.9362026442694,-1.86860431102687));
#34641=CARTESIAN_POINT('Ctrl Pts',(29.447145186874,24.2681366933022,-3.70979114470513));
#34642=CARTESIAN_POINT('Ctrl Pts',(30.3599922883371,25.3973651626758,-7.17014261469054));
#34643=CARTESIAN_POINT('Ctrl Pts',(31.0743967430845,26.1771478462959,-8.73670574472719));
#34644=CARTESIAN_POINT('Ctrl Pts',(32.0863072351869,27.238076095385,-10.1966053555739));
#34645=CARTESIAN_POINT('Ctrl Pts',(32.1866090102694,27.3427718639805,-10.3350231942301));
#34646=CARTESIAN_POINT('Ctrl Pts',(32.2890256406393,27.4492538662307,-10.4702558451018));
#34647=CARTESIAN_POINT('Ctrl Pts',(31.439445989728,31.6397608122765,1.24689105568327));
#34648=CARTESIAN_POINT('Ctrl Pts',(31.3915079136658,31.6563000607303,0.76425480955427));
#34649=CARTESIAN_POINT('Ctrl Pts',(31.3456016608091,31.6707408106671,0.332948724815391));
#34650=CARTESIAN_POINT('Ctrl Pts',(31.2395462388519,31.7970479454231,-0.978870002725275));
#34651=CARTESIAN_POINT('Ctrl Pts',(31.3034976581799,32.0225645221549,-1.98783577087666));
#34652=CARTESIAN_POINT('Ctrl Pts',(31.7151448889925,32.7052670087094,-3.80852727284797));
#34653=CARTESIAN_POINT('Ctrl Pts',(32.057093985311,33.1703611269161,-4.6554436072416));
#34654=CARTESIAN_POINT('Ctrl Pts',(32.9497533017817,34.2727650719351,-6.04997283341119));
#34655=CARTESIAN_POINT('Ctrl Pts',(33.5038992562213,34.9217287193948,-6.61832169924966));
#34656=CARTESIAN_POINT('Ctrl Pts',(34.7212963025802,36.3026175785815,-7.36768403056607));
#34657=CARTESIAN_POINT('Ctrl Pts',(35.4005693947338,37.0616291371886,-7.57138648705115));
#34658=CARTESIAN_POINT('Ctrl Pts',(36.0576472036359,37.7934972961793,-7.56962581969384));
#34659=CARTESIAN_POINT('Ctrl Pts',(30.6671178491337,29.4001542854015,1.35489343606325));
#34660=CARTESIAN_POINT('Ctrl Pts',(30.6203715276499,29.4162823633067,0.884255668139386));
#34661=CARTESIAN_POINT('Ctrl Pts',(30.5710069006797,29.4293136556717,0.42639701777831));
#34662=CARTESIAN_POINT('Ctrl Pts',(30.4632865154137,29.5561964051748,-1.25360819503402));
#34663=CARTESIAN_POINT('Ctrl Pts',(30.5686507750139,29.8143895731083,-2.5196091277888));
#34664=CARTESIAN_POINT('Ctrl Pts',(31.1352998840349,30.6351795888019,-4.84647586783175));
#34665=CARTESIAN_POINT('Ctrl Pts',(31.5921137090151,31.1973201148293,-5.91572199047832));
#34666=CARTESIAN_POINT('Ctrl Pts',(32.773533507375,32.5510483450333,-7.69376028690839));
#34667=CARTESIAN_POINT('Ctrl Pts',(33.4977500490821,33.344894581043,-8.41063186571964));
#34668=CARTESIAN_POINT('Ctrl Pts',(35.0948710912443,35.0585937299385,-9.37059840604598));
#34669=CARTESIAN_POINT('Ctrl Pts',(35.9713447024329,35.9854803114778,-9.62435378637997));
#34670=CARTESIAN_POINT('Ctrl Pts',(36.8343596268993,36.8970924436848,-9.62320046360512));
#34671=CARTESIAN_POINT('Ctrl Pts',(29.4725749263796,27.3548849305452,1.47293214974065));
#34672=CARTESIAN_POINT('Ctrl Pts',(29.4271284462509,27.3705645465863,1.01538106787412));
#34673=CARTESIAN_POINT('Ctrl Pts',(29.3740093215553,27.3820741720646,0.528580803096777));
#34674=CARTESIAN_POINT('Ctrl Pts',(29.2647682695535,27.5098462703966,-1.55402875459203));
#34675=CARTESIAN_POINT('Ctrl Pts',(29.4149573143405,27.8033726143444,-3.10121432122795));
#34676=CARTESIAN_POINT('Ctrl Pts',(30.1516133539766,28.7756052302924,-5.98129145451597));
#34677=CARTESIAN_POINT('Ctrl Pts',(30.7337162174557,29.4435926416019,-7.29389406576238));
#34678=CARTESIAN_POINT('Ctrl Pts',(32.2310076487024,31.0722410437258,-9.49113593804398));
#34679=CARTESIAN_POINT('Ctrl Pts',(33.1410090871746,32.0243541445035,-10.3708286018225));
#34680=CARTESIAN_POINT('Ctrl Pts',(35.153563896332,34.1021594177494,-11.5604045560192));
#34681=CARTESIAN_POINT('Ctrl Pts',(36.2455537133318,35.2124714377622,-11.8694761542139));
#34682=CARTESIAN_POINT('Ctrl Pts',(37.333783405879,36.3206928540896,-11.868714228481));
#34683=CARTESIAN_POINT('Ctrl Pts',(27.9017241322581,25.5825535213022,1.59647090706387));
#34684=CARTESIAN_POINT('Ctrl Pts',(27.8576356266577,25.5977646187872,1.15259179090232));
#34685=CARTESIAN_POINT('Ctrl Pts',(27.8006101679621,25.6076988465176,0.635573104328414));
#34686=CARTESIAN_POINT('Ctrl Pts',(27.6900511858084,25.7366398496321,-1.86858636179196));
#34687=CARTESIAN_POINT('Ctrl Pts',(27.8867543207108,26.066798081921,-3.71029995868804));
#34688=CARTESIAN_POINT('Ctrl Pts',(28.8018888878892,27.1980083507072,-7.16936247494692));
#34689=CARTESIAN_POINT('Ctrl Pts',(29.5148901762515,27.9765753734499,-8.73699595769884));
#34690=CARTESIAN_POINT('Ctrl Pts',(31.3430252789664,29.8931745079252,-11.3730256982207));
#34691=CARTESIAN_POINT('Ctrl Pts',(32.4473861126964,31.0108564710774,-12.4235805193185));
#34692=CARTESIAN_POINT('Ctrl Pts',(34.8951191225721,33.4700709140719,-13.8529470820634));
#34693=CARTESIAN_POINT('Ctrl Pts',(36.212651592373,34.7723177498292,-14.220471855726));
#34694=CARTESIAN_POINT('Ctrl Pts',(37.5367254229124,36.0864498658149,-14.2198708430665));
#34695=CARTESIAN_POINT('Ctrl Pts',(29.4615086055164,23.7833669488543,1.59674386441327));
#34696=CARTESIAN_POINT('Ctrl Pts',(29.4174349631896,23.7985729183272,1.15301439043765));
#34697=CARTESIAN_POINT('Ctrl Pts',(29.3602882272755,23.8084199485255,0.63557920950567));
#34698=CARTESIAN_POINT('Ctrl Pts',(29.248392487251,23.9362026442694,-1.86860431102687));
#34699=CARTESIAN_POINT('Ctrl Pts',(29.447145186874,24.2681366933022,-3.70979114470393));
#34700=CARTESIAN_POINT('Ctrl Pts',(30.3599922883371,25.3973651626758,-7.17014261469174));
#34701=CARTESIAN_POINT('Ctrl Pts',(31.0743967430845,26.1771478463006,-8.7367057447272));
#34702=CARTESIAN_POINT('Ctrl Pts',(32.9020249033686,28.0933077825791,-11.373454410538));
#34703=CARTESIAN_POINT('Ctrl Pts',(34.0072159003542,29.2117089635455,-12.4221714957558));
#34704=CARTESIAN_POINT('Ctrl Pts',(36.4540227502848,31.6701210585531,-13.8545909096301));
#34705=CARTESIAN_POINT('Ctrl Pts',(37.7721633453302,32.9729180118886,-14.2195188098868));
#34706=CARTESIAN_POINT('Ctrl Pts',(39.0960641936379,34.2868769911002,-14.2201291128085));
#34707=CARTESIAN_POINT('Ctrl Pts',(31.4387285991345,25.0869579521467,1.47327622041466));
#34708=CARTESIAN_POINT('Ctrl Pts',(31.3933008545913,25.1026311041785,1.01591376687384));
#34709=CARTESIAN_POINT('Ctrl Pts',(31.3400288564412,25.1140308146322,0.52858849885019));
#34710=CARTESIAN_POINT('Ctrl Pts',(31.2291027822745,25.240342832856,-1.55405138012444));
#34711=CARTESIAN_POINT('Ctrl Pts',(31.3818753629811,25.5361076454315,-3.10057294640994));
#34712=CARTESIAN_POINT('Ctrl Pts',(32.1156479855831,26.5058421456039,-5.98227484334299));
#34713=CARTESIAN_POINT('Ctrl Pts',(32.6995195810716,27.175361932793,-7.29352824387175));
#34714=CARTESIAN_POINT('Ctrl Pts',(34.1961719966689,28.8034567128308,-9.49167634238618));
#34715=CARTESIAN_POINT('Ctrl Pts',(35.1072198800537,29.7564764085591,-10.3690524866583));
#34716=CARTESIAN_POINT('Ctrl Pts',(37.1186072376635,31.8332702988585,-11.5624766484565));
#34717=CARTESIAN_POINT('Ctrl Pts',(38.2113611019924,32.9442792642618,-11.8682745704453));
#34718=CARTESIAN_POINT('Ctrl Pts',(39.2993752576344,34.0522789304535,-11.869039784999));
#34719=CARTESIAN_POINT('Ctrl Pts',(33.6327571359872,25.9793365537797,1.35541241355847));
#34720=CARTESIAN_POINT('Ctrl Pts',(33.5860390742467,25.9954548817286,0.885059162344105));
#34721=CARTESIAN_POINT('Ctrl Pts',(33.5364438612611,26.0083203842444,0.426408625634281));
#34722=CARTESIAN_POINT('Ctrl Pts',(33.4261818802043,26.1330008283034,-1.2536423221568));
#34723=CARTESIAN_POINT('Ctrl Pts',(33.5354430048848,26.3945703805904,-2.51864171288876));
#34724=CARTESIAN_POINT('Ctrl Pts',(34.0977429244508,27.2115923743002,-4.84795915806537));
#34725=CARTESIAN_POINT('Ctrl Pts',(34.5572246086239,27.776044252781,-5.91517020463262));
#34726=CARTESIAN_POINT('Ctrl Pts',(35.7376805505017,29.1289374295172,-7.6945754034308));
#34727=CARTESIAN_POINT('Ctrl Pts',(36.4634754928303,29.9241511240645,-8.40795287018175));
#34728=CARTESIAN_POINT('Ctrl Pts',(38.0588356145493,31.6363247579131,-9.37372383760818));
#34729=CARTESIAN_POINT('Ctrl Pts',(38.9364560608935,32.5642699125464,-9.62254085985904));
#34730=CARTESIAN_POINT('Ctrl Pts',(39.799151493507,33.4755402303452,-9.62369151535412));
#34731=CARTESIAN_POINT('Ctrl Pts',(35.9592765491248,26.4262081762391,1.24768201173545));
#34732=CARTESIAN_POINT('Ctrl Pts',(35.9113815427739,26.4427325651126,0.765479387903452));
#34733=CARTESIAN_POINT('Ctrl Pts',(35.8651238615809,26.4569206403468,0.332966415956187));
#34734=CARTESIAN_POINT('Ctrl Pts',(35.7551948793994,26.5798713158462,-0.97892201471915));
#34735=CARTESIAN_POINT('Ctrl Pts',(35.8250853790549,26.8105337258072,-1.98636136654047));
#34736=CARTESIAN_POINT('Ctrl Pts',(36.2301041572592,27.4874934974547,-3.81078790533667));
#34737=CARTESIAN_POINT('Ctrl Pts',(36.5761192475709,27.9561102697751,-4.6546026490906));
#34738=CARTESIAN_POINT('Ctrl Pts',(37.467309582976,29.0572415380629,-6.05121512494251));
#34739=CARTESIAN_POINT('Ctrl Pts',(38.0238611244248,29.7082892828337,-6.61423873273877));
#34740=CARTESIAN_POINT('Ctrl Pts',(39.2385744114853,31.0868531561125,-7.3724473951262));
#34741=CARTESIAN_POINT('Ctrl Pts',(39.9195822826463,31.8474936466127,-7.56862230151042));
#34742=CARTESIAN_POINT('Ctrl Pts',(40.5761862384902,32.578825261391,-7.57037421506047));
#34743=CARTESIAN_POINT('Ctrl Pts',(31.2585017743465,21.3513306581892,1.59647086199721));
#34744=CARTESIAN_POINT('Ctrl Pts',(31.2170267923954,21.3726613764951,1.15259176008521));
#34745=CARTESIAN_POINT('Ctrl Pts',(31.1619955607637,21.3906100567509,0.635573083900845));
#34746=CARTESIAN_POINT('Ctrl Pts',(31.0709121284139,21.5339728087887,-1.86858636186358));
#34747=CARTESIAN_POINT('Ctrl Pts',(31.312599524452,21.8327767315482,-3.71029995871917));
#34748=CARTESIAN_POINT('Ctrl Pts',(32.3794073476761,22.8222356829394,-7.1693624749162));
#34749=CARTESIAN_POINT('Ctrl Pts',(33.1959529509213,23.4914073529601,-8.73699595768941));
#34750=CARTESIAN_POINT('Ctrl Pts',(35.2782407701143,25.1283275202519,-11.3730256982305));
#34751=CARTESIAN_POINT('Ctrl Pts',(36.5304235306165,26.0774661593887,-12.4235805192369));
#34752=CARTESIAN_POINT('Ctrl Pts',(39.303224853761,28.1633006173233,-13.8529470821455));
#34753=CARTESIAN_POINT('Ctrl Pts',(40.7926757902182,29.2647880382365,-14.2204718556216));
#34754=CARTESIAN_POINT('Ctrl Pts',(42.2902929581068,30.3771088306738,-14.2198708430667));
#34755=CARTESIAN_POINT('Ctrl Pts',(31.1156831315058,20.4102131175327,1.62964630360479));
#34756=CARTESIAN_POINT('Ctrl Pts',(31.0745541646295,20.431365879152,1.18947037063688));
#34757=CARTESIAN_POINT('Ctrl Pts',(31.0183916683982,20.4490273774992,0.664244043783199));
#34758=CARTESIAN_POINT('Ctrl Pts',(30.9266087974273,20.5924969120704,-1.95287905136656));
#34759=CARTESIAN_POINT('Ctrl Pts',(31.1826348335975,20.8996315610168,-3.87337387080978));
#34760=CARTESIAN_POINT('Ctrl Pts',(32.3021679589004,21.9240162328045,-7.48792130211613));
#34761=CARTESIAN_POINT('Ctrl Pts',(33.1580626257629,22.6177912262544,-9.12360836230029));
#34762=CARTESIAN_POINT('Ctrl Pts',(35.3389311938233,24.3183718642228,-11.877404992731));
#34763=CARTESIAN_POINT('Ctrl Pts',(36.6492226398428,25.3041699214331,-12.9732563608915));
#34764=CARTESIAN_POINT('Ctrl Pts',(39.5517175889713,27.4743946038673,-14.4676858045434));
#34765=CARTESIAN_POINT('Ctrl Pts',(41.1084892565448,28.6183079046667,-14.8501851005199));
#34766=CARTESIAN_POINT('Ctrl Pts',(42.6764590955603,29.7762110964235,-14.8499483202528));
#34767=CARTESIAN_POINT('Ctrl Pts',(31.6308259996108,19.6090715485702,1.62975548654455));
#34768=CARTESIAN_POINT('Ctrl Pts',(31.5897026256139,19.6302214337507,1.18963941044875));
#34769=CARTESIAN_POINT('Ctrl Pts',(31.5334871484553,19.6478553119239,0.664246485850905));
#34770=CARTESIAN_POINT('Ctrl Pts',(31.4411090791311,19.7909423357087,-1.95288623105134));
#34771=CARTESIAN_POINT('Ctrl Pts',(31.6980476865711,20.0986634078557,-3.8731703452115));
#34772=CARTESIAN_POINT('Ctrl Pts',(32.816562323028,21.1223936447507,-7.48823335801853));
#34773=CARTESIAN_POINT('Ctrl Pts',(33.6730817462005,21.8165700765197,-9.1234922771144));
#34774=CARTESIAN_POINT('Ctrl Pts',(35.8537245994984,23.5170056815502,-11.877576477655));
#34775=CARTESIAN_POINT('Ctrl Pts',(37.1643856729968,24.5030412398075,-12.9726927515238));
#34776=CARTESIAN_POINT('Ctrl Pts',(40.0664682545742,26.6730009722967,-14.4683433355124));
#34777=CARTESIAN_POINT('Ctrl Pts',(41.6235121428062,27.8170972008726,-14.8498038985718));
#34778=CARTESIAN_POINT('Ctrl Pts',(43.191403506678,28.9749419513879,-14.8500516281495));
#34779=CARTESIAN_POINT('Ctrl Pts',(32.5463589446091,19.348476735783,1.5967438193466));
#34780=CARTESIAN_POINT('Ctrl Pts',(32.5048979448445,19.3698002629923,1.15301435961605));
#34781=CARTESIAN_POINT('Ctrl Pts',(32.4497342609043,19.3876798928093,0.635579189070094));
#34782=CARTESIAN_POINT('Ctrl Pts',(32.3571628326792,19.5300863678938,-1.86860431107553));
#34783=CARTESIAN_POINT('Ctrl Pts',(32.6011316568668,19.8303563486502,-3.70979114472406));
#34784=CARTESIAN_POINT('Ctrl Pts',(33.6653932580141,20.8181792128001,-7.1701426146716));
#34785=CARTESIAN_POINT('Ctrl Pts',(34.4835007520102,21.4883544786281,-8.73670574472706));
#34786=CARTESIAN_POINT('Ctrl Pts',(36.5652242843068,23.1249120635655,-11.373454410538));
#34787=CARTESIAN_POINT('Ctrl Pts',(37.818331113499,24.0746444553115,-12.4221714958225));
#34788=CARTESIAN_POINT('Ctrl Pts',(40.5901015177707,26.1598165384099,-13.8545909095632));
#34789=CARTESIAN_POINT('Ctrl Pts',(42.0802326794091,27.2617619321778,-14.2195188100673));
#34790=CARTESIAN_POINT('Ctrl Pts',(43.5776539859011,28.3739359680848,-14.2201291128083));
#34791=CARTESIAN_POINT('Ctrl Pts',(31.1388779521431,21.4269965203138,0.));
#34792=CARTESIAN_POINT('Ctrl Pts',(31.0709121284139,21.5339728087887,-1.86858636186358));
#34793=CARTESIAN_POINT('Ctrl Pts',(31.312599524452,21.8327767315482,-3.71029995871917));
#34794=CARTESIAN_POINT('Ctrl Pts',(32.3794073476761,22.8222356829394,-7.1693624749162));
#34795=CARTESIAN_POINT('Ctrl Pts',(33.1959529509165,23.4914073529577,-8.73699595768941));
#34796=CARTESIAN_POINT('Ctrl Pts',(34.3430070554486,24.3931251555465,-10.18908567635));
#34797=CARTESIAN_POINT('Ctrl Pts',(34.4511010682837,24.4777351286714,-10.3203928635166));
#34798=CARTESIAN_POINT('Ctrl Pts',(34.5612980340057,24.5636585134986,-10.4488603765991));
#34799=CARTESIAN_POINT('Ctrl Pts',(32.4262389885814,19.4238236466306,2.77555756156289E-16));
#34800=CARTESIAN_POINT('Ctrl Pts',(32.3571628326792,19.5300863678938,-1.86860431107553));
#34801=CARTESIAN_POINT('Ctrl Pts',(32.6011316568668,19.8303563486502,-3.70979114472406));
#34802=CARTESIAN_POINT('Ctrl Pts',(33.6653932580141,20.8181792128001,-7.1701426146716));
#34803=CARTESIAN_POINT('Ctrl Pts',(34.4835007520102,21.4883544786281,-8.73670574472706));
#34804=CARTESIAN_POINT('Ctrl Pts',(35.636097286559,22.3944741298323,-10.1966053555735));
#34805=CARTESIAN_POINT('Ctrl Pts',(35.7502778955686,22.4838298155642,-10.3350231942303));
#34806=CARTESIAN_POINT('Ctrl Pts',(35.8668060412402,22.5746525783813,-10.4702558451031));
#34807=CARTESIAN_POINT('Ctrl Pts',(35.6222452002842,26.8434139987111,1.24689101061669));
#34808=CARTESIAN_POINT('Ctrl Pts',(35.577148846646,26.8666072002712,0.764254780048341));
#34809=CARTESIAN_POINT('Ctrl Pts',(35.5337649883011,26.8874341048554,0.332948714093336));
#34810=CARTESIAN_POINT('Ctrl Pts',(35.4467644377115,27.0275488741943,-0.978870002701186));
#34811=CARTESIAN_POINT('Ctrl Pts',(35.5421592789952,27.241668781443,-1.98783577088219));
#34812=CARTESIAN_POINT('Ctrl Pts',(36.0467752285198,27.8588388319605,-3.80852727284291));
#34813=CARTESIAN_POINT('Ctrl Pts',(36.45143357029,28.2705345323201,-4.6554436072276));
#34814=CARTESIAN_POINT('Ctrl Pts',(37.491895341187,29.234678928466,-6.04997283342596));
#34815=CARTESIAN_POINT('Ctrl Pts',(38.1327580455662,29.7981738697163,-6.6183216990295));
#34816=CARTESIAN_POINT('Ctrl Pts',(39.5342847195712,30.99175360786,-7.36768403078741));
#34817=CARTESIAN_POINT('Ctrl Pts',(40.3146623988312,31.6463688825513,-7.57138648665175));
#34818=CARTESIAN_POINT('Ctrl Pts',(41.0692078014242,32.2772757571271,-7.56962581969453));
#34819=CARTESIAN_POINT('Ctrl Pts',(34.5390490058878,24.7365171914564,1.35489339099665));
#34820=CARTESIAN_POINT('Ctrl Pts',(34.4950737607895,24.7591338032453,0.884255638226709));
#34821=CARTESIAN_POINT('Ctrl Pts',(34.4480661428698,24.7790577744548,0.426397004057655));
#34822=CARTESIAN_POINT('Ctrl Pts',(34.3594994944659,24.9199792485653,-1.25360819503478));
#34823=CARTESIAN_POINT('Ctrl Pts',(34.5005360167875,25.1605494847776,-2.51960912779922));
#34824=CARTESIAN_POINT('Ctrl Pts',(35.1782280532683,25.89234246528,-4.84647586782171));
#34825=CARTESIAN_POINT('Ctrl Pts',(35.7103931102114,26.3837498256795,-5.91572199046418));
#34826=CARTESIAN_POINT('Ctrl Pts',(37.0724433726659,27.5555654868626,-7.69376028692305));
#34827=CARTESIAN_POINT('Ctrl Pts',(37.9022645329909,28.238264752807,-8.41063186556637));
#34828=CARTESIAN_POINT('Ctrl Pts',(39.727014002825,29.7072268925279,-9.37059840620004));
#34829=CARTESIAN_POINT('Ctrl Pts',(40.7264760905888,30.4999439048231,-9.62435378614244));
#34830=CARTESIAN_POINT('Ctrl Pts',(41.7104427005356,31.27945731062,-9.62320046360557));
#34831=CARTESIAN_POINT('Ctrl Pts',(33.0655926302368,22.88206691246,1.47293210467401));
#34832=CARTESIAN_POINT('Ctrl Pts',(33.0228401731551,22.904054640381,1.0153810375198));
#34833=CARTESIAN_POINT('Ctrl Pts',(32.9718997171366,22.9230067538168,0.528580786098969));
#34834=CARTESIAN_POINT('Ctrl Pts',(32.8819544477726,23.0650249378754,-1.55402875462511));
#34835=CARTESIAN_POINT('Ctrl Pts',(33.0723879388185,23.3341894772782,-3.1012143212481));
#34836=CARTESIAN_POINT('Ctrl Pts',(33.9399090096248,24.191689081893,-5.98129145449616));
#34837=CARTESIAN_POINT('Ctrl Pts',(34.6111514256731,24.7700354696468,-7.29389406575296));
#34838=CARTESIAN_POINT('Ctrl Pts',(36.3249834230628,26.1690197914561,-9.49113593805381));
#34839=CARTESIAN_POINT('Ctrl Pts',(37.3612221809303,26.981935046264,-10.3708286017266));
#34840=CARTESIAN_POINT('Ctrl Pts',(39.6489946054353,28.7521748453928,-11.5604045561156));
#34841=CARTESIAN_POINT('Ctrl Pts',(40.8878834161031,29.6957791360353,-11.869476154081));
#34842=CARTESIAN_POINT('Ctrl Pts',(42.1227528511812,30.6378492234117,-11.8687142284813));
#34843=CARTESIAN_POINT('Ctrl Pts',(31.2585017743465,21.3513306581892,1.59647086199721));
#34844=CARTESIAN_POINT('Ctrl Pts',(31.2170267923954,21.3726613764951,1.15259176008522));
#34845=CARTESIAN_POINT('Ctrl Pts',(31.1619955607637,21.3906100567509,0.635573083900845));
#34846=CARTESIAN_POINT('Ctrl Pts',(31.0709121284139,21.5339728087887,-1.86858636186358));
#34847=CARTESIAN_POINT('Ctrl Pts',(31.312599524452,21.8327767315482,-3.71029995871917));
#34848=CARTESIAN_POINT('Ctrl Pts',(32.3794073476761,22.8222356829394,-7.1693624749162));
#34849=CARTESIAN_POINT('Ctrl Pts',(33.1959529509165,23.4914073529577,-8.73699595768941));
#34850=CARTESIAN_POINT('Ctrl Pts',(35.2782407701191,25.1283275202542,-11.3730256982305));
#34851=CARTESIAN_POINT('Ctrl Pts',(36.5304235306164,26.0774661593863,-12.4235805192369));
#34852=CARTESIAN_POINT('Ctrl Pts',(39.303224853761,28.1633006173257,-13.8529470821455));
#34853=CARTESIAN_POINT('Ctrl Pts',(40.7926757902106,29.264788038245,-14.2204718556263));
#34854=CARTESIAN_POINT('Ctrl Pts',(42.2902929581068,30.3771088306738,-14.2198708430667));
#34855=CARTESIAN_POINT('Ctrl Pts',(32.5463589446091,19.348476735783,1.5967438193466));
#34856=CARTESIAN_POINT('Ctrl Pts',(32.5048979448444,19.3698002629924,1.15301435961605));
#34857=CARTESIAN_POINT('Ctrl Pts',(32.4497342609043,19.3876798928093,0.635579189070094));
#34858=CARTESIAN_POINT('Ctrl Pts',(32.3571628326792,19.5300863678938,-1.86860431107553));
#34859=CARTESIAN_POINT('Ctrl Pts',(32.6011316568668,19.8303563486502,-3.70979114472526));
#34860=CARTESIAN_POINT('Ctrl Pts',(33.6653932580141,20.8181792128001,-7.1701426146704));
#34861=CARTESIAN_POINT('Ctrl Pts',(34.4835007520103,21.4883544786329,-8.73670574472945));
#34862=CARTESIAN_POINT('Ctrl Pts',(36.5652242843068,23.1249120635607,-11.3734544105356));
#34863=CARTESIAN_POINT('Ctrl Pts',(37.818331113499,24.0746444553139,-12.4221714958273));
#34864=CARTESIAN_POINT('Ctrl Pts',(40.5901015177707,26.1598165384076,-13.8545909095584));
#34865=CARTESIAN_POINT('Ctrl Pts',(42.080232679402,27.2617619321892,-14.2195188100863));
#34866=CARTESIAN_POINT('Ctrl Pts',(43.5776539859011,28.3739359680848,-14.2201291128083));
#34867=CARTESIAN_POINT('Ctrl Pts',(34.6889740324161,20.3574113186623,1.47327617534801));
#34868=CARTESIAN_POINT('Ctrl Pts',(34.6462392002948,20.3793899820061,1.01591373651327));
#34869=CARTESIAN_POINT('Ctrl Pts',(34.5951317842845,20.3982550553479,0.528588481842291));
#34870=CARTESIAN_POINT('Ctrl Pts',(34.5033108528571,20.5390678245046,-1.55405138012857));
#34871=CARTESIAN_POINT('Ctrl Pts',(34.6966201504081,20.8100803726295,-3.10057294641664));
#34872=CARTESIAN_POINT('Ctrl Pts',(35.5609316342745,21.665517641723,-5.98227484333611));
#34873=CARTESIAN_POINT('Ctrl Pts',(36.2341428590225,22.2451290911678,-7.29352824387633));
#34874=CARTESIAN_POINT('Ctrl Pts',(37.9472635563608,23.6436563673688,-9.49167634238129));
#34875=CARTESIAN_POINT('Ctrl Pts',(38.9846671296744,24.4573200646104,-10.3690524867537));
#34876=CARTESIAN_POINT('Ctrl Pts',(41.2711400509868,26.2267249209946,-11.5624766483606));
#34877=CARTESIAN_POINT('Ctrl Pts',(42.5108843176087,27.1709103277471,-11.8682745706876));
#34878=CARTESIAN_POINT('Ctrl Pts',(43.745508851356,28.1127915962416,-11.8690397849987));
#34879=CARTESIAN_POINT('Ctrl Pts',(36.9876692386614,20.928463976445,1.35541236849184));
#34880=CARTESIAN_POINT('Ctrl Pts',(36.9437205780947,20.9510669157118,0.885059132421862));
#34881=CARTESIAN_POINT('Ctrl Pts',(36.8964611268002,20.9708596003835,0.426408611898412));
#34882=CARTESIAN_POINT('Ctrl Pts',(36.8050653317411,21.109962892202,-1.2536423221139));
#34883=CARTESIAN_POINT('Ctrl Pts',(36.9504395642185,21.353320564284,-2.51864171287721));
#34884=CARTESIAN_POINT('Ctrl Pts',(37.6232904342718,22.082002830026,-4.84795915807652));
#34885=CARTESIAN_POINT('Ctrl Pts',(38.1584251352155,22.5753183406925,-5.91517020464188));
#34886=CARTESIAN_POINT('Ctrl Pts',(39.5194025113344,23.7464446191315,-7.694575403421));
#34887=CARTESIAN_POINT('Ctrl Pts',(40.3509806159645,24.4302727949463,-8.40795287032022));
#34888=CARTESIAN_POINT('Ctrl Pts',(42.1737699858116,25.8979755524313,-9.37372383746895));
#34889=CARTESIAN_POINT('Ctrl Pts',(43.1745178860489,26.691577151262,-9.62254086020588));
#34890=CARTESIAN_POINT('Ctrl Pts',(44.1581196109331,27.4707976903311,-9.62369151535367));
#34891=CARTESIAN_POINT('Ctrl Pts',(39.3541045014166,21.0396888561031,1.24768196666885));
#34892=CARTESIAN_POINT('Ctrl Pts',(39.3090486643696,21.0628612198304,0.76547935838156));
#34893=CARTESIAN_POINT('Ctrl Pts',(39.2652809952897,21.0834880350444,0.332966405210928));
#34894=CARTESIAN_POINT('Ctrl Pts',(39.1739686379382,21.2208317742353,-0.978922014628528));
#34895=CARTESIAN_POINT('Ctrl Pts',(39.2759744366035,21.4391999182347,-1.98636136650944));
#34896=CARTESIAN_POINT('Ctrl Pts',(39.7732121280721,22.0516290335747,-3.81078790536698));
#34897=CARTESIAN_POINT('Ctrl Pts',(40.1823964038332,22.4662328812349,-4.65460264910927));
#34898=CARTESIAN_POINT('Ctrl Pts',(41.2212230249773,23.4293266124464,-6.05121512492297));
#34899=CARTESIAN_POINT('Ctrl Pts',(41.8647634287383,23.9945420870636,-6.61423873296337));
#34900=CARTESIAN_POINT('Ctrl Pts',(43.2633027806486,25.1862024433187,-7.37244739490039));
#34901=CARTESIAN_POINT('Ctrl Pts',(44.0456294021745,25.8421831847417,-7.56862230200933));
#34902=CARTESIAN_POINT('Ctrl Pts',(44.7996294168197,26.47262641274,-7.57037421505979));
#34903=CARTESIAN_POINT('Ctrl Pts',(33.9789464595044,16.6854562787121,1.59647077610296));
#34904=CARTESIAN_POINT('Ctrl Pts',(33.940929313104,16.7124723847533,1.1525917013978));
#34905=CARTESIAN_POINT('Ctrl Pts',(33.8890125875519,16.7380701329784,0.635573044906332));
#34906=CARTESIAN_POINT('Ctrl Pts',(33.8192589011608,16.8929361805061,-1.8685863618215));
#34907=CARTESIAN_POINT('Ctrl Pts',(34.1010104999226,17.1543030074917,-3.71029995867386));
#34908=CARTESIAN_POINT('Ctrl Pts',(35.2977744483967,17.9818681105204,-7.16936247496116));
#34909=CARTESIAN_POINT('Ctrl Pts',(36.2012418527514,18.5280220223856,-8.73699595771064));
#34910=CARTESIAN_POINT('Ctrl Pts',(38.4952930132093,19.8519402483835,-11.373025698209));
#34911=CARTESIAN_POINT('Ctrl Pts',(39.8698068705931,20.6132138377451,-12.4235805192036));
#34912=CARTESIAN_POINT('Ctrl Pts',(42.9112302679695,22.283206736412,-13.8529470821785));
#34913=CARTESIAN_POINT('Ctrl Pts',(44.5422787457951,23.1615116341824,-14.2204718557499));
#34914=CARTESIAN_POINT('Ctrl Pts',(46.1829520838074,24.0493774600891,-14.2198708430666));
#34915=CARTESIAN_POINT('Ctrl Pts',(33.7036465139255,15.7742431696984,1.62964621771056));
#34916=CARTESIAN_POINT('Ctrl Pts',(33.6659465347851,15.8010338873333,1.18947031171078));
#34917=CARTESIAN_POINT('Ctrl Pts',(33.6128691890261,15.8265083724714,0.664244003030573));
#34918=CARTESIAN_POINT('Ctrl Pts',(33.5424383800233,15.9815796561337,-1.95287905132536));
#34919=CARTESIAN_POINT('Ctrl Pts',(33.8395682581975,16.2491518132771,-3.87337387076446));
#34920=CARTESIAN_POINT('Ctrl Pts',(35.0934912894487,17.1037835503796,-7.48792130216115));
#34921=CARTESIAN_POINT('Ctrl Pts',(36.0394086586928,17.6686904036902,-9.12360836231917));
#34922=CARTESIAN_POINT('Ctrl Pts',(38.440096987709,19.0415916252445,-11.877404992712));
#34923=CARTESIAN_POINT('Ctrl Pts',(39.8773452471315,19.8308817644926,-12.9732563608726));
#34924=CARTESIAN_POINT('Ctrl Pts',(43.0591521575499,21.5659485894108,-14.4676858045621));
#34925=CARTESIAN_POINT('Ctrl Pts',(44.7628739707833,22.4766667937664,-14.8501851005436));
#34926=CARTESIAN_POINT('Ctrl Pts',(46.4796709429185,23.3996388269522,-14.8499483202528));
#34927=CARTESIAN_POINT('Ctrl Pts',(34.0995316375869,14.9079435927952,1.62975540065032));
#34928=CARTESIAN_POINT('Ctrl Pts',(34.0618367850428,14.9347306673263,1.18963935151253));
#34929=CARTESIAN_POINT('Ctrl Pts',(34.0087030668513,14.9601853533851,0.664246445100363));
#34930=CARTESIAN_POINT('Ctrl Pts',(33.9376286808045,15.1149627252298,-1.95288623101673));
#34931=CARTESIAN_POINT('Ctrl Pts',(34.2357452982906,15.3829854641993,-3.87317034517582));
#34932=CARTESIAN_POINT('Ctrl Pts',(35.4885670716917,16.2371143736886,-7.48823335805401));
#34933=CARTESIAN_POINT('Ctrl Pts',(36.4351599687256,16.8023296671644,-9.12349227712854));
#34934=CARTESIAN_POINT('Ctrl Pts',(38.8356042401095,18.1751194545612,-11.8775764776408));
#34935=CARTESIAN_POINT('Ctrl Pts',(40.2732521646523,18.9645920739613,-12.9726927515338));
#34936=CARTESIAN_POINT('Ctrl Pts',(43.4546131985136,20.6994553317739,-14.4683433355024));
#34937=CARTESIAN_POINT('Ctrl Pts',(45.1586304949261,21.6103158609297,-14.8498038985005));
#34938=CARTESIAN_POINT('Ctrl Pts',(46.8753414736305,22.5332412158905,-14.8500516281495));
#34939=CARTESIAN_POINT('Ctrl Pts',(34.968659268658,14.5197073364541,1.59674373345235));
#34940=CARTESIAN_POINT('Ctrl Pts',(34.9306549387561,14.5467143347325,1.15301430090095));
#34941=CARTESIAN_POINT('Ctrl Pts',(34.8785972821206,14.5722625852625,0.635579150080806));
#34942=CARTESIAN_POINT('Ctrl Pts',(34.8072346530973,14.7263938532467,-1.86860431104991));
#34943=CARTESIAN_POINT('Ctrl Pts',(35.0914531001646,14.9888871347947,-3.70979114470167));
#34944=CARTESIAN_POINT('Ctrl Pts',(36.2854639039945,15.8151951687953,-7.17014261469392));
#34945=CARTESIAN_POINT('Ctrl Pts',(37.1906201278479,16.3621201810638,-8.73670574473169));
#34946=CARTESIAN_POINT('Ctrl Pts',(39.4840611441962,17.6857598216825,-11.3734544105334));
#34947=CARTESIAN_POINT('Ctrl Pts',(40.8595741643879,18.4474896114217,-12.4221714958565));
#34948=CARTESIAN_POINT('Ctrl Pts',(43.899882870386,20.1169735923147,-13.8545909095293));
#34949=CARTESIAN_POINT('Ctrl Pts',(45.5316698260147,20.9956349953166,-14.2195188099295));
#34950=CARTESIAN_POINT('Ctrl Pts',(47.1721284105873,21.8833834324346,-14.2201291128084));
#34951=CARTESIAN_POINT('Ctrl Pts',(33.8713086176154,16.777376211144,0.));
#34952=CARTESIAN_POINT('Ctrl Pts',(33.8192589011608,16.8929361805061,-1.8685863618215));
#34953=CARTESIAN_POINT('Ctrl Pts',(34.1010104999226,17.1543030074917,-3.71029995867386));
#34954=CARTESIAN_POINT('Ctrl Pts',(35.2977744483967,17.9818681105204,-7.16936247496116));
#34955=CARTESIAN_POINT('Ctrl Pts',(36.2012418527514,18.5280220223832,-8.73699595770825));
#34956=CARTESIAN_POINT('Ctrl Pts',(37.4649484236425,19.2573188185314,-10.1890856763496));
#34957=CARTESIAN_POINT('Ctrl Pts',(37.5839834499269,19.3256842021738,-10.3203928635159));
#34958=CARTESIAN_POINT('Ctrl Pts',(37.705286942044,19.3950503474818,-10.4488603765981));
#34959=CARTESIAN_POINT('Ctrl Pts',(34.8604849513724,14.611382171278,1.77635683940025E-15));
#34960=CARTESIAN_POINT('Ctrl Pts',(34.8072346530973,14.7263938532467,-1.86860431104991));
#34961=CARTESIAN_POINT('Ctrl Pts',(35.0914531001646,14.9888871347947,-3.70979114470167));
#34962=CARTESIAN_POINT('Ctrl Pts',(36.2854639039945,15.8151951687953,-7.17014261469392));
#34963=CARTESIAN_POINT('Ctrl Pts',(37.1906201278479,16.3621201810638,-8.73670574473169));
#34964=CARTESIAN_POINT('Ctrl Pts',(38.4604391631928,17.0949852513288,-10.1966053555733));
#34965=CARTESIAN_POINT('Ctrl Pts',(38.5861742182004,17.1671818301162,-10.3350231942304));
#34966=CARTESIAN_POINT('Ctrl Pts',(38.7144417021696,17.2404964639596,-10.4702558451038));
#34967=CARTESIAN_POINT('Ctrl Pts',(39.0798782217544,21.5006126898291,1.2468909247222));
#34968=CARTESIAN_POINT('Ctrl Pts',(39.0385416232006,21.5299876964993,0.764254723810705));
#34969=CARTESIAN_POINT('Ctrl Pts',(38.998563331349,21.5567767789524,0.332948693668265));
#34970=CARTESIAN_POINT('Ctrl Pts',(38.9323887327488,21.7078468488828,-0.978870002686299));
#34971=CARTESIAN_POINT('Ctrl Pts',(39.0572850320743,21.9062112228022,-1.98783577086007));
#34972=CARTESIAN_POINT('Ctrl Pts',(39.6445971746525,22.4452850348741,-3.80852727286476));
#34973=CARTESIAN_POINT('Ctrl Pts',(40.1037270850429,22.7952013801406,-4.6554436072369));
#34974=CARTESIAN_POINT('Ctrl Pts',(41.2708105091343,23.6014590278601,-6.0499728334163));
#34975=CARTESIAN_POINT('Ctrl Pts',(41.9853438467173,24.0680141309112,-6.61832169894315));
#34976=CARTESIAN_POINT('Ctrl Pts',(43.5424691073156,25.0499869064955,-7.36768403087327));
#34977=CARTESIAN_POINT('Ctrl Pts',(44.4080651338049,25.5868798186403,-7.57138648703229));
#34978=CARTESIAN_POINT('Ctrl Pts',(45.2447177621913,26.1039819636361,-7.56962581969415));
#34979=CARTESIAN_POINT('Ctrl Pts',(37.707864724394,19.5693159454017,1.35489330510224));
#34980=CARTESIAN_POINT('Ctrl Pts',(37.6675557657705,19.5979606808254,0.884255581228092));
#34981=CARTESIAN_POINT('Ctrl Pts',(37.6238620982185,19.6243717351804,0.426396977899622));
#34982=CARTESIAN_POINT('Ctrl Pts',(37.5562521484826,19.7764631777486,-1.25360819501488));
#34983=CARTESIAN_POINT('Ctrl Pts',(37.7300898366261,19.9945131659699,-2.5196091277746));
#34984=CARTESIAN_POINT('Ctrl Pts',(38.5050289449343,20.6224119165152,-4.8464758678461));
#34985=CARTESIAN_POINT('Ctrl Pts',(39.1017118879826,21.0330824745219,-5.91572199047591));
#34986=CARTESIAN_POINT('Ctrl Pts',(40.6166651989596,21.9991307790772,-7.69376028691107));
#34987=CARTESIAN_POINT('Ctrl Pts',(41.5351982120318,22.5567852866117,-8.41063186550891));
#34988=CARTESIAN_POINT('Ctrl Pts',(43.550429472638,23.7511065841766,-9.37059840625714));
#34989=CARTESIAN_POINT('Ctrl Pts',(44.6525338708088,24.3935165950095,-9.62435378637539));
#34990=CARTESIAN_POINT('Ctrl Pts',(45.7374214437733,25.0250626292171,-9.62320046360533));
#34991=CARTESIAN_POINT('Ctrl Pts',(35.9854902185572,17.9434360021527,1.47293201877968));
#34992=CARTESIAN_POINT('Ctrl Pts',(35.9463021021743,17.9712842340133,1.0153809796928));
#34993=CARTESIAN_POINT('Ctrl Pts',(35.8985773174017,17.9972930238834,0.528580753670798));
#34994=CARTESIAN_POINT('Ctrl Pts',(35.8297588571711,18.150666211701,-1.55402875459602));
#34995=CARTESIAN_POINT('Ctrl Pts',(36.0565601177425,18.3899895327227,-3.10121432121615));
#34996=CARTESIAN_POINT('Ctrl Pts',(37.0372859924633,19.1152999068356,-5.98129145452784));
#34997=CARTESIAN_POINT('Ctrl Pts',(37.7840034012197,19.5922318064067,-7.29389406576467));
#34998=CARTESIAN_POINT('Ctrl Pts',(39.6794872874942,20.7330727614611,-9.49113593804186));
#34999=CARTESIAN_POINT('Ctrl Pts',(40.8208685319567,21.3902415598895,-10.3708286016837));
#35000=CARTESIAN_POINT('Ctrl Pts',(43.3372861226234,22.8168789076785,-11.5604045561583));
#35001=CARTESIAN_POINT('Ctrl Pts',(44.6978537235956,23.5745664063952,-11.8694761542236));
#35002=CARTESIAN_POINT('Ctrl Pts',(46.0542245204214,24.3313073348067,-11.8687142284811));
#35003=CARTESIAN_POINT('Ctrl Pts',(33.9789464595044,16.6854562787121,1.59647077610296));
#35004=CARTESIAN_POINT('Ctrl Pts',(33.940929313104,16.7124723847533,1.1525917013978));
#35005=CARTESIAN_POINT('Ctrl Pts',(33.8890125875519,16.7380701329784,0.635573044906332));
#35006=CARTESIAN_POINT('Ctrl Pts',(33.8192589011608,16.8929361805061,-1.8685863618215));
#35007=CARTESIAN_POINT('Ctrl Pts',(34.1010104999226,17.1543030074917,-3.71029995867386));
#35008=CARTESIAN_POINT('Ctrl Pts',(35.2977744483967,17.9818681105204,-7.16936247496116));
#35009=CARTESIAN_POINT('Ctrl Pts',(36.2012418527514,18.5280220223832,-8.73699595770825));
#35010=CARTESIAN_POINT('Ctrl Pts',(38.4952930132093,19.8519402483859,-11.3730256982114));
#35011=CARTESIAN_POINT('Ctrl Pts',(39.8698068705931,20.6132138377451,-12.4235805192036));
#35012=CARTESIAN_POINT('Ctrl Pts',(42.9112302679695,22.283206736412,-13.8529470821785));
#35013=CARTESIAN_POINT('Ctrl Pts',(44.5422787457922,23.1615116341878,-14.2204718557499));
#35014=CARTESIAN_POINT('Ctrl Pts',(46.1829520838074,24.0493774600891,-14.2198708430666));
#35015=CARTESIAN_POINT('Ctrl Pts',(34.968659268658,14.5197073364541,1.59674373345235));
#35016=CARTESIAN_POINT('Ctrl Pts',(34.930654938756,14.5467143347324,1.15301430090095));
#35017=CARTESIAN_POINT('Ctrl Pts',(34.8785972821206,14.5722625852624,0.635579150080806));
#35018=CARTESIAN_POINT('Ctrl Pts',(34.8072346530973,14.7263938532467,-1.86860431104991));
#35019=CARTESIAN_POINT('Ctrl Pts',(35.0914531001646,14.9888871347947,-3.70979114470287));
#35020=CARTESIAN_POINT('Ctrl Pts',(36.2854639039945,15.8151951687953,-7.17014261469272));
#35021=CARTESIAN_POINT('Ctrl Pts',(37.1906201278479,16.3621201810662,-8.73670574473408));
#35022=CARTESIAN_POINT('Ctrl Pts',(39.4840611441962,17.6857598216801,-11.373454410531));
#35023=CARTESIAN_POINT('Ctrl Pts',(40.8595741643879,18.4474896114217,-12.4221714958565));
#35024=CARTESIAN_POINT('Ctrl Pts',(43.8998828703861,20.1169735923147,-13.8545909095293));
#35025=CARTESIAN_POINT('Ctrl Pts',(45.531669826027,20.9956349952939,-14.2195188099295));
#35026=CARTESIAN_POINT('Ctrl Pts',(47.1721284105873,21.8833834324346,-14.2201291128084));
#35027=CARTESIAN_POINT('Ctrl Pts',(37.2330519862578,15.2134465003399,1.47327608945368));
#35028=CARTESIAN_POINT('Ctrl Pts',(37.1938800254435,15.2412832516015,1.01591367865198));
#35029=CARTESIAN_POINT('Ctrl Pts',(37.1459775929436,15.2672296481878,0.528588449420692));
#35030=CARTESIAN_POINT('Ctrl Pts',(37.0751310137516,15.4196766250279,-1.55405138012023));
#35031=CARTESIAN_POINT('Ctrl Pts',(37.3050418083334,15.66041987477,-3.10057294641005));
#35032=CARTESIAN_POINT('Ctrl Pts',(38.2822972641785,16.3841456768374,-5.9822748433428));
#35033=CARTESIAN_POINT('Ctrl Pts',(39.0311434790186,16.8620495708873,-7.29352824387147));
#35034=CARTESIAN_POINT('Ctrl Pts',(40.9258582609005,18.0025393609562,-9.49167634238628));
#35035=CARTESIAN_POINT('Ctrl Pts',(42.0684989791267,18.6602832132252,-10.3690524867972));
#35036=CARTESIAN_POINT('Ctrl Pts',(44.5835114689155,20.0862790553768,-11.5624766483172));
#35037=CARTESIAN_POINT('Ctrl Pts',(45.9450085199795,20.8444200112153,-11.8682745704832));
#35038=CARTESIAN_POINT('Ctrl Pts',(47.3011100364939,21.6010088957268,-11.8690397849988));
#35039=CARTESIAN_POINT('Ctrl Pts',(39.5896190563862,15.4515482289399,1.35541228259744));
#35040=CARTESIAN_POINT('Ctrl Pts',(39.5493344659561,15.4801756476478,0.885059075370257));
#35041=CARTESIAN_POINT('Ctrl Pts',(39.5053728442213,15.5064925913696,0.426408585750303));
#35042=CARTESIAN_POINT('Ctrl Pts',(39.4347037901216,15.6571869876679,-1.25364232212529));
#35043=CARTESIAN_POINT('Ctrl Pts',(39.6132317302818,15.8773787191618,-2.51864171289602));
#35044=CARTESIAN_POINT('Ctrl Pts',(40.382936247472,16.5028873873876,-4.84795915805801));
#35045=CARTESIAN_POINT('Ctrl Pts',(40.9828301658549,16.9150240490132,-5.91517020462755));
#35046=CARTESIAN_POINT('Ctrl Pts',(42.4966234015924,17.8805426754076,-7.6945754034356));
#35047=CARTESIAN_POINT('Ctrl Pts',(43.4170561364029,18.4390645628875,-8.40795287039257));
#35048=CARTESIAN_POINT('Ctrl Pts',(45.4301680192463,19.6324182482204,-9.37372383739693));
#35049=CARTESIAN_POINT('Ctrl Pts',(46.5336710319636,20.2755208515651,-9.62254085992063));
#35050=CARTESIAN_POINT('Ctrl Pts',(47.6181557545822,20.9068289285805,-9.62369151535394));
#35051=CARTESIAN_POINT('Ctrl Pts',(41.9477963710449,15.2248621479927,1.24768188077437));
#35052=CARTESIAN_POINT('Ctrl Pts',(41.9064969112189,15.2542107628473,0.765479302065719));
#35053=CARTESIAN_POINT('Ctrl Pts',(41.8661102394687,15.2808564144635,0.332966384800994));
#35054=CARTESIAN_POINT('Ctrl Pts',(41.795273363349,15.4297972934032,-0.978922014661338));
#35055=CARTESIAN_POINT('Ctrl Pts',(41.9273179171871,15.6314258258285,-1.98636136655007));
#35056=CARTESIAN_POINT('Ctrl Pts',(42.5066521964225,16.1668569942609,-3.81078790532691));
#35057=CARTESIAN_POINT('Ctrl Pts',(42.9706758457638,16.5190077784711,-4.65460264908071));
#35058=CARTESIAN_POINT('Ctrl Pts',(44.1359912383933,17.3244581616248,-6.051215124952));
#35059=CARTESIAN_POINT('Ctrl Pts',(44.8534198776544,17.7923352091155,-6.61423873305977));
#35060=CARTESIAN_POINT('Ctrl Pts',(46.4073150662577,18.7728332796184,-7.37244739480456));
#35061=CARTESIAN_POINT('Ctrl Pts',(47.2750345238088,19.3108003965529,-7.56862230161463));
#35062=CARTESIAN_POINT('Ctrl Pts',(48.1110813316863,19.8275212310755,-7.57037421506018));
#35063=CARTESIAN_POINT('Ctrl Pts',(36.0076777827441,11.6799141290247,1.59647068126612));
#35064=CARTESIAN_POINT('Ctrl Pts',(35.9738923911208,11.7120656519291,1.152591636598));
#35065=CARTESIAN_POINT('Ctrl Pts',(35.9261470465084,11.7447913705166,0.635573001854836));
#35066=CARTESIAN_POINT('Ctrl Pts',(35.879143089373,11.9080080866873,-1.86858636178295));
#35067=CARTESIAN_POINT('Ctrl Pts',(36.1952232408275,12.126617143028,-3.71029995869426));
#35068=CARTESIAN_POINT('Ctrl Pts',(37.497580651705,12.7754415588947,-7.16936247494101));
#35069=CARTESIAN_POINT('Ctrl Pts',(38.4695778661834,13.1874595938719,-8.73699595767948));
#35070=CARTESIAN_POINT('Ctrl Pts',(40.9286921018507,14.1714247212918,-11.3730256982404));
#35071=CARTESIAN_POINT('Ctrl Pts',(42.397555917808,14.7293359258803,-12.4235805192179));
#35072=CARTESIAN_POINT('Ctrl Pts',(45.6456867795974,15.9494910258928,-13.8529470821646));
#35073=CARTESIAN_POINT('Ctrl Pts',(47.3851293551906,16.5867336459556,-14.2204718557025));
#35074=CARTESIAN_POINT('Ctrl Pts',(49.1354594857183,17.2320701170938,-14.2198708430667));
#35075=CARTESIAN_POINT('Ctrl Pts',(35.6055008474197,10.8171551228317,1.62964612287373));
#35076=CARTESIAN_POINT('Ctrl Pts',(35.5719973185988,10.849038413867,1.18947024665197));
#35077=CARTESIAN_POINT('Ctrl Pts',(35.5230856250742,10.8818072974761,0.664243958036444));
#35078=CARTESIAN_POINT('Ctrl Pts',(35.47544064564,11.0453235253574,-1.95287905128342));
#35079=CARTESIAN_POINT('Ctrl Pts',(35.8076256583526,11.2678861931943,-3.87337387078009));
#35080=CARTESIAN_POINT('Ctrl Pts',(37.1704123385812,11.9353671582151,-7.48792130214571));
#35081=CARTESIAN_POINT('Ctrl Pts',(38.1870962603493,12.3599059968478,-9.12360836229034));
#35082=CARTESIAN_POINT('Ctrl Pts',(40.7587332590659,13.3771794921454,-11.8774049927409));
#35083=CARTESIAN_POINT('Ctrl Pts',(42.2936801020575,13.9538940422629,-12.973256360882));
#35084=CARTESIAN_POINT('Ctrl Pts',(45.6900265604413,15.2184820528374,-14.4676858045529));
#35085=CARTESIAN_POINT('Ctrl Pts',(47.5060156561426,15.8774655648044,-14.8501851005246));
#35086=CARTESIAN_POINT('Ctrl Pts',(49.3366907261822,16.5467173899494,-14.8499483202528));
#35087=CARTESIAN_POINT('Ctrl Pts',(35.8740691471582,9.90333289917181,1.62975530581352));
#35088=CARTESIAN_POINT('Ctrl Pts',(35.8405701742713,9.93521185459246,1.18963928644524));
#35089=CARTESIAN_POINT('Ctrl Pts',(35.7915998644016,9.96796916327873,0.664246400106497));
#35090=CARTESIAN_POINT('Ctrl Pts',(35.7432760306146,10.1312860615133,-1.95288623097604));
#35091=CARTESIAN_POINT('Ctrl Pts',(36.076501863553,10.3541542972526,-3.87317034518541));
#35092=CARTESIAN_POINT('Ctrl Pts',(37.4381269352739,11.0212942780538,-7.48823335804453));
#35093=CARTESIAN_POINT('Ctrl Pts',(38.4555234045685,11.4460422797433,-9.12349227711401));
#35094=CARTESIAN_POINT('Ctrl Pts',(41.0269029710712,12.4632402081524,-11.8775764776553));
#35095=CARTESIAN_POINT('Ctrl Pts',(42.5622713808008,13.0400785027576,-12.9726927515287));
#35096=CARTESIAN_POINT('Ctrl Pts',(45.9581475303923,14.3045284730937,-14.4683433355075));
#35097=CARTESIAN_POINT('Ctrl Pts',(47.7744493566106,14.9636108095524,-14.8498038985005));
#35098=CARTESIAN_POINT('Ctrl Pts',(49.6050326655027,15.6328286697383,-14.8500516281494));
#35099=CARTESIAN_POINT('Ctrl Pts',(36.6790985320904,9.39535856987503,1.59674363861559));
#35100=CARTESIAN_POINT('Ctrl Pts',(36.6453245302972,9.42749925373858,1.15301423608143));
#35101=CARTESIAN_POINT('Ctrl Pts',(36.5974326448246,9.46019603502289,0.635579107029969));
#35102=CARTESIAN_POINT('Ctrl Pts',(36.5487315518166,9.62291442707752,-1.86860431101451));
#35103=CARTESIAN_POINT('Ctrl Pts',(36.8674137538261,9.84228740317919,-3.70979114470517));
#35104=CARTESIAN_POINT('Ctrl Pts',(38.1668671434391,10.490259358486,-7.17014261469043));
#35105=CARTESIAN_POINT('Ctrl Pts',(39.1406457267337,10.9028003011106,-8.73670574472907));
#35106=CARTESIAN_POINT('Ctrl Pts',(41.5991163818614,11.8865765113095,-11.373454410536));
#35107=CARTESIAN_POINT('Ctrl Pts',(43.0690341146615,12.4447970771195,-12.4221714958514));
#35108=CARTESIAN_POINT('Ctrl Pts',(46.3159892044796,13.6646070765311,-13.8545909095343));
#35109=CARTESIAN_POINT('Ctrl Pts',(48.0562134772207,14.3020974767513,-14.2195188099531));
#35110=CARTESIAN_POINT('Ctrl Pts',(49.8063143340195,14.9473483165658,-14.2201291128083));
#35111=CARTESIAN_POINT('Ctrl Pts',(35.9142171164211,11.7862169042729,0.));
#35112=CARTESIAN_POINT('Ctrl Pts',(35.879143089373,11.9080080866873,-1.86858636178295));
#35113=CARTESIAN_POINT('Ctrl Pts',(36.1952232408275,12.126617143028,-3.71029995869426));
#35114=CARTESIAN_POINT('Ctrl Pts',(37.497580651705,12.7754415588947,-7.16936247494101));
#35115=CARTESIAN_POINT('Ctrl Pts',(38.4695778661786,13.1874595938719,-8.73699595767948));
#35116=CARTESIAN_POINT('Ctrl Pts',(39.8242114819224,13.7294890038866,-10.1890856763506));
#35117=CARTESIAN_POINT('Ctrl Pts',(39.9517643117909,13.7802180759794,-10.3203928635175));
#35118=CARTESIAN_POINT('Ctrl Pts',(40.081704941015,13.8316148870794,-10.4488603766));
#35119=CARTESIAN_POINT('Ctrl Pts',(36.5850719698906,9.50149509066483,1.60982338570648E-15));
#35120=CARTESIAN_POINT('Ctrl Pts',(36.5487315518166,9.62291442707752,-1.86860431101451));
#35121=CARTESIAN_POINT('Ctrl Pts',(36.8674137538261,9.84228740317919,-3.70979114470517));
#35122=CARTESIAN_POINT('Ctrl Pts',(38.1668671434391,10.490259358486,-7.17014261469043));
#35123=CARTESIAN_POINT('Ctrl Pts',(39.1406457267337,10.9028003011106,-8.73670574472907));
#35124=CARTESIAN_POINT('Ctrl Pts',(40.5018374092149,11.4474917709691,-10.196605355572));
#35125=CARTESIAN_POINT('Ctrl Pts',(40.6365673070934,11.5010595286606,-10.3350231942278));
#35126=CARTESIAN_POINT('Ctrl Pts',(40.773962973282,11.555373559002,-10.4702558450999));
#35127=CARTESIAN_POINT('Ctrl Pts',(41.7419576204998,15.7201209119706,1.2468908298854));
#35128=CARTESIAN_POINT('Ctrl Pts',(41.7052222707517,15.7550797324017,0.764254661706054));
#35129=CARTESIAN_POINT('Ctrl Pts',(41.6694633881772,15.7872856429817,0.332948671123798));
#35130=CARTESIAN_POINT('Ctrl Pts',(41.6254618648117,15.9462356620175,-0.978870002690552));
#35131=CARTESIAN_POINT('Ctrl Pts',(41.7773170936967,16.1248063760006,-1.98783577088475));
#35132=CARTESIAN_POINT('Ctrl Pts',(42.4353694479977,16.5748099612961,-3.80852727284034));
#35133=CARTESIAN_POINT('Ctrl Pts',(42.9396243659783,16.8558236637775,-4.65544360721786));
#35134=CARTESIAN_POINT('Ctrl Pts',(44.209570990269,17.4877814824514,-6.04997283343574));
#35135=CARTESIAN_POINT('Ctrl Pts',(44.9832291228105,17.8478990308906,-6.61832169896729));
#35136=CARTESIAN_POINT('Ctrl Pts',(46.6642543902182,18.5982747098438,-7.36768403084973));
#35137=CARTESIAN_POINT('Ctrl Pts',(47.5974477252292,19.0065156676782,-7.57138648690887));
#35138=CARTESIAN_POINT('Ctrl Pts',(48.4991757443116,19.3992863750339,-7.56962581969459));
#35139=CARTESIAN_POINT('Ctrl Pts',(40.1090570584213,14.0037398626873,1.35489321026543));
#35140=CARTESIAN_POINT('Ctrl Pts',(40.0732349602079,14.0378295966234,0.884255518285701));
#35141=CARTESIAN_POINT('Ctrl Pts',(40.0337447201316,14.0701900799517,0.426396949022936));
#35142=CARTESIAN_POINT('Ctrl Pts',(39.9884678119704,14.2303553472431,-1.25360819500655));
#35143=CARTESIAN_POINT('Ctrl Pts',(40.1915678319233,14.4214462185201,-2.51960912779463));
#35144=CARTESIAN_POINT('Ctrl Pts',(41.0479784866768,14.9326685312526,-4.84647586782628));
#35145=CARTESIAN_POINT('Ctrl Pts',(41.6970325717428,15.254242218588,-5.91572199045678));
#35146=CARTESIAN_POINT('Ctrl Pts',(43.3340488505895,15.9948572088803,-7.69376028693048));
#35147=CARTESIAN_POINT('Ctrl Pts',(44.322595033069,16.4161147204054,-8.41063186553294));
#35148=CARTESIAN_POINT('Ctrl Pts',(46.487283787483,17.31148223828,-9.37059840623356));
#35149=CARTESIAN_POINT('Ctrl Pts',(47.6695948287921,17.7905076322617,-9.6243537862995));
#35150=CARTESIAN_POINT('Ctrl Pts',(48.8333181822474,18.2612298390047,-9.62320046360562));
#35151=CARTESIAN_POINT('Ctrl Pts',(38.1728270004196,12.6395284821795,1.47293192394287));
#35152=CARTESIAN_POINT('Ctrl Pts',(38.1380009815219,12.6726703073971,1.01538091584187));
#35153=CARTESIAN_POINT('Ctrl Pts',(38.0944634070468,12.7052063084745,0.528580717869739));
#35154=CARTESIAN_POINT('Ctrl Pts',(38.0481727007018,12.8668122636064,-1.55402875457325));
#35155=CARTESIAN_POINT('Ctrl Pts',(38.3067247111946,13.0714224335833,-3.10121432123275));
#35156=CARTESIAN_POINT('Ctrl Pts',(39.3806906392157,13.6497783496954,-5.98129145451145));
#35157=CARTESIAN_POINT('Ctrl Pts',(40.187682027567,14.0155868029452,-7.2938940657431));
#35158=CARTESIAN_POINT('Ctrl Pts',(42.226231216963,14.8750601592607,-9.49113593806368));
#35159=CARTESIAN_POINT('Ctrl Pts',(43.4495197173632,15.3631044396819,-10.3708286016932));
#35160=CARTESIAN_POINT('Ctrl Pts',(46.1433554687415,16.4170971138854,-11.5604045561491));
#35161=CARTESIAN_POINT('Ctrl Pts',(47.5979046271564,16.9734434882805,-11.8694761541619));
#35162=CARTESIAN_POINT('Ctrl Pts',(49.0481649878424,17.529450194561,-11.8687142284813));
#35163=CARTESIAN_POINT('Ctrl Pts',(36.0076777827441,11.6799141290247,1.59647068126612));
#35164=CARTESIAN_POINT('Ctrl Pts',(35.9738923911208,11.7120656519291,1.152591636598));
#35165=CARTESIAN_POINT('Ctrl Pts',(35.9261470465084,11.7447913705166,0.635573001854836));
#35166=CARTESIAN_POINT('Ctrl Pts',(35.879143089373,11.9080080866873,-1.86858636178295));
#35167=CARTESIAN_POINT('Ctrl Pts',(36.1952232408275,12.126617143028,-3.71029995869426));
#35168=CARTESIAN_POINT('Ctrl Pts',(37.497580651705,12.7754415588947,-7.16936247494101));
#35169=CARTESIAN_POINT('Ctrl Pts',(38.4695778661786,13.1874595938719,-8.73699595767948));
#35170=CARTESIAN_POINT('Ctrl Pts',(40.9286921018555,14.1714247212918,-11.3730256982404));
#35171=CARTESIAN_POINT('Ctrl Pts',(42.3975559178032,14.7293359258803,-12.4235805192227));
#35172=CARTESIAN_POINT('Ctrl Pts',(45.6456867796022,15.9494910258928,-13.8529470821598));
#35173=CARTESIAN_POINT('Ctrl Pts',(47.3851293551851,16.5867336459606,-14.2204718557025));
#35174=CARTESIAN_POINT('Ctrl Pts',(49.1354594857183,17.2320701170938,-14.2198708430667));
#35175=CARTESIAN_POINT('Ctrl Pts',(36.6790985320904,9.39535856987503,1.59674363861559));
#35176=CARTESIAN_POINT('Ctrl Pts',(36.6453245302972,9.42749925373858,1.15301423608143));
#35177=CARTESIAN_POINT('Ctrl Pts',(36.5974326448246,9.46019603502288,0.635579107029969));
#35178=CARTESIAN_POINT('Ctrl Pts',(36.5487315518166,9.62291442707752,-1.86860431101452));
#35179=CARTESIAN_POINT('Ctrl Pts',(36.8674137538261,9.84228740317919,-3.70979114470517));
#35180=CARTESIAN_POINT('Ctrl Pts',(38.1668671434391,10.490259358486,-7.17014261469044));
#35181=CARTESIAN_POINT('Ctrl Pts',(39.1406457267289,10.9028003011094,-8.73670574472908));
#35182=CARTESIAN_POINT('Ctrl Pts',(41.5991163818662,11.8865765113107,-11.373454410536));
#35183=CARTESIAN_POINT('Ctrl Pts',(43.0690341146567,12.4447970771206,-12.4221714958514));
#35184=CARTESIAN_POINT('Ctrl Pts',(46.3159892044845,13.6646070765299,-13.8545909095343));
#35185=CARTESIAN_POINT('Ctrl Pts',(48.0562134772158,14.302097476756,-14.2195188099531));
#35186=CARTESIAN_POINT('Ctrl Pts',(49.8063143340195,14.9473483165658,-14.2201291128083));
#35187=CARTESIAN_POINT('Ctrl Pts',(39.019172373722,9.75977978596914,1.47327599461697));
#35188=CARTESIAN_POINT('Ctrl Pts',(38.9843607120455,9.79290794826382,1.01591361477532));
#35189=CARTESIAN_POINT('Ctrl Pts',(38.9406384185497,9.82540747302622,0.528588413620481));
#35190=CARTESIAN_POINT('Ctrl Pts',(38.8922084230886,9.98638527612265,-1.55405138010143));
#35191=CARTESIAN_POINT('Ctrl Pts',(39.1540403939528,10.191958389164,-3.10057294640731));
#35192=CARTESIAN_POINT('Ctrl Pts',(40.2243457187589,10.7692397539633,-5.98227484334544));
#35193=CARTESIAN_POINT('Ctrl Pts',(41.0335825742787,11.1357073475014,-7.29352824388559));
#35194=CARTESIAN_POINT('Ctrl Pts',(43.0713205117044,11.9949425681683,-9.49167634237202));
#35195=CARTESIAN_POINT('Ctrl Pts',(44.295937504919,12.483376807401,-10.3690524867825));
#35196=CARTESIAN_POINT('Ctrl Pts',(46.9882911615459,13.5369344722676,-11.5624766483317));
#35197=CARTESIAN_POINT('Ctrl Pts',(48.4438248432725,14.0935974137064,-11.8682745705354));
#35198=CARTESIAN_POINT('Ctrl Pts',(49.8937970264263,14.6494919462605,-11.8690397849986));
#35199=CARTESIAN_POINT('Ctrl Pts',(41.3856383979639,9.66008352082062,1.35541218776079));
#35200=CARTESIAN_POINT('Ctrl Pts',(41.3498379553998,9.6941526463457,0.885059012390845));
#35201=CARTESIAN_POINT('Ctrl Pts',(41.3100690951945,9.72645811078577,0.426408556874883));
#35202=CARTESIAN_POINT('Ctrl Pts',(41.2615653996783,9.88567590770113,-1.25364232212296));
#35203=CARTESIAN_POINT('Ctrl Pts',(41.4696127334802,10.0782192299378,-2.51864171288225));
#35204=CARTESIAN_POINT('Ctrl Pts',(42.3205019334091,10.5878207478988,-4.84795915807154));
#35205=CARTESIAN_POINT('Ctrl Pts',(42.9729429590446,10.9103886466027,-5.91517020465837));
#35206=CARTESIAN_POINT('Ctrl Pts',(44.6087355895318,11.6506444460343,-7.69457540340448));
#35207=CARTESIAN_POINT('Ctrl Pts',(45.5992855983381,12.072490150225,-8.40795287036824));
#35208=CARTESIAN_POINT('Ctrl Pts',(47.7617388416121,12.9672015236695,-9.3737238374209));
#35209=CARTESIAN_POINT('Ctrl Pts',(48.9455328277801,13.446713416983,-9.62254085998223));
#35210=CARTESIAN_POINT('Ctrl Pts',(50.1088235664895,13.9172574201602,-9.62369151535363));
#35211=CARTESIAN_POINT('Ctrl Pts',(43.6875520748214,9.10010115416761,1.24768178593779));
#35212=CARTESIAN_POINT('Ctrl Pts',(43.6508497297321,9.13502856601518,0.765479239901494));
#35213=CARTESIAN_POINT('Ctrl Pts',(43.6146662116266,9.16715062416918,0.332966362258436));
#35214=CARTESIAN_POINT('Ctrl Pts',(43.5657468507513,9.32465663564124,-0.978922014674724));
#35215=CARTESIAN_POINT('Ctrl Pts',(43.7251421133956,9.50544098102187,-1.98636136652885));
#35216=CARTESIAN_POINT('Ctrl Pts',(44.3747794050985,9.95297436780749,-3.8107879053477));
#35217=CARTESIAN_POINT('Ctrl Pts',(44.8841962446775,10.2355033142224,-4.65460264913776));
#35218=CARTESIAN_POINT('Ctrl Pts',(46.1522779478775,10.8669137022454,-6.05121512489442));
#35219=CARTESIAN_POINT('Ctrl Pts',(46.928990044369,11.227927695242,-6.61423873303054));
#35220=CARTESIAN_POINT('Ctrl Pts',(48.6066082448372,11.9773033666524,-7.37244739483315));
#35221=CARTESIAN_POINT('Ctrl Pts',(49.5420562727261,12.3863053996828,-7.56862230169514));
#35222=CARTESIAN_POINT('Ctrl Pts',(50.4431303715411,12.7787848949965,-7.57037421505972));
#35223=CARTESIAN_POINT('Ctrl Pts',(37.3033966274915,6.43660260973346,1.59647061166179));
#35224=CARTESIAN_POINT('Ctrl Pts',(37.2745307626595,6.47323503721765,1.15259158904714));
#35225=CARTESIAN_POINT('Ctrl Pts',(37.2319287549545,6.51242252436852,0.635572970245465));
#35226=CARTESIAN_POINT('Ctrl Pts',(37.2086313911938,6.68066728815551,-1.86858636171891));
#35227=CARTESIAN_POINT('Ctrl Pts',(37.5526056149563,6.85206832386134,-3.7102999587003));
#35228=CARTESIAN_POINT('Ctrl Pts',(38.934044247035,7.30894385840886,-7.16936247493491));
#35229=CARTESIAN_POINT('Ctrl Pts',(39.9547842114115,7.57843851744906,-8.73699595770386));
#35230=CARTESIAN_POINT('Ctrl Pts',(42.5289010478496,8.20241985396081,-11.3730256982159));
#35231=CARTESIAN_POINT('Ctrl Pts',(44.0622129909515,8.5456112103854,-12.4235805192521));
#35232=CARTESIAN_POINT('Ctrl Pts',(47.4509287397227,9.29108967269768,-13.8529470821302));
#35233=CARTESIAN_POINT('Ctrl Pts',(49.263355378306,9.67429759302916,-14.2204718556739));
#35234=CARTESIAN_POINT('Ctrl Pts',(51.0877106274638,10.0639675197017,-14.2198708430667));
#35235=CARTESIAN_POINT('Ctrl Pts',(36.7825298650421,5.63986099173568,1.62964605326941));
#35236=CARTESIAN_POINT('Ctrl Pts',(36.7539048206817,5.67618780432166,1.1894701989102));
#35237=CARTESIAN_POINT('Ctrl Pts',(36.7101544788329,5.71558400588172,0.664243924999381));
#35238=CARTESIAN_POINT('Ctrl Pts',(36.68626524241,5.88421645976228,-1.95287905121125));
#35239=CARTESIAN_POINT('Ctrl Pts',(37.0467430607544,6.05723890417281,-3.87337387078733));
#35240=CARTESIAN_POINT('Ctrl Pts',(38.490650983132,6.52398110941273,-7.48792130213842));
#35241=CARTESIAN_POINT('Ctrl Pts',(39.5574047047037,6.79950954685247,-9.12360836231238));
#35242=CARTESIAN_POINT('Ctrl Pts',(42.2476392596819,7.44044656126999,-11.8774049927189));
#35243=CARTESIAN_POINT('Ctrl Pts',(43.8490375949839,7.79284527694883,-12.9732563608924));
#35244=CARTESIAN_POINT('Ctrl Pts',(47.3907837817412,8.56121110823887,-14.4676858045425));
#35245=CARTESIAN_POINT('Ctrl Pts',(49.2820718587551,8.95504492393606,-14.8501851005532));
#35246=CARTESIAN_POINT('Ctrl Pts',(51.1893577615276,9.35695250368056,-14.8499483202528));
#35247=CARTESIAN_POINT('Ctrl Pts',(36.9183140647621,4.69711890654721,1.62975523620918));
#35248=CARTESIAN_POINT('Ctrl Pts',(36.8896929129492,4.7334407792703,1.18963923869573));
#35249=CARTESIAN_POINT('Ctrl Pts',(36.845882904082,4.77283386569958,0.664246367069779));
#35250=CARTESIAN_POINT('Ctrl Pts',(36.8212933555167,4.9413656298699,-1.95288623090525));
#35251=CARTESIAN_POINT('Ctrl Pts',(37.1828448868692,5.11454240778225,-3.87317034519028));
#35252=CARTESIAN_POINT('Ctrl Pts',(38.6255544971408,5.58111241365379,-7.48823335803965));
#35253=CARTESIAN_POINT('Ctrl Pts',(39.6930432805366,5.85674647908816,-9.12349227712411));
#35254=CARTESIAN_POINT('Ctrl Pts',(42.3830122692892,6.49764533220215,-11.8775764776452));
#35255=CARTESIAN_POINT('Ctrl Pts',(43.9848454910782,6.8501065376293,-12.9726927515247));
#35256=CARTESIAN_POINT('Ctrl Pts',(47.5261065109178,7.61840266564566,-14.4683433355115));
#35257=CARTESIAN_POINT('Ctrl Pts',(49.4177181995078,8.01228979376185,-14.8498038985861));
#35258=CARTESIAN_POINT('Ctrl Pts',(51.3249084414063,8.41417681322607,-14.8500516281495));
#35259=CARTESIAN_POINT('Ctrl Pts',(37.6428571267913,4.07974739676227,1.59674356901122));
#35260=CARTESIAN_POINT('Ctrl Pts',(37.6140009933336,4.11636747459116,1.15301418851043));
#35261=CARTESIAN_POINT('Ctrl Pts',(37.5712498180838,4.15554717391331,0.635579075421461));
#35262=CARTESIAN_POINT('Ctrl Pts',(37.5462016739414,4.32354021342426,-1.86860431095391));
#35263=CARTESIAN_POINT('Ctrl Pts',(37.8928601802626,4.49532708288615,-3.70979114470765));
#35264=CARTESIAN_POINT('Ctrl Pts',(39.2713030320377,4.95177211901035,-7.17014261468797));
#35265=CARTESIAN_POINT('Ctrl Pts',(40.2938806509913,5.2215308480374,-8.736705744732));
#35266=CARTESIAN_POINT('Ctrl Pts',(42.8673335718703,5.84541678129212,-11.3734544105331));
#35267=CARTESIAN_POINT('Ctrl Pts',(44.4017327311872,6.18876436208449,-12.4221714958281));
#35268=CARTESIAN_POINT('Ctrl Pts',(47.7892355626643,6.9340685662168,-13.8545909095575));
#35269=CARTESIAN_POINT('Ctrl Pts',(49.6024712046817,7.31741049756506,-14.2195188100863));
#35270=CARTESIAN_POINT('Ctrl Pts',(51.4265873271606,7.70702829356553,-14.2201291128083));
#35271=CARTESIAN_POINT('Ctrl Pts',(37.2260157227863,6.55512420987368,0.));
#35272=CARTESIAN_POINT('Ctrl Pts',(37.2086313911938,6.68066728815551,-1.86858636171891));
#35273=CARTESIAN_POINT('Ctrl Pts',(37.5526056149563,6.85206832386134,-3.7102999587003));
#35274=CARTESIAN_POINT('Ctrl Pts',(38.934044247035,7.30894385840886,-7.16936247493491));
#35275=CARTESIAN_POINT('Ctrl Pts',(39.9547842114115,7.57843851744906,-8.73699595770386));
#35276=CARTESIAN_POINT('Ctrl Pts',(41.3727684379698,7.92216638570883,-10.1890856763496));
#35277=CARTESIAN_POINT('Ctrl Pts',(41.5062424636367,7.95422644864134,-10.3203928635163));
#35278=CARTESIAN_POINT('Ctrl Pts',(41.6421750134739,7.98660763468041,-10.4488603765993));
#35279=CARTESIAN_POINT('Ctrl Pts',(37.5648924257372,4.19818497005497,3.88578058618805E-16));
#35280=CARTESIAN_POINT('Ctrl Pts',(37.5462016739414,4.32354021342426,-1.86860431095391));
#35281=CARTESIAN_POINT('Ctrl Pts',(37.8928601802626,4.49532708288615,-3.70979114470765));
#35282=CARTESIAN_POINT('Ctrl Pts',(39.2713030320377,4.95177211901035,-7.17014261468797));
#35283=CARTESIAN_POINT('Ctrl Pts',(40.2938806509913,5.2215308480374,-8.736705744732));
#35284=CARTESIAN_POINT('Ctrl Pts',(41.7187350432347,5.56696037000169,-10.1966053555729));
#35285=CARTESIAN_POINT('Ctrl Pts',(41.8597170717888,5.60080882153324,-10.3350231942292));
#35286=CARTESIAN_POINT('Ctrl Pts',(42.0034439406476,5.63501657134798,-10.4702558451016));
#35287=CARTESIAN_POINT('Ctrl Pts',(43.5542911395533,9.61961280540173,1.24689076028089));
#35288=CARTESIAN_POINT('Ctrl Pts',(43.52290486313,9.65944377882137,0.764254616120504));
#35289=CARTESIAN_POINT('Ctrl Pts',(43.4920933360762,9.69641089756346,0.332948654586433));
#35290=CARTESIAN_POINT('Ctrl Pts',(43.4711606313105,9.86000510220811,-0.97887000271989));
#35291=CARTESIAN_POINT('Ctrl Pts',(43.6468834551771,10.0151469714622,-1.98783577087993));
#35292=CARTESIAN_POINT('Ctrl Pts',(44.3622799728308,10.3669195547339,-3.80852727284503));
#35293=CARTESIAN_POINT('Ctrl Pts',(44.901394722402,10.5733099858341,-4.65544360723717));
#35294=CARTESIAN_POINT('Ctrl Pts',(46.2483520959891,11.0181031366242,-6.04997283341623));
#35295=CARTESIAN_POINT('Ctrl Pts',(47.0653855748544,11.2644521757558,-6.61832169905383));
#35296=CARTESIAN_POINT('Ctrl Pts',(48.8360900223635,11.7679552730305,-7.36768403076287));
#35297=CARTESIAN_POINT('Ctrl Pts',(49.8178835406694,12.0392336678406,-7.57138648671366));
#35298=CARTESIAN_POINT('Ctrl Pts',(50.7663303683513,12.2996772587577,-7.56962581969442));
#35299=CARTESIAN_POINT('Ctrl Pts',(41.6937446593044,8.15308801979167,1.35489314066098));
#35300=CARTESIAN_POINT('Ctrl Pts',(41.6631386548959,8.19192878357257,0.884255472089525));
#35301=CARTESIAN_POINT('Ctrl Pts',(41.6286557481959,8.22957992923818,0.426396927831693));
#35302=CARTESIAN_POINT('Ctrl Pts',(41.6066335880765,8.3945585188291,-1.25360819500777));
#35303=CARTESIAN_POINT('Ctrl Pts',(41.834861409093,8.55480021407296,-2.51960912779223));
#35304=CARTESIAN_POINT('Ctrl Pts',(42.7553095590059,8.93893907695881,-4.84647586782858));
#35305=CARTESIAN_POINT('Ctrl Pts',(43.4435219166219,9.1648695806861,-5.9157219904738));
#35306=CARTESIAN_POINT('Ctrl Pts',(45.169276232732,9.66497447126936,-7.69376028691332));
#35307=CARTESIAN_POINT('Ctrl Pts',(46.2077116350196,9.94125939867244,-8.41063186558128));
#35308=CARTESIAN_POINT('Ctrl Pts',(48.4777910626938,10.5194460361889,-9.37059840618501));
#35309=CARTESIAN_POINT('Ctrl Pts',(49.7162403038048,10.8253352376576,-9.62435378619477));
#35310=CARTESIAN_POINT('Ctrl Pts',(50.9351093861917,11.1256510703083,-9.62320046360551));
#35311=CARTESIAN_POINT('Ctrl Pts',(39.5830751094924,7.07831661167166,1.47293185433847));
#35312=CARTESIAN_POINT('Ctrl Pts',(39.5533201442405,7.11607735826543,1.01538086898131));
#35313=CARTESIAN_POINT('Ctrl Pts',(39.5148560779746,7.15447823086686,0.528580691589297));
#35314=CARTESIAN_POINT('Ctrl Pts',(39.4920354699322,7.3210271226842,-1.55402875454293));
#35315=CARTESIAN_POINT('Ctrl Pts',(39.7770748570079,7.486758868588,-3.10121432123517));
#35316=CARTESIAN_POINT('Ctrl Pts',(40.9224179890784,7.90638666804373,-5.98129145450895));
#35317=CARTESIAN_POINT('Ctrl Pts',(41.7732553395417,8.15362486975184,-7.29389406576261));
#35318=CARTESIAN_POINT('Ctrl Pts',(43.9133708492461,8.71423422838807,-9.49113593804405));
#35319=CARTESIAN_POINT('Ctrl Pts',(45.1936639793709,9.02321881659059,-10.3708286017369));
#35320=CARTESIAN_POINT('Ctrl Pts',(48.010079163986,9.68311056587906,-11.5604045561052));
#35321=CARTESIAN_POINT('Ctrl Pts',(49.5289994535062,10.0267902081681,-11.8694761541095));
#35322=CARTESIAN_POINT('Ctrl Pts',(51.0436262593386,10.3707439991142,-11.8687142284812));
#35323=CARTESIAN_POINT('Ctrl Pts',(37.3033966274915,6.43660260973346,1.59647061166179));
#35324=CARTESIAN_POINT('Ctrl Pts',(37.2745307626595,6.47323503721765,1.15259158904714));
#35325=CARTESIAN_POINT('Ctrl Pts',(37.2319287549545,6.51242252436852,0.635572970245465));
#35326=CARTESIAN_POINT('Ctrl Pts',(37.2086313911938,6.68066728815551,-1.86858636171891));
#35327=CARTESIAN_POINT('Ctrl Pts',(37.5526056149563,6.85206832386134,-3.7102999587003));
#35328=CARTESIAN_POINT('Ctrl Pts',(38.934044247035,7.30894385840886,-7.16936247493491));
#35329=CARTESIAN_POINT('Ctrl Pts',(39.9547842114115,7.57843851744906,-8.73699595770386));
#35330=CARTESIAN_POINT('Ctrl Pts',(42.5289010478496,8.20241985396081,-11.3730256982159));
#35331=CARTESIAN_POINT('Ctrl Pts',(44.0622129909515,8.5456112103854,-12.4235805192521));
#35332=CARTESIAN_POINT('Ctrl Pts',(47.4509287397227,9.29108967269768,-13.8529470821302));
#35333=CARTESIAN_POINT('Ctrl Pts',(49.263355378306,9.67429759302916,-14.2204718556739));
#35334=CARTESIAN_POINT('Ctrl Pts',(51.0877106274638,10.0639675197017,-14.2198708430667));
#35335=CARTESIAN_POINT('Ctrl Pts',(37.6428571267913,4.07974739676227,1.59674356901122));
#35336=CARTESIAN_POINT('Ctrl Pts',(37.6140009933336,4.11636747459113,1.15301418851043));
#35337=CARTESIAN_POINT('Ctrl Pts',(37.5712498180838,4.15554717391332,0.635579075421461));
#35338=CARTESIAN_POINT('Ctrl Pts',(37.5462016739414,4.32354021342426,-1.86860431095391));
#35339=CARTESIAN_POINT('Ctrl Pts',(37.8928601802626,4.49532708288675,-3.70979114470885));
#35340=CARTESIAN_POINT('Ctrl Pts',(39.2713030320377,4.95177211900975,-7.17014261468677));
#35341=CARTESIAN_POINT('Ctrl Pts',(40.2938806509865,5.221530848038,-8.736705744732));
#35342=CARTESIAN_POINT('Ctrl Pts',(42.867333571875,5.84541678129152,-11.3734544105331));
#35343=CARTESIAN_POINT('Ctrl Pts',(44.4017327311872,6.18876436208449,-12.4221714958282));
#35344=CARTESIAN_POINT('Ctrl Pts',(47.7892355626643,6.9340685662168,-13.8545909095575));
#35345=CARTESIAN_POINT('Ctrl Pts',(49.6024712046821,7.31741049756335,-14.2195188100863));
#35346=CARTESIAN_POINT('Ctrl Pts',(51.4265873271606,7.70702829356553,-14.2201291128083));
#35347=CARTESIAN_POINT('Ctrl Pts',(40.0109749372547,4.10743210000906,1.47327592501251));
#35348=CARTESIAN_POINT('Ctrl Pts',(39.9812322386681,4.14517727950216,1.01591356789114));
#35349=CARTESIAN_POINT('Ctrl Pts',(39.9425801423883,4.18356833531983,0.528588387341121));
#35350=CARTESIAN_POINT('Ctrl Pts',(39.9175526247866,4.34979992137089,-1.55405138007544));
#35351=CARTESIAN_POINT('Ctrl Pts',(40.2059756280488,4.51601802193941,-3.1005729464062));
#35352=CARTESIAN_POINT('Ctrl Pts',(41.3475424919703,4.93510316561798,-5.9822748433466));
#35353=CARTESIAN_POINT('Ctrl Pts',(42.2006962594468,5.18267423522182,-7.29352824387409));
#35354=CARTESIAN_POINT('Ctrl Pts',(44.3399748842815,5.74316333527757,-9.49167634238358));
#35355=CARTESIAN_POINT('Ctrl Pts',(45.6216384820559,6.05234484883939,-10.3690524867496));
#35356=CARTESIAN_POINT('Ctrl Pts',(48.4365247491596,6.71201694062345,-11.5624766483647));
#35357=CARTESIAN_POINT('Ctrl Pts',(49.9564645932056,7.05586981550164,-11.8682745706924));
#35358=CARTESIAN_POINT('Ctrl Pts',(51.4707901907297,7.39975358641479,-11.8690397849987));
#35359=CARTESIAN_POINT('Ctrl Pts',(42.3391654916811,3.67196736957026,1.35541211815624));
#35360=CARTESIAN_POINT('Ctrl Pts',(42.3085779896465,3.71078465278407,0.885058966158364));
#35361=CARTESIAN_POINT('Ctrl Pts',(42.2738114686987,3.7484209913462,0.426408535685267));
#35362=CARTESIAN_POINT('Ctrl Pts',(42.2484605261895,3.91292097417181,-1.2536423221307));
#35363=CARTESIAN_POINT('Ctrl Pts',(42.4817920098845,4.07389626034862,-2.51864171287515));
#35364=CARTESIAN_POINT('Ctrl Pts',(43.3965442422595,4.45721661076415,-4.84795915807873));
#35365=CARTESIAN_POINT('Ctrl Pts',(44.0882505573344,4.68364919432671,-5.91517020463247));
#35366=CARTESIAN_POINT('Ctrl Pts',(45.8127425618267,5.18357269340712,-7.69457540343052));
#35367=CARTESIAN_POINT('Ctrl Pts',(46.8532451029934,5.46015465231276,-8.40795287032088));
#35368=CARTESIAN_POINT('Ctrl Pts',(49.1210183946222,6.03800997039568,-9.37372383746844));
#35369=CARTESIAN_POINT('Ctrl Pts',(50.3610047225093,6.3441696742926,-9.6225408601964));
#35370=CARTESIAN_POINT('Ctrl Pts',(51.5794202324977,6.64437068472149,-9.62369151535374));
#35371=CARTESIAN_POINT('Ctrl Pts',(44.5379552064474,2.79008834334071,1.24768171633314));
#35372=CARTESIAN_POINT('Ctrl Pts',(44.5065971288807,2.82988353082186,0.765479194261193));
#35373=CARTESIAN_POINT('Ctrl Pts',(44.4753533549286,2.86682808255862,0.332966345723582));
#35374=CARTESIAN_POINT('Ctrl Pts',(44.4493473654757,3.02969285881443,-0.978922014714018));
#35375=CARTESIAN_POINT('Ctrl Pts',(44.6328485090626,3.18595276920499,-1.98636136651458));
#35376=CARTESIAN_POINT('Ctrl Pts',(45.3395640713933,3.53647788529764,-3.81078790536211));
#35377=CARTESIAN_POINT('Ctrl Pts',(45.8840038433944,3.74363351929919,-4.65460264909031));
#35378=CARTESIAN_POINT('Ctrl Pts',(47.2290373705107,4.18815021742991,-6.05121512494211));
#35379=CARTESIAN_POINT('Ctrl Pts',(48.0492213058428,4.43495195223039,-6.61423873295915));
#35380=CARTESIAN_POINT('Ctrl Pts',(49.8164110494045,4.9379500967639,-7.37244739490483));
#35381=CARTESIAN_POINT('Ctrl Pts',(50.8005446234618,5.20966094390348,-7.56862230199509));
#35382=CARTESIAN_POINT('Ctrl Pts',(51.7483027430072,5.46990934942745,-7.57037421505989));
#35383=CARTESIAN_POINT('Ctrl Pts',(37.8397258902528,1.0622604283696,1.59647049649025));
#35384=CARTESIAN_POINT('Ctrl Pts',(37.8339627771316,1.07222001191037,1.48695569078595));
#35385=CARTESIAN_POINT('Ctrl Pts',(37.8282008616259,1.08217829864126,1.37746392936641));
#35386=CARTESIAN_POINT('Ctrl Pts',(37.803637843476,1.12462383849689,0.910698635110369));
#35387=CARTESIAN_POINT('Ctrl Pts',(37.7798283754123,1.15759409919791,0.486448413031079));
#35388=CARTESIAN_POINT('Ctrl Pts',(37.7806592587321,1.31732736909012,-1.86858636174431));
#35389=CARTESIAN_POINT('Ctrl Pts',(38.1455252315258,1.43803115335118,-3.71029995870316));
#35390=CARTESIAN_POINT('Ctrl Pts',(39.5779229780183,1.69365713822224,-7.16936247493209));
#35391=CARTESIAN_POINT('Ctrl Pts',(40.6266263701611,1.81514228728193,-8.73699595769941));
#35392=CARTESIAN_POINT('Ctrl Pts',(43.2633442117545,2.06643737216945,-11.3730256982204));
#35393=CARTESIAN_POINT('Ctrl Pts',(44.8298904725261,2.18792249429946,-12.4235805192368));
#35394=CARTESIAN_POINT('Ctrl Pts',(48.290206627889,2.44354852691157,-13.8529470821456));
#35395=CARTESIAN_POINT('Ctrl Pts',(50.138721549822,2.56492073913256,-14.2204718556691));
#35396=CARTESIAN_POINT('Ctrl Pts',(51.9999633056261,2.69099156569408,-14.2198708430667));
#35397=CARTESIAN_POINT('Ctrl Pts',(37.2107726459064,0.347755560296454,1.62964593809789));
#35398=CARTESIAN_POINT('Ctrl Pts',(37.2050094709227,0.35771525074062,1.52012995689155));
#35399=CARTESIAN_POINT('Ctrl Pts',(37.1992477086583,0.367673423350967,1.4106409479282));
#35400=CARTESIAN_POINT('Ctrl Pts',(37.1746843010492,0.410118993966263,0.943868932648104));
#35401=CARTESIAN_POINT('Ctrl Pts',(37.1499314621533,0.443150337937791,0.508392298460196));
#35402=CARTESIAN_POINT('Ctrl Pts',(37.1502632733139,0.603323715727814,-1.95287905124252));
#35403=CARTESIAN_POINT('Ctrl Pts',(37.5316956084151,0.723283698694339,-3.87337387079016));
#35404=CARTESIAN_POINT('Ctrl Pts',(39.0273309715468,0.979785618832962,-7.48792130213564));
#35405=CARTESIAN_POINT('Ctrl Pts',(40.1224384633774,1.10069469071835,-9.12360836230794));
#35406=CARTESIAN_POINT('Ctrl Pts',(42.87650515713,1.35224759481403,-11.8774049927233));
#35407=CARTESIAN_POINT('Ctrl Pts',(44.51175513264,1.47315665467739,-12.9732563608865));
#35408=CARTESIAN_POINT('Ctrl Pts',(48.1268013089989,1.72965859379905,-14.4676858045483));
#35409=CARTESIAN_POINT('Ctrl Pts',(50.0548871962082,1.850325392223,-14.8501851005389));
#35410=CARTESIAN_POINT('Ctrl Pts',(51.9999570907663,1.97670704765929,-14.8499483202528));
#35411=CARTESIAN_POINT('Ctrl Pts',(37.2110085708707,-0.604714876209846,
1.62975512103766));
#35412=CARTESIAN_POINT('Ctrl Pts',(37.2052453954626,-0.594755185033613,
1.52023913178141));
#35413=CARTESIAN_POINT('Ctrl Pts',(37.1994836453944,-0.584797013151259,
1.41075014108546));
#35414=CARTESIAN_POINT('Ctrl Pts',(37.174920187614,-0.542351442553382,0.943978082258184));
#35415=CARTESIAN_POINT('Ctrl Pts',(37.1500689010425,-0.509320134040885,
0.508394167547144));
#35416=CARTESIAN_POINT('Ctrl Pts',(37.1497353315483,-0.349146756273058,
-1.95288623093576));
#35417=CARTESIAN_POINT('Ctrl Pts',(37.5322524147587,-0.229186815991632,
-3.8731703451907));
#35418=CARTESIAN_POINT('Ctrl Pts',(39.0266771563473,0.0273151951141526,
-7.48823335803926));
#35419=CARTESIAN_POINT('Ctrl Pts',(40.1225272605589,0.148224209648788,-9.12349227712685));
#35420=CARTESIAN_POINT('Ctrl Pts',(42.8763256602578,0.399777134881894,-11.8775764776425));
#35421=CARTESIAN_POINT('Ctrl Pts',(44.5120149889433,0.520686157637575,-12.9726927515332));
#35422=CARTESIAN_POINT('Ctrl Pts',(48.1265710168889,0.777188149417136,-14.468343335503));
#35423=CARTESIAN_POINT('Ctrl Pts',(50.0549848089105,0.897861662882116,-14.8498038985576));
#35424=CARTESIAN_POINT('Ctrl Pts',(51.9999570902568,1.02423658127858,-14.8500516281495));
#35425=CARTESIAN_POINT('Ctrl Pts',(37.8403157026637,-1.31891566289614,1.59674345383971));
#35426=CARTESIAN_POINT('Ctrl Pts',(37.8345525884796,-1.30895607752527,1.48722862801069));
#35427=CARTESIAN_POINT('Ctrl Pts',(37.828790703466,-1.29899779261428,1.37773691225954));
#35428=CARTESIAN_POINT('Ctrl Pts',(37.8042275598881,-1.25655225280221,0.910971509135609));
#35429=CARTESIAN_POINT('Ctrl Pts',(37.7801719726404,-1.22358208074877,0.486453085748451));
#35430=CARTESIAN_POINT('Ctrl Pts',(37.779339404299,-1.06384881091203,-1.8686043109774));
#35431=CARTESIAN_POINT('Ctrl Pts',(38.1469172474041,-0.943145133364113,
-3.7097911447081));
#35432=CARTESIAN_POINT('Ctrl Pts',(39.5762884400003,-0.687518921074427,
-7.17014261468754));
#35433=CARTESIAN_POINT('Ctrl Pts',(40.6268483631124,-0.566033915391893,
-8.7367057447395));
#35434=CARTESIAN_POINT('Ctrl Pts',(43.2628954695764,-0.31473877766099,-11.3734544105255));
#35435=CARTESIAN_POINT('Ctrl Pts',(44.8305401132913,-0.193253748299652,
-12.4221714958415));
#35436=CARTESIAN_POINT('Ctrl Pts',(48.2896308976067,0.0623724159563386,
-13.8545909095442));
#35437=CARTESIAN_POINT('Ctrl Pts',(50.1389656602224,0.183762141962158,-14.2195188100102));
#35438=CARTESIAN_POINT('Ctrl Pts',(51.9999633043522,0.309815399742307,-14.2201291128083));
#35439=CARTESIAN_POINT('Ctrl Pts',(37.78,1.19058808997869,0.));
#35440=CARTESIAN_POINT('Ctrl Pts',(37.7806592587321,1.31732736909012,-1.86858636174431));
#35441=CARTESIAN_POINT('Ctrl Pts',(38.1455252315258,1.43803115335118,-3.71029995870316));
#35442=CARTESIAN_POINT('Ctrl Pts',(39.5779229780183,1.69365713822224,-7.16936247493209));
#35443=CARTESIAN_POINT('Ctrl Pts',(40.6266263701611,1.81514228728193,-8.73699595769941));
#35444=CARTESIAN_POINT('Ctrl Pts',(42.079095137833,1.95357130555262,-10.1890856763502));
#35445=CARTESIAN_POINT('Ctrl Pts',(42.2157732130433,1.96630970889328,-10.3203928635173));
#35446=CARTESIAN_POINT('Ctrl Pts',(42.3549304887758,1.97901608230145,-10.4488603766003));
#35447=CARTESIAN_POINT('Ctrl Pts',(37.7799999998341,-1.19058808946242,-4.87766813886054E-9));
#35448=CARTESIAN_POINT('Ctrl Pts',(37.7793394048005,-1.0638488105451,-1.86860431420344));
#35449=CARTESIAN_POINT('Ctrl Pts',(38.1469172479177,-0.943145133125576,
-3.70979114624586));
#35450=CARTESIAN_POINT('Ctrl Pts',(38.8616028436213,-0.815332027121487,
-5.43996687972834));
#35451=CARTESIAN_POINT('Ctrl Pts',(39.5762884399489,-0.687518921005817,
-7.17014261472125));
#35452=CARTESIAN_POINT('Ctrl Pts',(40.6268483630872,-0.566033915352764,
-8.73670574476311));
#35453=CARTESIAN_POINT('Ctrl Pts',(41.9448719163384,-0.440386346516728,
-10.0550800776386));
#35454=CARTESIAN_POINT('Ctrl Pts',(42.0863595386707,-0.426898290311208,
-10.1966053555765));
#35455=CARTESIAN_POINT('Ctrl Pts',(42.2307237103618,-0.41345820180873,-10.3350231942305));
#35456=CARTESIAN_POINT('Ctrl Pts',(42.3778559173178,-0.400053103664619,
-10.470255845101));
#35457=CARTESIAN_POINT('Ctrl Pts',(44.4799848904464,3.32327712821972,1.24689064510934));
#35458=CARTESIAN_POINT('Ctrl Pts',(44.4742224279398,3.33323558739414,1.13738820285035));
#35459=CARTESIAN_POINT('Ctrl Pts',(44.4684589625378,3.34319507469509,1.02786748900887));
#35460=CARTESIAN_POINT('Ctrl Pts',(44.4438997771526,3.38564028976811,0.56117289744884));
#35461=CARTESIAN_POINT('Ctrl Pts',(44.4295022685185,3.41796558601113,0.254828874445209));
#35462=CARTESIAN_POINT('Ctrl Pts',(44.4319119278293,3.5730532724159,-0.978870002679086));
#35463=CARTESIAN_POINT('Ctrl Pts',(44.6279251367323,3.70160805589233,-1.98783577088195));
#35464=CARTESIAN_POINT('Ctrl Pts',(45.386102407664,3.94798856175628,-3.80852727284305));
#35465=CARTESIAN_POINT('Ctrl Pts',(45.9491021672716,4.07555420745019,-4.65544360723259));
#35466=CARTESIAN_POINT('Ctrl Pts',(47.3456501222045,4.32412798455813,-6.04997283342086));
#35467=CARTESIAN_POINT('Ctrl Pts',(48.1894265020301,4.45169355820927,-6.61832169901019));
#35468=CARTESIAN_POINT('Ctrl Pts',(50.0137636932357,4.69807420295008,-7.36768403080661));
#35469=CARTESIAN_POINT('Ctrl Pts',(51.0241709100486,4.82686758914895,-7.57138648680884));
#35470=CARTESIAN_POINT('Ctrl Pts',(52.000028904099,4.9496821828336,-7.56962581969449));
#35471=CARTESIAN_POINT('Ctrl Pts',(42.429667852992,2.13646282180974,1.35489302548942));
#35472=CARTESIAN_POINT('Ctrl Pts',(42.4239051893647,2.14642162855157,1.24538676140638));
#35473=CARTESIAN_POINT('Ctrl Pts',(42.4181422088106,2.15638074475633,1.13587499712206));
#35474=CARTESIAN_POINT('Ctrl Pts',(42.393581814172,2.19882606010976,0.669158551015892));
#35475=CARTESIAN_POINT('Ctrl Pts',(42.3762274914793,2.23135049600752,0.326351368873808));
#35476=CARTESIAN_POINT('Ctrl Pts',(42.3778082879602,2.38787268687572,-1.25360819498701));
#35477=CARTESIAN_POINT('Ctrl Pts',(42.6265178497614,2.51400314727895,-2.51960912779653));
#35478=CARTESIAN_POINT('Ctrl Pts',(43.592265824835,2.76323860082472,-4.84647586782431));
#35479=CARTESIAN_POINT('Ctrl Pts',(44.3056264360906,2.88892662741303,-5.91572199047166));
#35480=CARTESIAN_POINT('Ctrl Pts',(46.0849874081721,3.13834072491811,-7.69376028691551));
#35481=CARTESIAN_POINT('Ctrl Pts',(47.1521724801633,3.26402870377935,-8.41063186555665));
#35482=CARTESIAN_POINT('Ctrl Pts',(49.481430310228,3.51326424840639,-9.3705984062097));
#35483=CARTESIAN_POINT('Ctrl Pts',(50.7508064960181,3.63979023543883,-9.62435378624233));
#35484=CARTESIAN_POINT('Ctrl Pts',(52.0000086477592,3.76358612954873,-9.62320046360555));
#35485=CARTESIAN_POINT('Ctrl Pts',(40.1875259567355,1.37301063256203,1.47293173916693));
#35486=CARTESIAN_POINT('Ctrl Pts',(40.1817630734217,1.38296981895596,1.36342130045779));
#35487=CARTESIAN_POINT('Ctrl Pts',(40.1760006162045,1.39292852977775,1.25391931221354));
#35488=CARTESIAN_POINT('Ctrl Pts',(40.1514389273988,1.43537395479689,0.78717899271973));
#35489=CARTESIAN_POINT('Ctrl Pts',(40.1309065737656,1.46811616862065,0.404559744697675));
#35490=CARTESIAN_POINT('Ctrl Pts',(40.1319542826336,1.6262069816417,-1.55402875454452));
#35491=CARTESIAN_POINT('Ctrl Pts',(40.4376784663362,1.7496864830589,-3.10121432123695));
#35492=CARTESIAN_POINT('Ctrl Pts',(41.6310829191998,2.00204375396605,-5.98129145450721));
#35493=CARTESIAN_POINT('Ctrl Pts',(42.5084456369411,2.12567864734774,-7.29389406576051));
#35494=CARTESIAN_POINT('Ctrl Pts',(44.7065608867256,2.37601161837676,-9.49113593804618));
#35495=CARTESIAN_POINT('Ctrl Pts',(46.0177955705402,2.49964647926445,-10.3708286017169));
#35496=CARTESIAN_POINT('Ctrl Pts',(48.8994560970704,2.75200381047966,-11.5604045561253));
#35497=CARTESIAN_POINT('Ctrl Pts',(50.4518266808763,2.87602039418504,-11.8694761541333));
#35498=CARTESIAN_POINT('Ctrl Pts',(51.9999864978575,3.00091936260147,-11.8687142284813));
#35499=CARTESIAN_POINT('Ctrl Pts',(37.8397258902528,1.0622604283696,1.59647049649025));
#35500=CARTESIAN_POINT('Ctrl Pts',(37.8339627771316,1.07222001191037,1.48695569078595));
#35501=CARTESIAN_POINT('Ctrl Pts',(37.8282008616259,1.08217829864126,1.37746392936641));
#35502=CARTESIAN_POINT('Ctrl Pts',(37.803637843476,1.12462383849689,0.910698635110369));
#35503=CARTESIAN_POINT('Ctrl Pts',(37.7798283754123,1.15759409919791,0.486448413031079));
#35504=CARTESIAN_POINT('Ctrl Pts',(37.7806592587321,1.31732736909012,-1.86858636174431));
#35505=CARTESIAN_POINT('Ctrl Pts',(38.1455252315258,1.43803115335118,-3.71029995870316));
#35506=CARTESIAN_POINT('Ctrl Pts',(39.5779229780183,1.69365713822224,-7.16936247493209));
#35507=CARTESIAN_POINT('Ctrl Pts',(40.6266263701611,1.81514228728193,-8.73699595769941));
#35508=CARTESIAN_POINT('Ctrl Pts',(43.2633442117545,2.06643737216945,-11.3730256982204));
#35509=CARTESIAN_POINT('Ctrl Pts',(44.8298904725261,2.18792249429946,-12.4235805192368));
#35510=CARTESIAN_POINT('Ctrl Pts',(48.290206627889,2.44354852691157,-13.8529470821456));
#35511=CARTESIAN_POINT('Ctrl Pts',(50.138721549822,2.56492073913256,-14.2204718556691));
#35512=CARTESIAN_POINT('Ctrl Pts',(51.9999633056261,2.69099156569408,-14.2198708430667));
#35513=CARTESIAN_POINT('Ctrl Pts',(37.8403157026637,-1.31891566289614,1.59674345383971));
#35514=CARTESIAN_POINT('Ctrl Pts',(37.8345525884796,-1.30895607752529,1.48722862801069));
#35515=CARTESIAN_POINT('Ctrl Pts',(37.828790703466,-1.29899779261428,1.37773691225954));
#35516=CARTESIAN_POINT('Ctrl Pts',(37.8042275598881,-1.25655225280221,0.910971509135609));
#35517=CARTESIAN_POINT('Ctrl Pts',(37.7801719726404,-1.22358208074877,0.486453085748451));
#35518=CARTESIAN_POINT('Ctrl Pts',(37.779339404299,-1.06384881091203,-1.8686043109774));
#35519=CARTESIAN_POINT('Ctrl Pts',(38.1469172474041,-0.943145133364111,
-3.7097911447081));
#35520=CARTESIAN_POINT('Ctrl Pts',(39.5762884400003,-0.68751892107443,-7.17014261468754));
#35521=CARTESIAN_POINT('Ctrl Pts',(40.6268483631172,-0.566033915391893,
-8.7367057447419));
#35522=CARTESIAN_POINT('Ctrl Pts',(43.2628954695716,-0.31473877766099,-11.3734544105232));
#35523=CARTESIAN_POINT('Ctrl Pts',(44.8305401132913,-0.193253748299652,
-12.4221714958415));
#35524=CARTESIAN_POINT('Ctrl Pts',(48.2896308976067,0.0623724159563386,
-13.8545909095442));
#35525=CARTESIAN_POINT('Ctrl Pts',(50.1389656602224,0.183762141962158,-14.2195188100102));
#35526=CARTESIAN_POINT('Ctrl Pts',(51.9999633043522,0.309815399742307,-14.2201291128083));
#35527=CARTESIAN_POINT('Ctrl Pts',(40.1882694324257,-1.62853105321875,1.47327580984102));
#35528=CARTESIAN_POINT('Ctrl Pts',(40.1825065477754,-1.61857186451787,1.3637653457639));
#35529=CARTESIAN_POINT('Ctrl Pts',(40.1767441289915,-1.60861315599014,1.25426341508618));
#35530=CARTESIAN_POINT('Ctrl Pts',(40.1521822820784,-1.56616773102595,0.787522958361224));
#35531=CARTESIAN_POINT('Ctrl Pts',(40.1313396880605,-1.53342562894499,0.404565634793769));
#35532=CARTESIAN_POINT('Ctrl Pts',(40.1302905677502,-1.37533481599403,-1.55405138007464));
#35533=CARTESIAN_POINT('Ctrl Pts',(40.4394331428155,-1.25185544909165,-3.10057294640437));
#35534=CARTESIAN_POINT('Ctrl Pts',(41.6290225365131,-0.999497891516836,
-5.98227484334843));
#35535=CARTESIAN_POINT('Ctrl Pts',(42.5087254655197,-0.87586317886622,-7.29352824389111));
#35536=CARTESIAN_POINT('Ctrl Pts',(44.7059952341549,-0.62553014122646,-9.49167634236655));
#35537=CARTESIAN_POINT('Ctrl Pts',(46.018614461608,-0.501895397277342,-10.3690524867728));
#35538=CARTESIAN_POINT('Ctrl Pts',(48.898730372315,-0.249537900119364,-11.5624766483416));
#35539=CARTESIAN_POINT('Ctrl Pts',(50.4521347865894,-0.125494944822144,
-11.8682745705925));
#35540=CARTESIAN_POINT('Ctrl Pts',(51.9999864962518,-0.000622417323211651,
-11.8690397849987));
#35541=CARTESIAN_POINT('Ctrl Pts',(42.4307892712953,-2.39089944281272,1.35541200298475));
#35542=CARTESIAN_POINT('Ctrl Pts',(42.4250266056522,-2.38094063259133,1.24590570063802));
#35543=CARTESIAN_POINT('Ctrl Pts',(42.4192636830689,-2.37098151984669,1.13639402318395));
#35544=CARTESIAN_POINT('Ctrl Pts',(42.3947030499486,-2.3285362045761,0.669677370085716));
#35545=CARTESIAN_POINT('Ctrl Pts',(42.3768807775288,-2.29601193722516,0.326360253174464));
#35546=CARTESIAN_POINT('Ctrl Pts',(42.3752988309042,-2.13948974646263,-1.25364232210634));
#35547=CARTESIAN_POINT('Ctrl Pts',(42.6291645083452,-2.01335948895392,-2.51864171287222));
#35548=CARTESIAN_POINT('Ctrl Pts',(43.5891580556312,-1.7641236030149,-4.84795915808161));
#35549=CARTESIAN_POINT('Ctrl Pts',(44.3060485143003,-1.63843584903174,-5.91517020465899));
#35550=CARTESIAN_POINT('Ctrl Pts',(46.084134208595,-1.38902165105357,-7.69457540340396));
#35551=CARTESIAN_POINT('Ctrl Pts',(47.1534076509197,-1.26333384857635,-8.40795287035376));
#35552=CARTESIAN_POINT('Ctrl Pts',(49.4803356664711,-1.01409805365085,-9.37372383743556));
#35553=CARTESIAN_POINT('Ctrl Pts',(50.7512717901641,-0.887523067774766,
-9.62254086007749));
#35554=CARTESIAN_POINT('Ctrl Pts',(52.0000086453373,-0.763776277075275,
-9.62369151535372));
#35555=CARTESIAN_POINT('Ctrl Pts',(44.4816940061638,-3.5767226147739,1.24768160116169));
#35556=CARTESIAN_POINT('Ctrl Pts',(44.4759315405831,-3.5667641502963,1.13817910058646));
#35557=CARTESIAN_POINT('Ctrl Pts',(44.4701681635331,-3.55680466826894,1.02865851907984));
#35558=CARTESIAN_POINT('Ctrl Pts',(44.445608614691,-3.51435945332208,0.561963612050326));
#35559=CARTESIAN_POINT('Ctrl Pts',(44.4304979196961,-3.48203441395558,0.25484241470743));
#35560=CARTESIAN_POINT('Ctrl Pts',(44.4280873491857,-3.32694672771197,-0.978922014667701));
#35561=CARTESIAN_POINT('Ctrl Pts',(44.6319588195988,-3.19839225346,-1.98636136651175));
#35562=CARTESIAN_POINT('Ctrl Pts',(45.3813659616932,-2.95201108860042,-3.81078790536488));
#35563=CARTESIAN_POINT('Ctrl Pts',(45.9497454423979,-2.8244458583741,-4.65460264913353));
#35564=CARTESIAN_POINT('Ctrl Pts',(47.3443497895797,-2.57587192813957,-6.05121512489886));
#35565=CARTESIAN_POINT('Ctrl Pts',(48.191308984017,-2.44830662330919,-6.61423873299696));
#35566=CARTESIAN_POINT('Ctrl Pts',(50.0120953836972,-2.20192559709628,-7.37244739486701));
#35567=CARTESIAN_POINT('Ctrl Pts',(51.0248803821898,-2.07303718496541,-7.56862230181907));
#35568=CARTESIAN_POINT('Ctrl Pts',(52.0000289004077,-1.95031777657975,-7.57037421505986));
#35569=CARTESIAN_POINT('Ctrl Pts',(37.6057474666452,-4.33370633274517,1.59647061166166));
#35570=CARTESIAN_POINT('Ctrl Pts',(37.6014604087227,-4.32302794314919,1.48695576757045));
#35571=CARTESIAN_POINT('Ctrl Pts',(37.5971743516732,-4.31235100760126,1.37746396775187));
#35572=CARTESIAN_POINT('Ctrl Pts',(37.5789019782671,-4.26684181644427,0.910698635138339));
#35573=CARTESIAN_POINT('Ctrl Pts',(37.5600270135782,-4.23081870486248,0.486448413027734));
#35574=CARTESIAN_POINT('Ctrl Pts',(37.583581854176,-4.07282953634437,-1.8685863617679));
#35575=CARTESIAN_POINT('Ctrl Pts',(37.9619119570128,-4.00528018447453,-3.71029995872063));
#35576=CARTESIAN_POINT('Ctrl Pts',(39.4161093304535,-3.95610755722229,-7.1693624749145));
#35577=CARTESIAN_POINT('Ctrl Pts',(40.4714275735129,-3.98510500541578,-8.7369959576895));
#35578=CARTESIAN_POINT('Ctrl Pts',(43.1170704487074,-4.11161181540662,-11.3730256982303));
#35579=CARTESIAN_POINT('Ctrl Pts',(44.6849606627931,-4.21430601438156,-12.4235805192282));
#35580=CARTESIAN_POINT('Ctrl Pts',(48.1464351665831,-4.45373622021211,-13.8529470821542));
#35581=CARTESIAN_POINT('Ctrl Pts',(49.9934079386735,-4.59667050425296,-14.2204718556502));
#35582=CARTESIAN_POINT('Ctrl Pts',(51.8536466863968,-4.73676521641239,-14.2198708430668));
#35583=CARTESIAN_POINT('Ctrl Pts',(36.8815114147052,-4.95142919224173,1.6296460532693));
#35584=CARTESIAN_POINT('Ctrl Pts',(36.8772243107676,-4.940750688027,1.52013003367661));
#35585=CARTESIAN_POINT('Ctrl Pts',(36.8729383891546,-4.93007388724583,1.41064098631263));
#35586=CARTESIAN_POINT('Ctrl Pts',(36.8546656346322,-4.88456461021745,0.943868932681406));
#35587=CARTESIAN_POINT('Ctrl Pts',(36.8348655943188,-4.84834678143695,0.508392298457217));
#35588=CARTESIAN_POINT('Ctrl Pts',(36.857989076486,-4.68985095930904,-1.95287905126917));
#35589=CARTESIAN_POINT('Ctrl Pts',(37.2526110659712,-4.62539547707885,-3.87337387081003));
#35590=CARTESIAN_POINT('Ctrl Pts',(38.7695270468993,-4.58435548151087,-7.48792130211559));
#35591=CARTESIAN_POINT('Ctrl Pts',(39.8706950784794,-4.62052713517624,-9.12360836230037));
#35592=CARTESIAN_POINT('Ctrl Pts',(42.6325290552245,-4.76347923311373,-11.8774049927308));
#35593=CARTESIAN_POINT('Ctrl Pts',(44.2683416970863,-4.8765211889194,-12.9732563608876));
#35594=CARTESIAN_POINT('Ctrl Pts',(47.883095947851,-5.13710478161822,-14.4676858045473));
#35595=CARTESIAN_POINT('Ctrl Pts',(49.8087293766755,-5.29206142841395,-14.8501851005199));
#35596=CARTESIAN_POINT('Ctrl Pts',(51.7519872491301,-5.44377846350007,-14.8499483202528));
#35597=CARTESIAN_POINT('Ctrl Pts',(36.7461942621622,-5.89423842867652,1.62975523620908));
#35598=CARTESIAN_POINT('Ctrl Pts',(36.741907157911,-5.88355992367708,1.52023920856652));
#35599=CARTESIAN_POINT('Ctrl Pts',(36.7376212482637,-5.87288312535188,1.41075017946966));
#35600=CARTESIAN_POINT('Ctrl Pts',(36.7193484440797,-5.82737384120054,0.943978082292227));
#35601=CARTESIAN_POINT('Ctrl Pts',(36.6994509531013,-5.79114203695372,0.508394167544537));
#35602=CARTESIAN_POINT('Ctrl Pts',(36.7219158272129,-5.63255152130492,-1.95288623096384));
#35603=CARTESIAN_POINT('Ctrl Pts',(37.1176115175746,-5.56825045708003,-3.87317034521415));
#35604=CARTESIAN_POINT('Ctrl Pts',(38.6333292122811,-5.52703808205988,-7.4882333580156));
#35605=CARTESIAN_POINT('Ctrl Pts',(39.7352322893592,-5.56331547725347,-9.12349227712403));
#35606=CARTESIAN_POINT('Ctrl Pts',(42.4968007059073,-5.70622937204501,-11.8775764776452));
#35607=CARTESIAN_POINT('Ctrl Pts',(44.1330482236775,-5.81933389105681,-12.9726927515199));
#35608=CARTESIAN_POINT('Ctrl Pts',(47.7473173225335,-6.07984767624027,-14.4683433355162));
#35609=CARTESIAN_POINT('Ctrl Pts',(49.6732762742163,-6.23484434206627,-14.849803898529));
#35610=CARTESIAN_POINT('Ctrl Pts',(51.6164365682427,-6.3865541538095,-14.8500516281494));
#35611=CARTESIAN_POINT('Ctrl Pts',(37.2674545852876,-6.69072942383213,1.59674356901113));
#35612=CARTESIAN_POINT('Ctrl Pts',(37.2631675265797,-6.68005103227416,1.4872287047953));
#35613=CARTESIAN_POINT('Ctrl Pts',(37.2588814994465,-6.66937410286626,1.37773695064445));
#35614=CARTESIAN_POINT('Ctrl Pts',(37.240609001884,-6.62386489390232,0.910971509165356));
#35615=CARTESIAN_POINT('Ctrl Pts',(37.2214904105334,-6.58780684365416,0.486453085746033));
#35616=CARTESIAN_POINT('Ctrl Pts',(37.2433987309978,-6.42958094133495,-1.86860431100456));
#35617=CARTESIAN_POINT('Ctrl Pts',(37.624413086019,-6.36241763447689,-3.70979114473031));
#35618=CARTESIAN_POINT('Ctrl Pts',(39.0756147439104,-6.31281405859542,-7.17014261466511));
#35619=CARTESIAN_POINT('Ctrl Pts',(40.13277060071,-6.34207586060887,-8.73670574474625));
#35620=CARTESIAN_POINT('Ctrl Pts',(42.7777495754168,-6.46848716273484,-11.3734544105186));
#35621=CARTESIAN_POINT('Ctrl Pts',(44.3467269792879,-6.57133776972387,-12.4221714958281));
#35622=CARTESIAN_POINT('Ctrl Pts',(47.8069886032727,-6.81059345676843,-13.8545909095574));
#35623=CARTESIAN_POINT('Ctrl Pts',(49.6547753637234,-6.95362708078685,-14.2195188099959));
#35624=CARTESIAN_POINT('Ctrl Pts',(51.5147699841783,-7.093704442186,-14.2201291128083));
#35625=CARTESIAN_POINT('Ctrl Pts',(37.5648924257371,-4.19818497005578,0.));
#35626=CARTESIAN_POINT('Ctrl Pts',(37.583581854176,-4.07282953634436,-1.86858636176791));
#35627=CARTESIAN_POINT('Ctrl Pts',(37.9619119570128,-4.00528018447453,-3.71029995872063));
#35628=CARTESIAN_POINT('Ctrl Pts',(39.4161093304535,-3.95610755722229,-7.1693624749145));
#35629=CARTESIAN_POINT('Ctrl Pts',(40.4714275735129,-3.98510500541578,-8.7369959576895));
#35630=CARTESIAN_POINT('Ctrl Pts',(41.9288128067803,-4.05479285275038,-10.1890856763502));
#35631=CARTESIAN_POINT('Ctrl Pts',(42.0659125600698,-4.06163542615967,-10.320392863517));
#35632=CARTESIAN_POINT('Ctrl Pts',(42.2054617208597,-4.06886253050386,-10.4488603765996));
#35633=CARTESIAN_POINT('Ctrl Pts',(37.2260157226955,-6.55512420933908,-4.87766791140768E-9));
#35634=CARTESIAN_POINT('Ctrl Pts',(37.2433987315464,-6.42958094104316,-1.8686043142306));
#35635=CARTESIAN_POINT('Ctrl Pts',(37.6244130865613,-6.36241763431395,-3.70979114626806));
#35636=CARTESIAN_POINT('Ctrl Pts',(38.3500139148987,-6.33761584642798,-5.43996687972819));
#35637=CARTESIAN_POINT('Ctrl Pts',(39.0756147438694,-6.31281405852036,-7.17014261469875));
#35638=CARTESIAN_POINT('Ctrl Pts',(40.1327706006907,-6.34207586056676,-8.73670574476976));
#35639=CARTESIAN_POINT('Ctrl Pts',(41.4552600880589,-6.40528151166162,-10.0550800776384));
#35640=CARTESIAN_POINT('Ctrl Pts',(41.5972271209431,-6.41206653251295,-10.196605355575));
#35641=CARTESIAN_POINT('Ctrl Pts',(41.7420345975448,-6.41930840848147,-10.3350231942279));
#35642=CARTESIAN_POINT('Ctrl Pts',(41.8895769551558,-6.42697885114752,-10.4702558450972));
#35643=CARTESIAN_POINT('Ctrl Pts',(44.5001944306518,-3.04071090848738,1.24689076028073));
#35644=CARTESIAN_POINT('Ctrl Pts',(44.4959078567059,-3.03003372440451,1.13738827962796));
#35645=CARTESIAN_POINT('Ctrl Pts',(44.4916204363964,-3.01935537993571,1.02786752740425));
#35646=CARTESIAN_POINT('Ctrl Pts',(44.4733518105209,-2.97384705570815,0.561172897423655));
#35647=CARTESIAN_POINT('Ctrl Pts',(44.463701217072,-2.93980180525762,0.254828874440047));
#35648=CARTESIAN_POINT('Ctrl Pts',(44.488157628544,-2.78663561817574,-0.97887000267835));
#35649=CARTESIAN_POINT('Ctrl Pts',(44.7004709588316,-2.68728492516155,-1.98783577086809));
#35650=CARTESIAN_POINT('Ctrl Pts',(45.4859946801691,-2.55131209325765,-3.80852727285718));
#35651=CARTESIAN_POINT('Ctrl Pts',(46.0614183982484,-2.50516810167956,-4.65544360722297));
#35652=CARTESIAN_POINT('Ctrl Pts',(47.4791272455479,-2.45787394350806,-6.04997283343074));
#35653=CARTESIAN_POINT('Ctrl Pts',(48.3324696724574,-2.45168870251593,-6.61832169902524));
#35654=CARTESIAN_POINT('Ctrl Pts',(50.1733013630956,-2.46744610981745,-7.36768403079182));
#35655=CARTESIAN_POINT('Ctrl Pts',(51.1917533012975,-2.48375959424081,-7.57138648676607));
#35656=CARTESIAN_POINT('Ctrl Pts',(52.1751568070596,-2.50107414862821,-7.56962581969462));
#35657=CARTESIAN_POINT('Ctrl Pts',(42.3018453782486,-3.92365461890892,1.35489314066083));
#35658=CARTESIAN_POINT('Ctrl Pts',(42.2975586546956,-3.91297706217431,1.24538683818609));
#35659=CARTESIAN_POINT('Ctrl Pts',(42.2932716614843,-3.90229915402469,1.13587503551432));
#35660=CARTESIAN_POINT('Ctrl Pts',(42.275001852934,-3.85679055844476,0.669158551007349));
#35661=CARTESIAN_POINT('Ctrl Pts',(42.2624528820614,-3.82212739678043,0.326351368869398));
#35662=CARTESIAN_POINT('Ctrl Pts',(42.2862930185905,-3.66742334692941,-1.25360819499453));
#35663=CARTESIAN_POINT('Ctrl Pts',(42.5504213117423,-3.57797177381408,-2.5196091277947));
#35664=CARTESIAN_POINT('Ctrl Pts',(43.5418092681772,-3.46871344469322,-4.84647586782627));
#35665=CARTESIAN_POINT('Ctrl Pts',(44.2657961681648,-3.44582654102279,-5.91572199046432));
#35666=CARTESIAN_POINT('Ctrl Pts',(46.0625411381427,-3.45218058836019,-7.69376028692298));
#35667=CARTESIAN_POINT('Ctrl Pts',(47.1367510692373,-3.47964820283172,-8.41063186557179));
#35668=CARTESIAN_POINT('Ctrl Pts',(49.4777703293181,-3.56443746806574,-9.3705984061947));
#35669=CARTESIAN_POINT('Ctrl Pts',(50.7522326212184,-3.61985039973288,-9.62435378619005));
#35670=CARTESIAN_POINT('Ctrl Pts',(52.0063376889004,-3.67509457152228,-9.62320046360564));
#35671=CARTESIAN_POINT('Ctrl Pts',(39.9738746787522,-4.36024590432593,1.47293185433834));
#35672=CARTESIAN_POINT('Ctrl Pts',(39.9695877917789,-4.3495679405393,1.36342137723986));
#35673=CARTESIAN_POINT('Ctrl Pts',(39.965301258885,-4.33889050812412,1.2539193506024));
#35674=CARTESIAN_POINT('Ctrl Pts',(39.9470301849507,-4.29338161981782,0.787178992729243));
#35675=CARTESIAN_POINT('Ctrl Pts',(39.9313665239358,-4.25805061593422,0.404559744693875));
#35676=CARTESIAN_POINT('Ctrl Pts',(39.9549022371336,-4.10171804395135,-1.55402875456025));
#35677=CARTESIAN_POINT('Ctrl Pts',(40.2750875547397,-4.02300447357647,-3.10121432124357));
#35678=CARTESIAN_POINT('Ctrl Pts',(41.4922590552009,-3.94305499753475,-5.98129145450059));
#35679=CARTESIAN_POINT('Ctrl Pts',(42.3782865653796,-3.94554026236852,-7.29389406575307));
#35680=CARTESIAN_POINT('Ctrl Pts',(44.589654267654,-4.01057973632999,-9.49113593805367));
#35681=CARTESIAN_POINT('Ctrl Pts',(45.9051375482496,-4.07481145201866,-10.3708286017226));
#35682=CARTESIAN_POINT('Ctrl Pts',(48.7933811184127,-4.2351258063533,-11.5604045561197));
#35683=CARTESIAN_POINT('Ctrl Pts',(50.3476002080607,-4.33329690122034,-11.8694761541096));
#35684=CARTESIAN_POINT('Ctrl Pts',(51.8977769668582,-4.42999533819711,-11.8687142284813));
#35685=CARTESIAN_POINT('Ctrl Pts',(37.6057474666452,-4.33370633274517,1.59647061166166));
#35686=CARTESIAN_POINT('Ctrl Pts',(37.6014604087227,-4.32302794314919,1.48695576757045));
#35687=CARTESIAN_POINT('Ctrl Pts',(37.5971743516732,-4.31235100760126,1.37746396775187));
#35688=CARTESIAN_POINT('Ctrl Pts',(37.5789019782671,-4.26684181644427,0.910698635138339));
#35689=CARTESIAN_POINT('Ctrl Pts',(37.5600270135782,-4.23081870486248,0.486448413027734));
#35690=CARTESIAN_POINT('Ctrl Pts',(37.583581854176,-4.07282953634436,-1.8685863617679));
#35691=CARTESIAN_POINT('Ctrl Pts',(37.9619119570128,-4.00528018447453,-3.71029995872063));
#35692=CARTESIAN_POINT('Ctrl Pts',(39.4161093304535,-3.95610755722229,-7.1693624749145));
#35693=CARTESIAN_POINT('Ctrl Pts',(40.4714275735129,-3.98510500541578,-8.7369959576895));
#35694=CARTESIAN_POINT('Ctrl Pts',(43.1170704487074,-4.11161181540662,-11.3730256982303));
#35695=CARTESIAN_POINT('Ctrl Pts',(44.6849606627931,-4.21430601438036,-12.4235805192282));
#35696=CARTESIAN_POINT('Ctrl Pts',(48.1464351665831,-4.45373622021331,-13.8529470821542));
#35697=CARTESIAN_POINT('Ctrl Pts',(49.9934079386734,-4.59667050425296,-14.2204718556502));
#35698=CARTESIAN_POINT('Ctrl Pts',(51.8536466863968,-4.73676521641239,-14.2198708430668));
#35699=CARTESIAN_POINT('Ctrl Pts',(37.2674545852876,-6.69072942383213,1.59674356901113));
#35700=CARTESIAN_POINT('Ctrl Pts',(37.2631675265797,-6.68005103227415,1.4872287047953));
#35701=CARTESIAN_POINT('Ctrl Pts',(37.2588814994465,-6.66937410286626,1.37773695064445));
#35702=CARTESIAN_POINT('Ctrl Pts',(37.240609001884,-6.62386489390232,0.910971509165356));
#35703=CARTESIAN_POINT('Ctrl Pts',(37.2214904105334,-6.58780684365416,0.486453085746033));
#35704=CARTESIAN_POINT('Ctrl Pts',(37.2433987309978,-6.42958094133495,-1.86860431100456));
#35705=CARTESIAN_POINT('Ctrl Pts',(37.624413086019,-6.36241763447689,-3.70979114473031));
#35706=CARTESIAN_POINT('Ctrl Pts',(39.0756147439104,-6.31281405859542,-7.17014261466511));
#35707=CARTESIAN_POINT('Ctrl Pts',(40.13277060071,-6.34207586060887,-8.73670574474625));
#35708=CARTESIAN_POINT('Ctrl Pts',(42.7777495754168,-6.46848716273484,-11.3734544105186));
#35709=CARTESIAN_POINT('Ctrl Pts',(44.3467269792879,-6.57133776972387,-12.4221714958281));
#35710=CARTESIAN_POINT('Ctrl Pts',(47.8069886032727,-6.81059345676843,-13.8545909095574));
#35711=CARTESIAN_POINT('Ctrl Pts',(49.6547753637234,-6.95362708078685,-14.2195188099959));
#35712=CARTESIAN_POINT('Ctrl Pts',(51.5147699841783,-7.093704442186,-14.2201291128083));
#35713=CARTESIAN_POINT('Ctrl Pts',(39.5474466673498,-7.33134203123383,1.47327592501242));
#35714=CARTESIAN_POINT('Ctrl Pts',(39.5431597793878,-7.32066406497413,1.36376542254622));
#35715=CARTESIAN_POINT('Ctrl Pts',(39.5388732842035,-7.3099866402986,1.25426345347434));
#35716=CARTESIAN_POINT('Ctrl Pts',(39.5206020537639,-7.26447772954601,0.787522958372976));
#35717=CARTESIAN_POINT('Ctrl Pts',(39.5046312942629,-7.22910268445771,0.404565634791133));
#35718=CARTESIAN_POINT('Ctrl Pts',(39.5260915209589,-7.07247170263716,-1.55405138009485));
#35719=CARTESIAN_POINT('Ctrl Pts',(39.8496604164864,-6.99424475322044,-3.10057294641932));
#35720=CARTESIAN_POINT('Ctrl Pts',(41.0630557304034,-6.91375205390619,-5.98227484333336));
#35721=CARTESIAN_POINT('Ctrl Pts',(41.9513996061261,-6.91657054441245,-7.29352824389794));
#35722=CARTESIAN_POINT('Ctrl Pts',(44.1619304425351,-6.98148962793616,-9.4916763423596));
#35723=CARTESIAN_POINT('Ctrl Pts',(45.4787841574493,-7.0459185004724,-10.3690524867687));
#35724=CARTESIAN_POINT('Ctrl Pts',(48.3654988573818,-7.20601286880373,-11.5624766483454));
#35725=CARTESIAN_POINT('Ctrl Pts',(49.9207450076504,-7.30430498992435,-11.8682745706019));
#35726=CARTESIAN_POINT('Ctrl Pts',(51.4706130322883,-7.40098575043949,-11.8690397849986));
#35727=CARTESIAN_POINT('Ctrl Pts',(41.6586445536367,-8.40509445805938,1.35541211815617));
#35728=CARTESIAN_POINT('Ctrl Pts',(41.6543578285897,-8.39441689759457,1.24590577741826));
#35729=CARTESIAN_POINT('Ctrl Pts',(41.6500708922589,-8.38373900111893,1.13639406157512));
#35730=CARTESIAN_POINT('Ctrl Pts',(41.6318008476496,-8.33823037168233,0.669677370080662));
#35731=CARTESIAN_POINT('Ctrl Pts',(41.6187886661145,-8.30350078066026,0.326360253171814));
#35732=CARTESIAN_POINT('Ctrl Pts',(41.6394982516696,-8.14834662563339,-1.25364232212061));
#35733=CARTESIAN_POINT('Ctrl Pts',(41.9087301497588,-8.05962904511281,-2.51864171287989));
#35734=CARTESIAN_POINT('Ctrl Pts',(42.8944223117582,-7.94955134754687,-4.8479591580739));
#35735=CARTESIAN_POINT('Ctrl Pts',(43.621903091562,-7.92716706336173,-5.91517020467067));
#35736=CARTESIAN_POINT('Ctrl Pts',(45.4173857785914,-7.93333952030752,-7.69457540339218));
#35737=CARTESIAN_POINT('Ctrl Pts',(46.4936627982988,-7.96110451544899,-8.40795287034955));
#35738=CARTESIAN_POINT('Ctrl Pts',(48.8323759936291,-8.04556196575582,-9.37372383743957));
#35739=CARTESIAN_POINT('Ctrl Pts',(50.1083893187855,-8.1011483996294,-9.62254086008693));
#35740=CARTESIAN_POINT('Ctrl Pts',(51.3620268377998,-8.15637495641971,-9.62369151535362));
#35741=CARTESIAN_POINT('Ctrl Pts',(43.5199138025263,-9.87072183560237,1.24768171633309));
#35742=CARTESIAN_POINT('Ctrl Pts',(43.5156272263023,-9.86004464583426,1.13817917736476));
#35743=CARTESIAN_POINT('Ctrl Pts',(43.5113398926843,-9.84936631915757,1.02865855747361));
#35744=CARTESIAN_POINT('Ctrl Pts',(43.4930709070365,-9.80385794333019,0.561963612030324));
#35745=CARTESIAN_POINT('Ctrl Pts',(43.4827143498846,-9.76971145014119,0.254842414704953));
#35746=CARTESIAN_POINT('Ctrl Pts',(43.5023995944571,-9.61585927298276,-0.978922014677277));
#35747=CARTESIAN_POINT('Ctrl Pts',(43.7224911564668,-9.51762723326116,-1.98636136651214));
#35748=CARTESIAN_POINT('Ctrl Pts',(44.4993341101079,-9.38040562961654,-3.81078790536449));
#35749=CARTESIAN_POINT('Ctrl Pts',(45.0800827322703,-9.33502766340239,-4.65460264915721));
#35750=CARTESIAN_POINT('Ctrl Pts',(46.495867776811,-9.28745674945108,-6.05121512487505));
#35751=CARTESIAN_POINT('Ctrl Pts',(47.3523605835685,-9.28172473628545,-6.61423873299739));
#35752=CARTESIAN_POINT('Ctrl Pts',(49.1896776789186,-9.2969764356746,-7.37244739486635));
#35753=CARTESIAN_POINT('Ctrl Pts',(50.2104967200023,-9.31353425501145,-7.56862230181894));
#35754=CARTESIAN_POINT('Ctrl Pts',(51.1931844250963,-9.33084205690778,-7.5703742150597));
#35755=CARTESIAN_POINT('Ctrl Pts',(36.6062244663074,-9.64145132693369,1.5964706812661));
#35756=CARTESIAN_POINT('Ctrl Pts',(36.5951848118711,-9.59613798296326,1.15259163662005));
#35757=CARTESIAN_POINT('Ctrl Pts',(36.5727117312847,-9.54279427445071,0.635573001824062));
#35758=CARTESIAN_POINT('Ctrl Pts',(36.6214111051582,-9.38007537751166,-1.86858636169253));
#35759=CARTESIAN_POINT('Ctrl Pts',(37.005503628143,-9.36705556805879,-3.71029995870864));
#35760=CARTESIAN_POINT('Ctrl Pts',(38.4518973636206,-9.52533731123247,-7.16936247492662));
#35761=CARTESIAN_POINT('Ctrl Pts',(39.492347221447,-9.70422705237809,-8.73699595770811));
#35762=CARTESIAN_POINT('Ctrl Pts',(42.0930574706692,-10.2059604432482,-11.3730256982116));
#35763=CARTESIAN_POINT('Ctrl Pts',(43.6303739147809,-10.5307434056714,-12.4235805192465));
#35764=CARTESIAN_POINT('Ctrl Pts',(47.0225411281103,-11.260355741399,-13.8529470821356));
#35765=CARTESIAN_POINT('Ctrl Pts',(48.830372711006,-11.664686791883,-14.2204718556452));
#35766=CARTESIAN_POINT('Ctrl Pts',(50.6517393542017,-12.0680951184149,-14.2198708430666));
#35767=CARTESIAN_POINT('Ctrl Pts',(35.8014489642672,-10.1498171217999,1.62964612287371));
#35768=CARTESIAN_POINT('Ctrl Pts',(35.7905014108312,-10.1048818153799,1.18947024667652));
#35769=CARTESIAN_POINT('Ctrl Pts',(35.7670704718575,-10.0508712183064,0.664243958000225));
#35770=CARTESIAN_POINT('Ctrl Pts',(35.8153925117057,-9.88755379325372,-1.95287905117699));
#35771=CARTESIAN_POINT('Ctrl Pts',(36.215170789872,-9.87991493952696,-3.87337387079453));
#35772=CARTESIAN_POINT('Ctrl Pts',(37.7224873536725,-10.0551723243901,-7.4879213021314));
#35773=CARTESIAN_POINT('Ctrl Pts',(38.8072993194045,-10.2476883531955,-9.12360836232144));
#35774=CARTESIAN_POINT('Ctrl Pts',(41.520677603786,-10.7822353604969,-11.8774049927099));
#35775=CARTESIAN_POINT('Ctrl Pts',(43.1237524839592,-11.1269271238462,-12.9732563609012));
#35776=CARTESIAN_POINT('Ctrl Pts',(46.6646288366278,-11.8992915178566,-14.4676858045336));
#35777=CARTESIAN_POINT('Ctrl Pts',(48.5486094635743,-12.3267171394201,-14.8501851005103));
#35778=CARTESIAN_POINT('Ctrl Pts',(50.4504961875093,-12.7534443437025,-14.8499483202528));
#35779=CARTESIAN_POINT('Ctrl Pts',(35.5333334012201,-11.0637722809467,1.62975530581349));
#35780=CARTESIAN_POINT('Ctrl Pts',(35.5223873364831,-11.0188430850085,1.18963928646871));
#35781=CARTESIAN_POINT('Ctrl Pts',(35.4989008284158,-10.9648105349846,0.664246400070066));
#35782=CARTESIAN_POINT('Ctrl Pts',(35.5465440138856,-10.8012937803281,-1.95288623086898));
#35783=CARTESIAN_POINT('Ctrl Pts',(35.947363088238,-10.7939605764187,-3.87317034519632));
#35784=CARTESIAN_POINT('Ctrl Pts',(37.453518094782,-10.9688768024953,-7.48823335803387));
#35785=CARTESIAN_POINT('Ctrl Pts',(38.5390425757361,-11.1616021044182,-9.12349227713323));
#35786=CARTESIAN_POINT('Ctrl Pts',(41.2521634397981,-11.6960735042602,-11.8775764776363));
#35787=CARTESIAN_POINT('Ctrl Pts',(42.855659865817,-12.0408890833115,-12.9726927515384));
#35788=CARTESIAN_POINT('Ctrl Pts',(46.3960659393469,-12.8131153360318,-14.468343335498));
#35789=CARTESIAN_POINT('Ctrl Pts',(48.280363080515,-13.2406268960268,-14.8498038985481));
#35790=CARTESIAN_POINT('Ctrl Pts',(50.1821542472111,-13.6673330636266,-14.8500516281495));
#35791=CARTESIAN_POINT('Ctrl Pts',(35.9359355586898,-11.9263392248007,1.59674363861555));
#35792=CARTESIAN_POINT('Ctrl Pts',(35.9248996260065,-11.8810411570359,1.15301423610032));
#35793=CARTESIAN_POINT('Ctrl Pts',(35.9022876226764,-11.827642566146,0.63557910699865));
#35794=CARTESIAN_POINT('Ctrl Pts',(35.9492898606198,-11.6644253451977,-1.8686043109225));
#35795=CARTESIAN_POINT('Ctrl Pts',(36.335984374051,-11.6521696602917,-3.70979114471011));
#35796=CARTESIAN_POINT('Ctrl Pts',(37.7794742164015,-11.8095985064919,-7.1701426146858));
#35797=CARTESIAN_POINT('Ctrl Pts',(38.8217053622758,-11.9890114304293,-8.73670574474357));
#35798=CARTESIAN_POINT('Ctrl Pts',(41.4217720606995,-12.4905558026619,-11.3734544105218));
#35799=CARTESIAN_POINT('Ctrl Pts',(42.9601423694208,-12.81564830434,-12.4221714958419));
#35800=CARTESIAN_POINT('Ctrl Pts',(46.3511338849127,-13.5449152868315,-13.854590909544));
#35801=CARTESIAN_POINT('Ctrl Pts',(48.1597570333989,-13.9494605087848,-14.2195188100056));
#35802=CARTESIAN_POINT('Ctrl Pts',(49.9808845034561,-14.3528169182251,-14.2201291128085));
#35803=CARTESIAN_POINT('Ctrl Pts',(36.5850719698904,-9.50149509066561,0.));
#35804=CARTESIAN_POINT('Ctrl Pts',(36.6214111051582,-9.38007537751166,-1.86858636169253));
#35805=CARTESIAN_POINT('Ctrl Pts',(37.005503628143,-9.36705556805998,-3.71029995870864));
#35806=CARTESIAN_POINT('Ctrl Pts',(38.4518973636206,-9.52533731123127,-7.16936247492662));
#35807=CARTESIAN_POINT('Ctrl Pts',(39.492347221447,-9.70422705237809,-8.7369959577105));
#35808=CARTESIAN_POINT('Ctrl Pts',(40.9249807596937,-9.98061312161967,-10.1890856763493));
#35809=CARTESIAN_POINT('Ctrl Pts',(41.0597112354494,-10.0068973767103,-10.3203928635158));
#35810=CARTESIAN_POINT('Ctrl Pts',(41.1968114628114,-10.0339108357988,-10.4488603765985));
#35811=CARTESIAN_POINT('Ctrl Pts',(35.9142171164209,-11.7862169042736,-4.44089209850063E-16));
#35812=CARTESIAN_POINT('Ctrl Pts',(35.9492898606198,-11.6644253451977,-1.8686043109225));
#35813=CARTESIAN_POINT('Ctrl Pts',(36.335984374051,-11.6521696602917,-3.70979114471011));
#35814=CARTESIAN_POINT('Ctrl Pts',(37.7794742164015,-11.8095985064919,-7.1701426146858));
#35815=CARTESIAN_POINT('Ctrl Pts',(38.8217053622758,-11.9890114304293,-8.73670574474357));
#35816=CARTESIAN_POINT('Ctrl Pts',(40.2612951155294,-12.2667035909826,-10.196605355573));
#35817=CARTESIAN_POINT('Ctrl Pts',(40.4035980344059,-12.2944800077005,-10.3350231942297));
#35818=CARTESIAN_POINT('Ctrl Pts',(40.5485470057469,-12.3230698430749,-10.4702558451028));
#35819=CARTESIAN_POINT('Ctrl Pts',(43.6145083358835,-9.34279883641536,1.24689082988539));
#35820=CARTESIAN_POINT('Ctrl Pts',(43.6025047583517,-9.2935289757009,0.764254661689123));
#35821=CARTESIAN_POINT('Ctrl Pts',(43.5898343019063,-9.24710292813879,0.332948671149295));
#35822=CARTESIAN_POINT('Ctrl Pts',(43.6387527331667,-9.08959664355163,-0.978870002765541));
#35823=CARTESIAN_POINT('Ctrl Pts',(43.8630440977107,-9.02147253459711,-1.98783577089164));
#35824=CARTESIAN_POINT('Ctrl Pts',(44.6599232717754,-8.99867539146223,-3.80852727283284));
#35825=CARTESIAN_POINT('Ctrl Pts',(45.2360569807709,-9.03489241248372,-4.65544360723186));
#35826=CARTESIAN_POINT('Ctrl Pts',(46.6460662566965,-9.18984064609203,-6.04997283342104));
#35827=CARTESIAN_POINT('Ctrl Pts',(47.4916031396324,-9.30516165132963,-6.61832169902913));
#35828=CARTESIAN_POINT('Ctrl Pts',(49.3114553051098,-9.58273633533165,-7.3676840307869));
#35829=CARTESIAN_POINT('Ctrl Pts',(50.3172192201087,-9.74382459488535,-7.57138648674191));
#35830=CARTESIAN_POINT('Ctrl Pts',(51.2881489781557,-9.90091582292662,-7.56962581969414));
#35831=CARTESIAN_POINT('Ctrl Pts',(41.3128793157231,-9.90389776310366,1.35489321026542));
#35832=CARTESIAN_POINT('Ctrl Pts',(41.3011741506616,-9.85585276552939,0.884255518280862));
#35833=CARTESIAN_POINT('Ctrl Pts',(41.2854482448493,-9.80727935893269,0.426396949030956));
#35834=CARTESIAN_POINT('Ctrl Pts',(41.3339507669543,-9.64806121735613,-1.25360819503015));
#35835=CARTESIAN_POINT('Ctrl Pts',(41.6081209011006,-9.59710950760114,-2.51960912780404));
#35836=CARTESIAN_POINT('Ctrl Pts',(42.6049670390268,-9.63005248743076,-4.84647586781651));
#35837=CARTESIAN_POINT('Ctrl Pts',(43.3248419422611,-9.71043261799562,-5.91572199047331));
#35838=CARTESIAN_POINT('Ctrl Pts',(45.1023943639496,-9.97242546015736,-7.69376028691353));
#35839=CARTESIAN_POINT('Ctrl Pts',(46.1617613376869,-10.152489506502,-8.41063186557578));
#35840=CARTESIAN_POINT('Ctrl Pts',(48.4668856266305,-10.5695775166851,-9.37059840619009));
#35841=CARTESIAN_POINT('Ctrl Pts',(49.7204896475851,-10.8058013195656,-9.62435378619457));
#35842=CARTESIAN_POINT('Ctrl Pts',(50.9539676685887,-11.0389609452148,-9.62320046360532));
#35843=CARTESIAN_POINT('Ctrl Pts',(38.9464705831154,-10.0047404051441,1.47293192394285));
#35844=CARTESIAN_POINT('Ctrl Pts',(38.9350908951694,-9.95803136027261,1.0153809158493));
#35845=CARTESIAN_POINT('Ctrl Pts',(38.9160550470399,-9.90712214456902,0.528580717858753));
#35846=CARTESIAN_POINT('Ctrl Pts',(38.9644836024862,-9.74614391855282,-1.55402875454098));
#35847=CARTESIAN_POINT('Ctrl Pts',(39.2926120042887,-9.71379866053015,-3.10121432124465));
#35848=CARTESIAN_POINT('Ctrl Pts',(40.5087724506345,-9.80788452010349,-5.98129145449939));
#35849=CARTESIAN_POINT('Ctrl Pts',(41.3854277882457,-9.93643935036519,-7.29389406576689));
#35850=CARTESIAN_POINT('Ctrl Pts',(43.565030873626,-10.3155272531378,-9.49113593803963));
#35851=CARTESIAN_POINT('Ctrl Pts',(44.8579833049588,-10.5663179729255,-10.3708286017266));
#35852=CARTESIAN_POINT('Ctrl Pts',(47.6940136086793,-11.1360404748617,-11.5604045561153));
#35853=CARTESIAN_POINT('Ctrl Pts',(49.2184417854976,-11.4544007679218,-11.8694761540999));
#35854=CARTESIAN_POINT('Ctrl Pts',(50.7390783576437,-11.7707281089613,-11.8687142284811));
#35855=CARTESIAN_POINT('Ctrl Pts',(36.6062244663074,-9.64145132693368,1.5964706812661));
#35856=CARTESIAN_POINT('Ctrl Pts',(36.595184811871,-9.59613798296326,1.15259163662005));
#35857=CARTESIAN_POINT('Ctrl Pts',(36.5727117312847,-9.54279427445071,0.635573001824062));
#35858=CARTESIAN_POINT('Ctrl Pts',(36.6214111051582,-9.38007537751166,-1.86858636169253));
#35859=CARTESIAN_POINT('Ctrl Pts',(37.005503628143,-9.36705556805998,-3.71029995870864));
#35860=CARTESIAN_POINT('Ctrl Pts',(38.4518973636206,-9.52533731123127,-7.16936247492662));
#35861=CARTESIAN_POINT('Ctrl Pts',(39.492347221447,-9.70422705237809,-8.7369959577105));
#35862=CARTESIAN_POINT('Ctrl Pts',(42.0930574706692,-10.2059604432482,-11.3730256982092));
#35863=CARTESIAN_POINT('Ctrl Pts',(43.6303739147809,-10.5307434056702,-12.4235805192465));
#35864=CARTESIAN_POINT('Ctrl Pts',(47.0225411281103,-11.2603557414002,-13.8529470821356));
#35865=CARTESIAN_POINT('Ctrl Pts',(48.830372711005,-11.6646867918863,-14.2204718556452));
#35866=CARTESIAN_POINT('Ctrl Pts',(50.6517393542018,-12.0680951184149,-14.2198708430666));
#35867=CARTESIAN_POINT('Ctrl Pts',(35.9359355586898,-11.9263392248007,1.59674363861555));
#35868=CARTESIAN_POINT('Ctrl Pts',(35.9248996260064,-11.8810411570359,1.15301423610033));
#35869=CARTESIAN_POINT('Ctrl Pts',(35.9022876226764,-11.827642566146,0.63557910699865));
#35870=CARTESIAN_POINT('Ctrl Pts',(35.9492898606198,-11.6644253451977,-1.8686043109225));
#35871=CARTESIAN_POINT('Ctrl Pts',(36.335984374051,-11.6521696602917,-3.70979114471011));
#35872=CARTESIAN_POINT('Ctrl Pts',(37.7794742164015,-11.8095985064919,-7.1701426146858));
#35873=CARTESIAN_POINT('Ctrl Pts',(38.8217053622758,-11.9890114304293,-8.73670574474597));
#35874=CARTESIAN_POINT('Ctrl Pts',(41.4217720606995,-12.4905558026619,-11.3734544105194));
#35875=CARTESIAN_POINT('Ctrl Pts',(42.960142369416,-12.81564830434,-12.4221714958419));
#35876=CARTESIAN_POINT('Ctrl Pts',(46.3511338849175,-13.5449152868315,-13.854590909544));
#35877=CARTESIAN_POINT('Ctrl Pts',(48.1597570333954,-13.949460508784,-14.2195188100056));
#35878=CARTESIAN_POINT('Ctrl Pts',(49.9808845034561,-14.3528169182251,-14.2201291128085));
#35879=CARTESIAN_POINT('Ctrl Pts',(38.1015519292155,-12.8849080239691,1.47327599461691));
#35880=CARTESIAN_POINT('Ctrl Pts',(38.0901769326353,-12.8382182351976,1.01591361478005));
#35881=CARTESIAN_POINT('Ctrl Pts',(38.0709659683616,-12.7872398386631,0.528588413608809));
#35882=CARTESIAN_POINT('Ctrl Pts',(38.1172552346281,-12.6256334607469,-1.55405138006716));
#35883=CARTESIAN_POINT('Ctrl Pts',(38.4486635210265,-12.594251403927,-3.10057294640624));
#35884=CARTESIAN_POINT('Ctrl Pts',(39.6611635256788,-12.6872621620748,-5.98227484334677));
#35885=CARTESIAN_POINT('Ctrl Pts',(40.5400642286605,-12.8164764794555,-7.29352824388334));
#35886=CARTESIAN_POINT('Ctrl Pts',(42.7188560995337,-13.1953261187354,-9.49167634237456));
#35887=CARTESIAN_POINT('Ctrl Pts',(44.0131369578425,-13.4465070217538,-10.3690524867684));
#35888=CARTESIAN_POINT('Ctrl Pts',(46.8476852602796,-14.0157941958989,-11.5624766483463));
#35889=CARTESIAN_POINT('Ctrl Pts',(48.3731128199089,-14.3344204493097,-11.8682745705926));
#35890=CARTESIAN_POINT('Ctrl Pts',(49.8934463159786,-14.650686356357,-11.8690397849988));
#35891=CARTESIAN_POINT('Ctrl Pts',(40.0384499621468,-14.2481859850624,1.35541218776073));
#35892=CARTESIAN_POINT('Ctrl Pts',(40.0267518732903,-14.2001700323427,0.885059012381398));
#35893=CARTESIAN_POINT('Ctrl Pts',(40.0107618318057,-14.1514922771428,0.426408556881866));
#35894=CARTESIAN_POINT('Ctrl Pts',(40.0560375664345,-13.9913266653943,-1.25364232214352));
#35895=CARTESIAN_POINT('Ctrl Pts',(40.3351549001603,-13.9418277959606,-2.51864171287518));
#35896=CARTESIAN_POINT('Ctrl Pts',(41.3264798268773,-13.9731491512594,-4.84795915807886));
#35897=CARTESIAN_POINT('Ctrl Pts',(42.0497415171332,-14.0545240163318,-5.91517020463943));
#35898=CARTESIAN_POINT('Ctrl Pts',(43.8260703469873,-14.316157474802,-7.69457540342382));
#35899=CARTESIAN_POINT('Ctrl Pts',(44.887441047737,-14.4968100523122,-8.40795287033977));
#35900=CARTESIAN_POINT('Ctrl Pts',(47.1903299665195,-14.9132414377274,-9.37372383744997));
#35901=CARTESIAN_POINT('Ctrl Pts',(48.4454445415193,-15.1498577118716,-9.62254086007292));
#35902=CARTESIAN_POINT('Ctrl Pts',(49.678462279699,-15.3829333626946,-9.62369151535395));
#35903=CARTESIAN_POINT('Ctrl Pts',(41.6721936506076,-15.9637816213008,1.24768178593771));
#35904=CARTESIAN_POINT('Ctrl Pts',(41.6602008577063,-15.9145560268665,0.765479239878682));
#35905=CARTESIAN_POINT('Ctrl Pts',(41.6471278409845,-15.8679709451274,0.332966362282368));
#35906=CARTESIAN_POINT('Ctrl Pts',(41.6911284345756,-15.7090206532874,-0.978922014745105));
#35907=CARTESIAN_POINT('Ctrl Pts',(41.922959658712,-15.6431107691407,-1.98636136650983));
#35908=CARTESIAN_POINT('Ctrl Pts',(42.7114241414519,-15.6178421628933,-3.81078790536703));
#35909=CARTESIAN_POINT('Ctrl Pts',(43.2927195380239,-15.6555752251425,-4.65460264909979));
#35910=CARTESIAN_POINT('Ctrl Pts',(44.7008639790291,-15.8099757342161,-6.051215124933));
#35911=CARTESIAN_POINT('Ctrl Pts',(45.5494546745409,-15.9261936999035,-6.61423873298305));
#35912=CARTESIAN_POINT('Ctrl Pts',(47.3658999879423,-16.2027676443008,-7.37244739488157));
#35913=CARTESIAN_POINT('Ctrl Pts',(48.3739721396802,-16.3644346256642,-7.56862230182889));
#35914=CARTESIAN_POINT('Ctrl Pts',(49.3441943438428,-16.5214173008841,-7.5703742150602));
#35915=CARTESIAN_POINT('Ctrl Pts',(34.8615042977018,-14.7529241788872,1.596470776103));
#35916=CARTESIAN_POINT('Ctrl Pts',(34.8570257719499,-14.7065009496497,1.15259170141934));
#35917=CARTESIAN_POINT('Ctrl Pts',(34.8423730342718,-14.6505019462243,0.63557304487636));
#35918=CARTESIAN_POINT('Ctrl Pts',(34.9137340335215,-14.4963699338552,-1.86858636173319));
#35919=CARTESIAN_POINT('Ctrl Pts',(35.2957699604174,-14.5381447126848,-3.71029995872548));
#35920=CARTESIAN_POINT('Ctrl Pts',(36.704915652626,-14.9006586663418,-7.16936247490966));
#35921=CARTESIAN_POINT('Ctrl Pts',(37.7093165664698,-15.2257990211601,-8.73699595768435));
#35922=CARTESIAN_POINT('Ctrl Pts',(40.2121512288891,-16.0925451480995,-11.3730256982353));
#35923=CARTESIAN_POINT('Ctrl Pts',(41.6875985735119,-16.6328052292317,-12.4235805191845));
#35924=CARTESIAN_POINT('Ctrl Pts',(44.9414037540397,-17.8377468920231,-13.8529470821977));
#35925=CARTESIAN_POINT('Ctrl Pts',(46.6732919100491,-18.4952436947556,-14.2204718556833));
#35926=CARTESIAN_POINT('Ctrl Pts',(48.4187086763093,-19.1537534053196,-14.2198708430666));
#35927=CARTESIAN_POINT('Ctrl Pts',(33.9925722540018,-15.1415840475455,1.6296462177106));
#35928=CARTESIAN_POINT('Ctrl Pts',(33.9881310914301,-15.0955481153421,1.1894703117361));
#35929=CARTESIAN_POINT('Ctrl Pts',(33.9726251531405,-15.0387526938512,0.66424400299639));
#35930=CARTESIAN_POINT('Ctrl Pts',(34.0436978384923,-14.8839745452648,-1.95287905122465));
#35931=CARTESIAN_POINT('Ctrl Pts',(34.4404940723683,-14.9333078251896,-3.87337387080411));
#35932=CARTESIAN_POINT('Ctrl Pts',(35.907526600646,-15.3212948554071,-7.48792130212165));
#35933=CARTESIAN_POINT('Ctrl Pts',(36.9538988571648,-15.6662361881476,-9.12360836229528));
#35934=CARTESIAN_POINT('Ctrl Pts',(39.5635848921121,-16.5814962694294,-11.8774049927359));
#35935=CARTESIAN_POINT('Ctrl Pts',(41.1012880289339,-17.150820909756,-12.9732563608631));
#35936=CARTESIAN_POINT('Ctrl Pts',(44.496204451925,-18.4192429936996,-14.4676858045717));
#35937=CARTESIAN_POINT('Ctrl Pts',(46.3001798643446,-19.1104364369604,-14.8501851005199));
#35938=CARTESIAN_POINT('Ctrl Pts',(48.1219785107275,-19.8034868749643,-14.8499483202528));
#35939=CARTESIAN_POINT('Ctrl Pts',(33.5971163401329,-16.0080796379932,1.62975540065039));
#35940=CARTESIAN_POINT('Ctrl Pts',(33.5926757814804,-15.9620499659334,1.18963935153781));
#35941=CARTESIAN_POINT('Ctrl Pts',(33.5771179639697,-15.905224906648,0.664246445067017));
#35942=CARTESIAN_POINT('Ctrl Pts',(33.6475470722393,-15.7501528462821,-1.9528862309185));
#35943=CARTESIAN_POINT('Ctrl Pts',(34.0453300100182,-15.7999367857058,-3.8731703451939));
#35944=CARTESIAN_POINT('Ctrl Pts',(35.5112613559415,-16.1874208227894,-7.4882333580361));
#35945=CARTESIAN_POINT('Ctrl Pts',(36.5583090926487,-16.5326707000397,-9.12349227710467));
#35946=CARTESIAN_POINT('Ctrl Pts',(39.1677510875134,-17.44781930872,-11.8775764776647));
#35947=CARTESIAN_POINT('Ctrl Pts',(40.705853858616,-18.0173264966996,-12.9726927515386));
#35948=CARTESIAN_POINT('Ctrl Pts',(44.1003244488303,-19.2855449177437,-14.4683433354976));
#35949=CARTESIAN_POINT('Ctrl Pts',(45.9046009234659,-19.9768684693553,-14.8498038985148));
#35950=CARTESIAN_POINT('Ctrl Pts',(47.7263079790886,-20.6698844856028,-14.8500516281495));
#35951=CARTESIAN_POINT('Ctrl Pts',(33.8728645130295,-16.9191631550063,1.59674373345245));
#35952=CARTESIAN_POINT('Ctrl Pts',(33.8683874970823,-16.8727555761308,1.15301430092323));
#35953=CARTESIAN_POINT('Ctrl Pts',(33.8536050613457,-16.8166824782156,0.635579150052946));
#35954=CARTESIAN_POINT('Ctrl Pts',(33.9233571178867,-16.6618156864003,-1.86860431096782));
#35955=CARTESIAN_POINT('Ctrl Pts',(34.3078598045374,-16.7047171139728,-3.70979114470055));
#35956=CARTESIAN_POINT('Ctrl Pts',(35.7142525408696,-17.0659735847998,-7.17014261469517));
#35957=CARTESIAN_POINT('Ctrl Pts',(36.7203421551699,-17.3918853008964,-8.7367057447198));
#35958=CARTESIAN_POINT('Ctrl Pts',(39.2225667174021,-18.2583527463199,-11.3734544105454));
#35959=CARTESIAN_POINT('Ctrl Pts',(40.6990131477269,-18.7990691965894,-12.4221714958709));
#35960=CARTESIAN_POINT('Ctrl Pts',(43.9517037462933,-20.0035017021346,-13.8545909095149));
#35961=CARTESIAN_POINT('Ctrl Pts',(45.6843449310537,-20.6613231478665,-14.2195188099675));
#35962=CARTESIAN_POINT('Ctrl Pts',(47.4295323472119,-21.3197474319158,-14.2201291128084));
#35963=CARTESIAN_POINT('Ctrl Pts',(34.8604849513721,-14.6113821712787,0.));
#35964=CARTESIAN_POINT('Ctrl Pts',(34.9137340335215,-14.4963699338552,-1.86858636173319));
#35965=CARTESIAN_POINT('Ctrl Pts',(35.2957699604174,-14.5381447126848,-3.71029995872548));
#35966=CARTESIAN_POINT('Ctrl Pts',(36.704915652626,-14.9006586663418,-7.16936247490966));
#35967=CARTESIAN_POINT('Ctrl Pts',(37.7093165664698,-15.2257990211577,-8.73699595768434));
#35968=CARTESIAN_POINT('Ctrl Pts',(39.0880341222367,-15.7032568890521,-10.1890856763509));
#35969=CARTESIAN_POINT('Ctrl Pts',(39.2176525965017,-15.7484477541922,-10.3203928635178));
#35970=CARTESIAN_POINT('Ctrl Pts',(39.3495129251698,-15.7946976519001,-10.4488603766002));
#35971=CARTESIAN_POINT('Ctrl Pts',(33.871308617615,-16.7773762111447,8.88178419700125E-16));
#35972=CARTESIAN_POINT('Ctrl Pts',(33.9233571178867,-16.6618156864003,-1.86860431096782));
#35973=CARTESIAN_POINT('Ctrl Pts',(34.3078598045374,-16.7047171139728,-3.70979114470055));
#35974=CARTESIAN_POINT('Ctrl Pts',(35.7142525408696,-17.0659735847998,-7.17014261469517));
#35975=CARTESIAN_POINT('Ctrl Pts',(36.7203421551699,-17.3918853008964,-8.7367057447198));
#35976=CARTESIAN_POINT('Ctrl Pts',(38.1057592455497,-17.8716259385938,-10.1966053555733));
#35977=CARTESIAN_POINT('Ctrl Pts',(38.2426607296422,-17.919371448325,-10.3350231942302));
#35978=CARTESIAN_POINT('Ctrl Pts',(38.3820655716557,-17.9682986698104,-10.4702558451034));
#35979=CARTESIAN_POINT('Ctrl Pts',(41.8409566234846,-15.4546943255726,1.24689092472231));
#35980=CARTESIAN_POINT('Ctrl Pts',(41.8360870570327,-15.4042176704004,0.764254723794704));
#35981=CARTESIAN_POINT('Ctrl Pts',(41.8301526811214,-15.3564609751279,0.332948693687485));
#35982=CARTESIAN_POINT('Ctrl Pts',(41.9009886759631,-15.2075196935603,-0.978870002742722));
#35983=CARTESIAN_POINT('Ctrl Pts',(42.1326921492877,-15.1720089789358,-1.98783577092476));
#35984=CARTESIAN_POINT('Ctrl Pts',(42.924704614198,-15.2628516088035,-3.80852727279997));
#35985=CARTESIAN_POINT('Ctrl Pts',(43.4898198932461,-15.3806923683367,-4.65544360723683));
#35986=CARTESIAN_POINT('Ctrl Pts',(44.8634258749406,-15.7347286943442,-6.04997283341622));
#35987=CARTESIAN_POINT('Ctrl Pts',(45.6839445214076,-15.9692083429551,-6.61832169890477));
#35988=CARTESIAN_POINT('Ctrl Pts',(47.4457702195574,-16.5029496832246,-7.3676840309116));
#35989=CARTESIAN_POINT('Ctrl Pts',(48.4183716585838,-16.8055334255027,-7.57138648687994));
#35990=CARTESIAN_POINT('Ctrl Pts',(49.3570623388651,-17.0992034029534,-7.5696258196942));
#35991=CARTESIAN_POINT('Ctrl Pts',(39.4829021650676,-15.6825261124559,1.35489330510234));
#35992=CARTESIAN_POINT('Ctrl Pts',(39.4781536574544,-15.6333043216819,0.884255581223509));
#35993=CARTESIAN_POINT('Ctrl Pts',(39.4695005333267,-15.5829872885748,0.426396977904085));
#35994=CARTESIAN_POINT('Ctrl Pts',(39.5401684750088,-15.4322923841402,-1.25360819502788));
#35995=CARTESIAN_POINT('Ctrl Pts',(39.8187991367757,-15.420877767565,-2.51960912782495));
#35996=CARTESIAN_POINT('Ctrl Pts',(40.8008105435898,-15.595351432329,-4.84647586779572));
#35997=CARTESIAN_POINT('Ctrl Pts',(41.5019188729783,-15.7773622894765,-5.91572199046869));
#35998=CARTESIAN_POINT('Ctrl Pts',(43.2240929050328,-16.2896605076506,-7.69376028691819));
#35999=CARTESIAN_POINT('Ctrl Pts',(44.2470512648663,-16.618655401243,-8.41063186548494));
#36000=CARTESIAN_POINT('Ctrl Pts',(46.4693548995031,-17.3595514471479,-9.37059840628112));
#36001=CARTESIAN_POINT('Ctrl Pts',(47.6765808868325,-17.7717772858459,-9.62435378629451));
#36002=CARTESIAN_POINT('Ctrl Pts',(48.8643218056536,-18.1781059077972,-9.62320046360535));
#36003=CARTESIAN_POINT('Ctrl Pts',(37.126228656985,-15.4455672457341,1.47293201877976));
#36004=CARTESIAN_POINT('Ctrl Pts',(37.121612187704,-15.3977141299041,1.01538097970151));
#36005=CARTESIAN_POINT('Ctrl Pts',(37.1100152319929,-15.3446140089033,0.528580753658652));
#36006=CARTESIAN_POINT('Ctrl Pts',(37.1808604460319,-15.1921664085262,-1.55402875456015));
#36007=CARTESIAN_POINT('Ctrl Pts',(37.5102521839154,-15.2068479190487,-3.10121432125934));
#36008=CARTESIAN_POINT('Ctrl Pts',(38.7006440566771,-15.4730537974356,-5.9812914544847));
#36009=CARTESIAN_POINT('Ctrl Pts',(39.5500810470697,-15.725061187495,-7.29389406575031));
#36010=CARTESIAN_POINT('Ctrl Pts',(41.6535490821772,-16.4104803826146,-9.4911359380562));
#36011=CARTESIAN_POINT('Ctrl Pts',(42.8976498813582,-16.8427247306038,-10.3708286016645));
#36012=CARTESIAN_POINT('Ctrl Pts',(45.6237335200129,-17.8102574730359,-11.5604045561775));
#36013=CARTESIAN_POINT('Ctrl Pts',(47.0873378224419,-18.3423260668147,-11.8694761541617));
#36014=CARTESIAN_POINT('Ctrl Pts',(48.5474784324869,-18.8718427994042,-11.8687142284811));
#36015=CARTESIAN_POINT('Ctrl Pts',(34.8615042977018,-14.7529241788872,1.596470776103));
#36016=CARTESIAN_POINT('Ctrl Pts',(34.8570257719499,-14.7065009496497,1.15259170141934));
#36017=CARTESIAN_POINT('Ctrl Pts',(34.8423730342718,-14.6505019462243,0.63557304487636));
#36018=CARTESIAN_POINT('Ctrl Pts',(34.9137340335215,-14.4963699338552,-1.86858636173319));
#36019=CARTESIAN_POINT('Ctrl Pts',(35.2957699604174,-14.5381447126848,-3.71029995872548));
#36020=CARTESIAN_POINT('Ctrl Pts',(36.704915652626,-14.9006586663418,-7.16936247490966));
#36021=CARTESIAN_POINT('Ctrl Pts',(37.7093165664698,-15.2257990211577,-8.73699595768434));
#36022=CARTESIAN_POINT('Ctrl Pts',(40.2121512288891,-16.0925451481019,-11.3730256982353));
#36023=CARTESIAN_POINT('Ctrl Pts',(41.6875985735119,-16.6328052292293,-12.4235805191845));
#36024=CARTESIAN_POINT('Ctrl Pts',(44.9414037540397,-17.8377468920255,-13.8529470821977));
#36025=CARTESIAN_POINT('Ctrl Pts',(46.6732919100429,-18.4952436947699,-14.2204718556833));
#36026=CARTESIAN_POINT('Ctrl Pts',(48.4187086763093,-19.1537534053196,-14.2198708430666));
#36027=CARTESIAN_POINT('Ctrl Pts',(33.8728645130295,-16.9191631550063,1.59674373345245));
#36028=CARTESIAN_POINT('Ctrl Pts',(33.8683874970823,-16.8727555761308,1.15301430092323));
#36029=CARTESIAN_POINT('Ctrl Pts',(33.8536050613457,-16.8166824782156,0.635579150052946));
#36030=CARTESIAN_POINT('Ctrl Pts',(33.9233571178867,-16.6618156864003,-1.86860431096782));
#36031=CARTESIAN_POINT('Ctrl Pts',(34.3078598045374,-16.7047171139705,-3.70979114470055));
#36032=CARTESIAN_POINT('Ctrl Pts',(35.7142525408696,-17.0659735848022,-7.17014261469517));
#36033=CARTESIAN_POINT('Ctrl Pts',(36.7203421551699,-17.391885300894,-8.7367057447174));
#36034=CARTESIAN_POINT('Ctrl Pts',(39.2225667174021,-18.2583527463223,-11.3734544105478));
#36035=CARTESIAN_POINT('Ctrl Pts',(40.6990131477221,-18.7990691965894,-12.4221714958709));
#36036=CARTESIAN_POINT('Ctrl Pts',(43.9517037462981,-20.0035017021346,-13.8545909095149));
#36037=CARTESIAN_POINT('Ctrl Pts',(45.684344931045,-20.66132314788,-14.2195188099485));
#36038=CARTESIAN_POINT('Ctrl Pts',(47.4295323472119,-21.3197474319158,-14.2201291128084));
#36039=CARTESIAN_POINT('Ctrl Pts',(35.8800194678368,-18.1761744494744,1.47327608945384));
#36040=CARTESIAN_POINT('Ctrl Pts',(35.8754049017066,-18.1283410613852,1.01591367866102));
#36041=CARTESIAN_POINT('Ctrl Pts',(35.863644457821,-18.0751475421218,0.528588449411221));
#36042=CARTESIAN_POINT('Ctrl Pts',(35.9324615528156,-17.9217737308913,-1.5540513800922));
#36043=CARTESIAN_POINT('Ctrl Pts',(36.2649627130594,-17.9378754149084,-3.10057294639211));
#36044=CARTESIAN_POINT('Ctrl Pts',(37.4518844049313,-18.2024961996302,-5.98227484336081));
#36045=CARTESIAN_POINT('Ctrl Pts',(38.3034500513313,-18.4554759130049,-7.29352824386674));
#36046=CARTESIAN_POINT('Ctrl Pts',(40.4061490374134,-19.140543821974,-9.49167634239111));
#36047=CARTESIAN_POINT('Ctrl Pts',(41.6515092131697,-19.5733634365314,-10.3690524868117));
#36048=CARTESIAN_POINT('Ctrl Pts',(44.3761878888565,-20.5402543714441,-11.5624766483028));
#36049=CARTESIAN_POINT('Ctrl Pts',(45.840743551652,-21.0727284454479,-11.8682745705403));
#36050=CARTESIAN_POINT('Ctrl Pts',(47.3005929134931,-21.60214123715,-11.8690397849988));
#36051=CARTESIAN_POINT('Ctrl Pts',(37.6031879890149,-19.8012255369167,1.35541228259766));
#36052=CARTESIAN_POINT('Ctrl Pts',(37.5984423520111,-19.7520335023888,0.885059075368103));
#36053=CARTESIAN_POINT('Ctrl Pts',(37.5895426312094,-19.7015755924258,0.42640858575879));
#36054=CARTESIAN_POINT('Ctrl Pts',(37.6571514684129,-19.5494836419063,-1.25364232215011));
#36055=CARTESIAN_POINT('Ctrl Pts',(37.9404722137893,-19.5402111378009,-2.51864171285047));
#36056=CARTESIAN_POINT('Ctrl Pts',(38.917249388435,-19.7122939334798,-4.84795915810355));
#36057=CARTESIAN_POINT('Ctrl Pts',(39.6215684668002,-19.8957713902408,-5.91517020463238));
#36058=CARTESIAN_POINT('Ctrl Pts',(41.3425825071256,-20.4075397474874,-7.69457540343085));
#36059=CARTESIAN_POINT('Ctrl Pts',(42.3674404420954,-20.7374023418912,-8.40795287042136));
#36060=CARTESIAN_POINT('Ctrl Pts',(44.5876249070044,-21.4773303202308,-9.37372383736816));
#36061=CARTESIAN_POINT('Ctrl Pts',(45.7962902185093,-21.8901596096101,-9.62254085998721));
#36062=CARTESIAN_POINT('Ctrl Pts',(46.9835874904385,-22.2963396064216,-9.62369151535389));
#36063=CARTESIAN_POINT('Ctrl Pts',(38.9761478068775,-21.7318648520661,1.24768188077466));
#36064=CARTESIAN_POINT('Ctrl Pts',(38.9712826154239,-21.681433547381,0.765479302051883));
#36065=CARTESIAN_POINT('Ctrl Pts',(38.9649724098635,-21.6334621464569,0.332966384826352));
#36066=CARTESIAN_POINT('Ctrl Pts',(39.0311461269946,-21.4823916741919,-0.978922014735768));
#36067=CARTESIAN_POINT('Ctrl Pts',(39.269997598184,-21.450145680751,-1.98636136647091));
#36068=CARTESIAN_POINT('Ctrl Pts',(40.0540327468074,-21.5373444678863,-3.81078790540598));
#36069=CARTESIAN_POINT('Ctrl Pts',(40.6240414198136,-21.6574204222982,-4.65460264909513));
#36070=CARTESIAN_POINT('Ctrl Pts',(41.9958794973451,-22.0106492051883,-6.05121512493769));
#36071=CARTESIAN_POINT('Ctrl Pts',(42.8192932220523,-22.2464512872586,-6.61423873311251));
#36072=CARTESIAN_POINT('Ctrl Pts',(44.5778891652563,-22.7787172284945,-7.3724473947518));
#36073=CARTESIAN_POINT('Ctrl Pts',(45.5526929856258,-23.0822022983042,-7.56862230172406));
#36074=CARTESIAN_POINT('Ctrl Pts',(46.4906987626547,-23.3756641324473,-7.57037421506012));
#36075=CARTESIAN_POINT('Ctrl Pts',(31.1202396243796,-21.5675617135473,1.59674381934713));
#36076=CARTESIAN_POINT('Ctrl Pts',(31.1224126652406,-21.5209893482701,1.15301435964445));
#36077=CARTESIAN_POINT('Ctrl Pts',(31.1157607260978,-21.4633832297129,0.635579189033741));
#36078=CARTESIAN_POINT('Ctrl Pts',(31.2068426510981,-21.320019509083,-1.86860431096819));
#36079=CARTESIAN_POINT('Ctrl Pts',(31.5813261451123,-21.4172046995034,-3.70979114473245));
#36080=CARTESIAN_POINT('Ctrl Pts',(32.9219916749941,-21.9749346552614,-7.17014261466314));
#36081=CARTESIAN_POINT('Ctrl Pts',(33.8714586745532,-22.4407105406785,-8.73670574474145));
#36082=CARTESIAN_POINT('Ctrl Pts',(36.2249030242345,-23.6544622808189,-11.3734544105236));
#36083=CARTESIAN_POINT('Ctrl Pts',(37.6093693845368,-24.399795252403,-12.4221714958129));
#36084=CARTESIAN_POINT('Ctrl Pts',(40.6575436657172,-26.0548745077493,-13.8545909095728));
#36085=CARTESIAN_POINT('Ctrl Pts',(42.2789313088874,-26.9525808296639,-14.2195188100293));
#36086=CARTESIAN_POINT('Ctrl Pts',(43.9126516878551,-27.8526693689673,-14.2201291128084));
#36087=CARTESIAN_POINT('Ctrl Pts',(32.9280732767456,-23.097426378281,1.47327617534843));
#36088=CARTESIAN_POINT('Ctrl Pts',(32.9303130813041,-23.0494231409482,1.01591373652235));
#36089=CARTESIAN_POINT('Ctrl Pts',(32.9262425677183,-22.9950973654526,0.528588481831309));
#36090=CARTESIAN_POINT('Ctrl Pts',(33.0161865744695,-22.8530783700746,-1.55405138009592));
#36091=CARTESIAN_POINT('Ctrl Pts',(33.3430118437574,-22.91633601094,-3.1005729464167));
#36092=CARTESIAN_POINT('Ctrl Pts',(34.4801929200289,-23.3471799062887,-5.98227484333611));
#36093=CARTESIAN_POINT('Ctrl Pts',(35.2870880890083,-23.718775078158,-7.29352824389314));
#36094=CARTESIAN_POINT('Ctrl Pts',(37.2708893025803,-24.6961152497729,-9.49167634236457));
#36095=CARTESIAN_POINT('Ctrl Pts',(38.441976853954,-25.3017626168073,-10.3690524867346));
#36096=CARTESIAN_POINT('Ctrl Pts',(41.0013193023712,-26.6465742010416,-11.5624766483798));
#36097=CARTESIAN_POINT('Ctrl Pts',(42.3751889385695,-27.3820564590436,-11.8682745706496));
#36098=CARTESIAN_POINT('Ctrl Pts',(43.7448358429351,-28.1138388177857,-11.8690397849987));
#36099=CARTESIAN_POINT('Ctrl Pts',(34.4024335442869,-24.9511692381922,1.35541236849217));
#36100=CARTESIAN_POINT('Ctrl Pts',(34.4047369676381,-24.9018025300741,0.885059132411614));
#36101=CARTESIAN_POINT('Ctrl Pts',(34.4031087413041,-24.8505916427402,0.426408611912723));
#36102=CARTESIAN_POINT('Ctrl Pts',(34.49167436083,-24.7096695075246,-1.25364232215568));
#36103=CARTESIAN_POINT('Ctrl Pts',(34.7734309243662,-24.7408121301906,-2.51864171287734));
#36104=CARTESIAN_POINT('Ctrl Pts',(35.7157759805903,-25.0501532567769,-4.8479591580766));
#36105=CARTESIAN_POINT('Ctrl Pts',(36.3868145416534,-25.331998233306,-5.91517020466113));
#36106=CARTESIAN_POINT('Ctrl Pts',(38.0174789095799,-26.0834833614041,-7.69457540340194));
#36107=CARTESIAN_POINT('Ctrl Pts',(38.9849609267772,-26.5558409214644,-8.40795287029638));
#36108=CARTESIAN_POINT('Ctrl Pts',(41.0772443843597,-27.6042026929754,-9.37372383749305));
#36109=CARTESIAN_POINT('Ctrl Pts',(42.2148554922723,-28.1848409838253,-9.62254086017268));
#36110=CARTESIAN_POINT('Ctrl Pts',(43.3322623493507,-28.7558566730956,-9.62369151535378));
#36111=CARTESIAN_POINT('Ctrl Pts',(35.4866599889488,-27.0575499833002,1.2476819666691));
#36112=CARTESIAN_POINT('Ctrl Pts',(35.4890214412832,-27.0069396045641,0.7654793583525));
#36113=CARTESIAN_POINT('Ctrl Pts',(35.4896025055219,-26.9585584437039,0.33296640524947));
#36114=CARTESIAN_POINT('Ctrl Pts',(35.5766022409729,-26.8184431506615,-0.978922014741607));
#36115=CARTESIAN_POINT('Ctrl Pts',(35.8176116317321,-26.820517483472,-1.98636136650726));
#36116=CARTESIAN_POINT('Ctrl Pts',(36.5812567518767,-27.0184085480271,-3.81078790536956));
#36117=CARTESIAN_POINT('Ctrl Pts',(37.1283749683431,-27.2183829945029,-4.65460264913816));
#36118=CARTESIAN_POINT('Ctrl Pts',(38.4359800152256,-27.7632493318097,-6.05121512489442));
#36119=CARTESIAN_POINT('Ctrl Pts',(39.2174544404224,-28.1138352796404,-6.61423873291563));
#36120=CARTESIAN_POINT('Ctrl Pts',(40.8824010709675,-28.8909578185449,-7.37244739494853));
#36121=CARTESIAN_POINT('Ctrl Pts',(41.8040923654846,-29.3300828960655,-7.56862230196192));
#36122=CARTESIAN_POINT('Ctrl Pts',(42.6907866227632,-29.7540498521225,-7.57037421505996));
#36123=CARTESIAN_POINT('Ctrl Pts',(31.1388779521426,-21.4269965203145,7.38298311375729E-15));
#36124=CARTESIAN_POINT('Ctrl Pts',(31.2068426510981,-21.320019509083,-1.86860431096819));
#36125=CARTESIAN_POINT('Ctrl Pts',(31.5813261451123,-21.4172046995034,-3.70979114473245));
#36126=CARTESIAN_POINT('Ctrl Pts',(32.9219916749941,-21.9749346552614,-7.17014261466314));
#36127=CARTESIAN_POINT('Ctrl Pts',(33.8714586745532,-22.4407105406785,-8.73670574474145));
#36128=CARTESIAN_POINT('Ctrl Pts',(35.1745000052642,-23.1127335196113,-10.1966053555721));
#36129=CARTESIAN_POINT('Ctrl Pts',(35.3032131351466,-23.1794761614708,-10.3350231942276));
#36130=CARTESIAN_POINT('Ctrl Pts',(35.4342359672587,-23.2477447519414,-10.4702558450994));
#36131=CARTESIAN_POINT('Ctrl Pts',(39.2156436908074,-21.2519768052529,1.24689101061683));
#36132=CARTESIAN_POINT('Ctrl Pts',(39.218007266706,-21.2013209149703,0.764254780031375));
#36133=CARTESIAN_POINT('Ctrl Pts',(39.2189297793915,-21.1532057605279,0.332948714116346));
#36134=CARTESIAN_POINT('Ctrl Pts',(39.310241321719,-21.0158614973052,-0.978870002768584));
#36135=CARTESIAN_POINT('Ctrl Pts',(39.544640089421,-21.0136870730577,-1.98783577086775));
#36136=CARTESIAN_POINT('Ctrl Pts',(40.3156627552369,-21.2163201816855,-3.8085272728572));
#36137=CARTESIAN_POINT('Ctrl Pts',(40.8582554869254,-21.4133857818212,-4.65544360719877));
#36138=CARTESIAN_POINT('Ctrl Pts',(42.1674955178609,-21.9593030415928,-6.04997283345453));
#36139=CARTESIAN_POINT('Ctrl Pts',(42.9462925343071,-22.3081680037623,-6.61832169907729));
#36140=CARTESIAN_POINT('Ctrl Pts',(44.6142260746746,-23.0872105664939,-7.36768403073927));
#36141=CARTESIAN_POINT('Ctrl Pts',(45.5338656769265,-23.5251300590179,-7.57138648664217));
#36142=CARTESIAN_POINT('Ctrl Pts',(46.4212082443693,-23.9494005117266,-7.56962581969437));
#36143=CARTESIAN_POINT('Ctrl Pts',(36.8491669828394,-21.1419034541631,1.3548933909969));
#36144=CARTESIAN_POINT('Ctrl Pts',(36.8514717995482,-21.0925068841199,0.884255638225286));
#36145=CARTESIAN_POINT('Ctrl Pts',(36.8500676110209,-21.0414705341014,0.426397004061771));
#36146=CARTESIAN_POINT('Ctrl Pts',(36.9414623772721,-20.9023665809611,-1.25360819504659));
#36147=CARTESIAN_POINT('Ctrl Pts',(37.2188814500116,-20.9307214263664,-2.51960912779197));
#36148=CARTESIAN_POINT('Ctrl Pts',(38.1660672052557,-21.2431739952986,-4.8464758678288));
#36149=CARTESIAN_POINT('Ctrl Pts',(38.8341364170723,-21.5231103628947,-5.91572199044975));
#36150=CARTESIAN_POINT('Ctrl Pts',(40.4658735625806,-22.2752850427144,-7.69376028693729));
#36151=CARTESIAN_POINT('Ctrl Pts',(41.4315988261968,-22.7465133961258,-8.41063186560463));
#36152=CARTESIAN_POINT('Ctrl Pts',(43.5258421132307,-23.7961349710929,-9.37059840616155));
#36153=CARTESIAN_POINT('Ctrl Pts',(44.6621144270249,-24.3759711162289,-9.62435378612333));
#36154=CARTESIAN_POINT('Ctrl Pts',(45.7799392638232,-24.9471970554255,-9.62320046360547));
#36155=CARTESIAN_POINT('Ctrl Pts',(34.5502037758215,-20.5719668778725,1.47293210467438));
#36156=CARTESIAN_POINT('Ctrl Pts',(34.5524445041376,-20.5239438427437,1.01538103753427));
#36157=CARTESIAN_POINT('Ctrl Pts',(34.5485225226992,-20.4697337816493,0.528580786081231));
#36158=CARTESIAN_POINT('Ctrl Pts',(34.6403421915648,-20.3289202010265,-1.55402875457259));
#36159=CARTESIAN_POINT('Ctrl Pts',(34.964291799767,-20.3903296068349,-3.10121432124684));
#36160=CARTESIAN_POINT('Ctrl Pts',(36.1046821531125,-20.823236320083,-5.98129145449724));
#36161=CARTESIAN_POINT('Ctrl Pts',(36.9096087087966,-21.1935661261718,-7.29389406574334));
#36162=CARTESIAN_POINT('Ctrl Pts',(38.8941211503257,-22.1713634554262,-9.49113593806328));
#36163=CARTESIAN_POINT('Ctrl Pts',(40.0640440126768,-22.7762621832688,-10.3708286017458));
#36164=CARTESIAN_POINT('Ctrl Pts',(42.6246857849651,-24.1219089895058,-11.5604045560964));
#36165=CARTESIAN_POINT('Ctrl Pts',(43.9976714500081,-24.8568545017212,-11.8694761540667));
#36166=CARTESIAN_POINT('Ctrl Pts',(45.3675918458115,-25.5887811923518,-11.8687142284812));
#36167=CARTESIAN_POINT('Ctrl Pts',(32.4071044310923,-19.5640700378125,1.59647086199769));
#36168=CARTESIAN_POINT('Ctrl Pts',(32.4092782047888,-19.5174819665916,1.15259176011853));
#36169=CARTESIAN_POINT('Ctrl Pts',(32.402744098825,-19.4599676463163,0.635573083859125));
#36170=CARTESIAN_POINT('Ctrl Pts',(32.4953140197357,-19.3175602025281,-1.86858636174048));
#36171=CARTESIAN_POINT('Ctrl Pts',(32.8675162009725,-19.4132791553963,-3.71029995872507));
#36172=CARTESIAN_POINT('Ctrl Pts',(34.2107277071003,-19.9726455810671,-7.16936247491005));
#36173=CARTESIAN_POINT('Ctrl Pts',(35.1586329709169,-20.4374176294354,-8.73699595768695));
#36174=CARTESIAN_POINT('Ctrl Pts',(37.5126415503284,-21.6515320408183,-11.3730256982328));
#36175=CARTESIAN_POINT('Ctrl Pts',(38.8961839422332,-22.3962711036893,-12.4235805192561));
#36176=CARTESIAN_POINT('Ctrl Pts',(41.9453890000031,-24.0520129554246,-13.8529470821262));
#36177=CARTESIAN_POINT('Ctrl Pts',(43.5660774805969,-24.9492907715107,-14.220471855612));
#36178=CARTESIAN_POINT('Ctrl Pts',(45.2000127177927,-25.8494965077557,-14.2198708430667));
#36179=CARTESIAN_POINT('Ctrl Pts',(32.426238988581,-19.4238236466313,0.));
#36180=CARTESIAN_POINT('Ctrl Pts',(32.4953140197357,-19.3175602025281,-1.86858636174048));
#36181=CARTESIAN_POINT('Ctrl Pts',(32.8675162009725,-19.4132791553963,-3.71029995872507));
#36182=CARTESIAN_POINT('Ctrl Pts',(34.2107277071003,-19.9726455810671,-7.16936247491005));
#36183=CARTESIAN_POINT('Ctrl Pts',(35.1586329709169,-20.4374176294354,-8.73699595768695));
#36184=CARTESIAN_POINT('Ctrl Pts',(36.4553678306315,-21.1062276306783,-10.1890856763509));
#36185=CARTESIAN_POINT('Ctrl Pts',(36.5772356450557,-21.1694051501777,-10.3203928635186));
#36186=CARTESIAN_POINT('Ctrl Pts',(36.7011717789887,-21.233949971968,-10.4488603766022));
#36187=CARTESIAN_POINT('Ctrl Pts',(32.4071044310923,-19.5640700378125,1.59647086199769));
#36188=CARTESIAN_POINT('Ctrl Pts',(32.4092782047888,-19.5174819665916,1.15259176011853));
#36189=CARTESIAN_POINT('Ctrl Pts',(32.402744098825,-19.4599676463163,0.635573083859125));
#36190=CARTESIAN_POINT('Ctrl Pts',(32.4953140197357,-19.3175602025281,-1.86858636174048));
#36191=CARTESIAN_POINT('Ctrl Pts',(32.8675162009725,-19.4132791553963,-3.71029995872507));
#36192=CARTESIAN_POINT('Ctrl Pts',(34.2107277071003,-19.9726455810671,-7.16936247491005));
#36193=CARTESIAN_POINT('Ctrl Pts',(35.1586329709169,-20.4374176294354,-8.73699595768695));
#36194=CARTESIAN_POINT('Ctrl Pts',(37.5126415503284,-21.6515320408183,-11.3730256982328));
#36195=CARTESIAN_POINT('Ctrl Pts',(38.8961839422332,-22.3962711036893,-12.4235805192561));
#36196=CARTESIAN_POINT('Ctrl Pts',(41.9453890000031,-24.0520129554246,-13.8529470821262));
#36197=CARTESIAN_POINT('Ctrl Pts',(43.5660774805969,-24.9492907715107,-14.220471855612));
#36198=CARTESIAN_POINT('Ctrl Pts',(45.2000127177927,-25.8494965077557,-14.2198708430667));
#36199=CARTESIAN_POINT('Ctrl Pts',(31.4917047963492,-19.8251119861396,1.62964630360532));
#36200=CARTESIAN_POINT('Ctrl Pts',(31.4938604348119,-19.77891258719,1.18947037067314));
#36201=CARTESIAN_POINT('Ctrl Pts',(31.4865951546911,-19.7204885321049,0.664244043736472));
#36202=CARTESIAN_POINT('Ctrl Pts',(31.5789716511101,-19.5774004975086,-1.95287905122872));
#36203=CARTESIAN_POINT('Ctrl Pts',(31.9647082138114,-19.6827016274975,-3.87337387081569));
#36204=CARTESIAN_POINT('Ctrl Pts',(33.3615921547095,-20.2755200062714,-7.48792130210999));
#36205=CARTESIAN_POINT('Ctrl Pts',(34.3482235804883,-20.7658646319867,-9.12360836230025));
#36206=CARTESIAN_POINT('Ctrl Pts',(36.8010916839413,-22.0432057314202,-11.8774049927309));
#36207=CARTESIAN_POINT('Ctrl Pts',(38.2421198758116,-22.8255734412205,-12.9732563608963));
#36208=CARTESIAN_POINT('Ctrl Pts',(41.4219656611935,-24.5642317985072,-14.4676858045386));
#36209=CARTESIAN_POINT('Ctrl Pts',(43.1092121219652,-25.5051223581494,-14.8501851005009));
#36210=CARTESIAN_POINT('Ctrl Pts',(44.8138361237937,-26.4503875219921,-14.8499483202528));
#36211=CARTESIAN_POINT('Ctrl Pts',(30.9769588736641,-20.6265086564335,1.62975548654509));
#36212=CARTESIAN_POINT('Ctrl Pts',(30.9791142189907,-20.5803155398586,1.18963941048385));
#36213=CARTESIAN_POINT('Ctrl Pts',(30.9718018055999,-20.5218547654632,0.664246485806314));
#36214=CARTESIAN_POINT('Ctrl Pts',(31.063583103656,-20.3783842201315,-1.9528862309198));
#36215=CARTESIAN_POINT('Ctrl Pts',(31.4502321914759,-20.4842718451404,-3.87317034521865));
#36216=CARTESIAN_POINT('Ctrl Pts',(32.8460977418583,-21.0764356359492,-7.48823335801123));
#36217=CARTESIAN_POINT('Ctrl Pts',(33.8333538619476,-21.5671817964815,-9.12349227712397));
#36218=CARTESIAN_POINT('Ctrl Pts',(36.2859962734989,-22.8443778274229,-11.8775764776454));
#36219=CARTESIAN_POINT('Ctrl Pts',(37.7273940527312,-23.6269831007036,-12.972692751519));
#36220=CARTESIAN_POINT('Ctrl Pts',(40.906827527481,-25.3653764194394,-14.4683433355172));
#36221=CARTESIAN_POINT('Ctrl Pts',(42.5943534697789,-26.3064386087592,-14.8498038985433));
#36222=CARTESIAN_POINT('Ctrl Pts',(44.2988917118187,-27.2516566664768,-14.8500516281495));
#36223=CARTESIAN_POINT('Ctrl Pts',(31.1202396243796,-21.5675617135473,1.59674381934713));
#36224=CARTESIAN_POINT('Ctrl Pts',(31.1224126652406,-21.5209893482701,1.15301435964445));
#36225=CARTESIAN_POINT('Ctrl Pts',(31.1157607260978,-21.4633832297129,0.635579189033741));
#36226=CARTESIAN_POINT('Ctrl Pts',(31.2068426510981,-21.320019509083,-1.86860431096819));
#36227=CARTESIAN_POINT('Ctrl Pts',(31.5813261451123,-21.4172046995034,-3.70979114473125));
#36228=CARTESIAN_POINT('Ctrl Pts',(32.9219916749941,-21.9749346552614,-7.17014261466433));
#36229=CARTESIAN_POINT('Ctrl Pts',(33.8714586745532,-22.4407105406785,-8.73670574474144));
#36230=CARTESIAN_POINT('Ctrl Pts',(36.2249030242345,-23.6544622808189,-11.3734544105236));
#36231=CARTESIAN_POINT('Ctrl Pts',(37.609369384532,-24.399795252403,-12.4221714958081));
#36232=CARTESIAN_POINT('Ctrl Pts',(40.657543665722,-26.0548745077493,-13.8545909095776));
#36233=CARTESIAN_POINT('Ctrl Pts',(42.2789313088846,-26.9525808296624,-14.219518810034));
#36234=CARTESIAN_POINT('Ctrl Pts',(43.9126516878551,-27.8526693689673,-14.2201291128084));
#36235=CARTESIAN_POINT('Ctrl Pts',(29.2929893708795,-23.976947844554,1.59647090706345));
#36236=CARTESIAN_POINT('Ctrl Pts',(29.3017711927835,-23.9311433314999,1.15259179091382));
#36237=CARTESIAN_POINT('Ctrl Pts',(29.3034887354727,-23.8732845217247,0.635573104312268));
#36238=CARTESIAN_POINT('Ctrl Pts',(29.4153831213971,-23.7455006526079,-1.86858636174501));
#36239=CARTESIAN_POINT('Ctrl Pts',(29.7701745937406,-23.8932152178192,-3.71029995871689));
#36240=CARTESIAN_POINT('Ctrl Pts',(31.0201080010755,-24.6380470280742,-7.16936247491829));
#36241=CARTESIAN_POINT('Ctrl Pts',(31.8922209971975,-25.2329893514644,-8.73699595769411));
#36242=CARTESIAN_POINT('Ctrl Pts',(34.0494826673323,-26.7697561790045,-11.3730256982256));
#36243=CARTESIAN_POINT('Ctrl Pts',(35.3129551735408,-27.7038134835938,-12.4235805191652));
#36244=CARTESIAN_POINT('Ctrl Pts',(38.0954870861221,-29.7766493957256,-13.852947082217));
#36245=CARTESIAN_POINT('Ctrl Pts',(39.5719833476435,-30.8954422364371,-14.2204718557213));
#36246=CARTESIAN_POINT('Ctrl Pts',(41.0611748464151,-32.0190184050858,-14.2198708430666));
#36247=CARTESIAN_POINT('Ctrl Pts',(28.3497570418621,-24.1050578112646,1.629646348671));
#36248=CARTESIAN_POINT('Ctrl Pts',(28.3584655992913,-24.0596354334659,1.18947040159126));
#36249=CARTESIAN_POINT('Ctrl Pts',(28.359588878887,-24.000772091729,0.664244065112554));
#36250=CARTESIAN_POINT('Ctrl Pts',(28.4713886672656,-23.872287032033,-1.9528790512343));
#36251=CARTESIAN_POINT('Ctrl Pts',(28.8382130746032,-24.031412384946,-3.87337387079909));
#36252=CARTESIAN_POINT('Ctrl Pts',(30.1365118994152,-24.8169940395271,-7.48792130212669));
#36253=CARTESIAN_POINT('Ctrl Pts',(31.0433175237996,-25.4427599557794,-9.12360836231701));
#36254=CARTESIAN_POINT('Ctrl Pts',(33.2894343746814,-27.0561790920224,-11.8774049927142));
#36255=CARTESIAN_POINT('Ctrl Pts',(34.604452443506,-28.0356631204391,-12.9732563608534));
#36256=CARTESIAN_POINT('Ctrl Pts',(37.5044951003644,-30.2091636817924,-14.4676858045814));
#36257=CARTESIAN_POINT('Ctrl Pts',(39.0406651372098,-31.3805975393655,-14.8501851005436));
#36258=CARTESIAN_POINT('Ctrl Pts',(40.5934132658115,-32.5588345556908,-14.8499483202528));
#36259=CARTESIAN_POINT('Ctrl Pts',(27.726199852942,-24.8250414362348,1.62975553161074));
#36260=CARTESIAN_POINT('Ctrl Pts',(27.7349072261468,-24.7796252351492,1.18963944140568));
#36261=CARTESIAN_POINT('Ctrl Pts',(27.7359890779304,-24.7207188400934,0.664246507182928));
#36262=CARTESIAN_POINT('Ctrl Pts',(27.8472541631358,-24.5917704574944,-1.9528862309267));
#36263=CARTESIAN_POINT('Ctrl Pts',(28.214898340463,-24.7516062016254,-3.87317034519845));
#36264=CARTESIAN_POINT('Ctrl Pts',(29.5122822981076,-25.5363949989265,-7.48823335803153));
#36265=CARTESIAN_POINT('Ctrl Pts',(30.4196491139356,-26.1626472662222,-9.12349227713836));
#36266=CARTESIAN_POINT('Ctrl Pts',(32.6655632155459,-27.7758906912455,-11.877576477631));
#36267=CARTESIAN_POINT('Ctrl Pts',(33.9809133010314,-28.7556624628396,-12.9726927515433));
#36268=CARTESIAN_POINT('Ctrl Pts',(36.8805855629435,-30.9288420054706,-14.4683433354929));
#36269=CARTESIAN_POINT('Ctrl Pts',(38.4170078110994,-32.1004855201288,-14.8498038985624));
#36270=CARTESIAN_POINT('Ctrl Pts',(39.9696777567511,-33.2786637049093,-14.8500516281495));
#36271=CARTESIAN_POINT('Ctrl Pts',(27.7340963985793,-25.7769069069793,1.59674386441279));
#36272=CARTESIAN_POINT('Ctrl Pts',(27.7428752599197,-25.7311178357269,1.1530143904477));
#36273=CARTESIAN_POINT('Ctrl Pts',(27.7444892330823,-25.6731513926385,0.635579209488198));
#36274=CARTESIAN_POINT('Ctrl Pts',(27.8550468610688,-25.544209216253,-1.86860431097603));
#36275=CARTESIAN_POINT('Ctrl Pts',(28.2118877583879,-25.6936997595176,-3.7097911447111));
#36276=CARTESIAN_POINT('Ctrl Pts',(29.4595339978087,-26.4365494265728,-7.17014261468459));
#36277=CARTESIAN_POINT('Ctrl Pts',(30.3330499725326,-27.0327076275655,-8.73670574475586));
#36278=CARTESIAN_POINT('Ctrl Pts',(32.4898047694984,-28.5690351770683,-11.3734544105093));
#36279=CARTESIAN_POINT('Ctrl Pts',(33.7541073173495,-29.5038118395949,-12.4221714958996));
#36280=CARTESIAN_POINT('Ctrl Pts',(36.5357132425746,-31.5758452049212,-13.8545909094863));
#36281=CARTESIAN_POINT('Ctrl Pts',(38.0128405673564,-32.6951616910142,-14.2195188100056));
#36282=CARTESIAN_POINT('Ctrl Pts',(39.5018360737642,-33.8185912781322,-14.2201291128084));
#36283=CARTESIAN_POINT('Ctrl Pts',(29.3318883095338,-23.8408520862203,0.));
#36284=CARTESIAN_POINT('Ctrl Pts',(29.4153831213971,-23.7455006526079,-1.86858636174501));
#36285=CARTESIAN_POINT('Ctrl Pts',(29.7701745937406,-23.8932152178192,-3.71029995871809));
#36286=CARTESIAN_POINT('Ctrl Pts',(31.0201080010755,-24.6380470280742,-7.1693624749171));
#36287=CARTESIAN_POINT('Ctrl Pts',(31.8922209971975,-25.2329893514668,-8.73699595769651));
#36288=CARTESIAN_POINT('Ctrl Pts',(33.0805753785957,-26.0795364430743,-10.1890856763513));
#36289=CARTESIAN_POINT('Ctrl Pts',(33.19221165592,-26.1594145048181,-10.3203928635187));
#36290=CARTESIAN_POINT('Ctrl Pts',(33.3057006128401,-26.240940304242,-10.4488603766015));
#36291=CARTESIAN_POINT('Ctrl Pts',(27.7725495286734,-25.6404249706862,-1.49880108324396E-15));
#36292=CARTESIAN_POINT('Ctrl Pts',(27.8550468610688,-25.544209216253,-1.86860431097603));
#36293=CARTESIAN_POINT('Ctrl Pts',(28.2118877583879,-25.6936997595176,-3.7097911447111));
#36294=CARTESIAN_POINT('Ctrl Pts',(29.4595339978087,-26.4365494265728,-7.17014261468459));
#36295=CARTESIAN_POINT('Ctrl Pts',(30.3330499725326,-27.0327076275655,-8.73670574475586));
#36296=CARTESIAN_POINT('Ctrl Pts',(31.5271893797544,-27.8833324977838,-10.1966053555717));
#36297=CARTESIAN_POINT('Ctrl Pts',(31.6450939272834,-27.9677135840438,-10.3350231942281));
#36298=CARTESIAN_POINT('Ctrl Pts',(31.7650675024754,-28.0539337918559,-10.4702558451017));
#36299=CARTESIAN_POINT('Ctrl Pts',(35.7920133394051,-26.616630318486,1.246891055683));
#36300=CARTESIAN_POINT('Ctrl Pts',(35.8015619426228,-26.566826402425,0.764254809544874));
#36301=CARTESIAN_POINT('Ctrl Pts',(35.8093225655931,-26.519332276069,0.332948724830327));
#36302=CARTESIAN_POINT('Ctrl Pts',(35.9192508155954,-26.3963809659062,-0.978870002769423));
#36303=CARTESIAN_POINT('Ctrl Pts',(36.151573194659,-26.4275870967948,-1.9878357709031));
#36304=CARTESIAN_POINT('Ctrl Pts',(36.8859102633496,-26.7378856585306,-3.8085272728217));
#36305=CARTESIAN_POINT('Ctrl Pts',(37.3949348243792,-27.010164411862,-4.65544360718431));
#36306=CARTESIAN_POINT('Ctrl Pts',(38.6131565530439,-27.7368493043474,-6.04997283346876));
#36307=CARTESIAN_POINT('Ctrl Pts',(39.3343778780771,-28.1929976959362,-6.61832169883747));
#36308=CARTESIAN_POINT('Ctrl Pts',(40.8744649437267,-29.2014824201682,-7.36768403097867));
#36309=CARTESIAN_POINT('Ctrl Pts',(41.7224214992404,-29.7658228850822,-7.57138648693213));
#36310=CARTESIAN_POINT('Ctrl Pts',(42.540352217728,-30.3120568904492,-7.56962581969415));
#36311=CARTESIAN_POINT('Ctrl Pts',(33.4652890233051,-26.1708926054257,1.35489343606293));
#36312=CARTESIAN_POINT('Ctrl Pts',(33.4746002454547,-26.1223268292875,0.884255668135784));
#36313=CARTESIAN_POINT('Ctrl Pts',(33.4804735791513,-26.0716101167854,0.426397017783367));
#36314=CARTESIAN_POINT('Ctrl Pts',(33.5907346359808,-25.9469288717332,-1.25360819504925));
#36315=CARTESIAN_POINT('Ctrl Pts',(33.8612946673231,-26.0144759561311,-2.51960912781043));
#36316=CARTESIAN_POINT('Ctrl Pts',(34.7543728004649,-26.4585467959913,-4.84647586781028));
#36317=CARTESIAN_POINT('Ctrl Pts',(35.3758029321052,-26.8307099768394,-5.91572199044252));
#36318=CARTESIAN_POINT('Ctrl Pts',(36.8838857283485,-27.8074490109362,-7.6937602869444));
#36319=CARTESIAN_POINT('Ctrl Pts',(37.7727185143506,-28.4113179739906,-8.41063186543685));
#36320=CARTESIAN_POINT('Ctrl Pts',(39.6962686996365,-29.7482978092141,-9.37059840632905));
#36321=CARTESIAN_POINT('Ctrl Pts',(40.7384561125427,-30.48394046912,-9.62435378631342));
#36322=CARTESIAN_POINT('Ctrl Pts',(41.7636091770243,-31.2084352127809,-9.62320046360533));
#36323=CARTESIAN_POINT('Ctrl Pts',(31.2708363785842,-25.2795805846981,1.47293214974027));
#36324=CARTESIAN_POINT('Ctrl Pts',(31.2798886902773,-25.2323652421901,1.01538106787782));
#36325=CARTESIAN_POINT('Ctrl Pts',(31.2837215247233,-25.1781488031013,0.528580803091344));
#36326=CARTESIAN_POINT('Ctrl Pts',(31.3946464646597,-25.0518358019871,-1.5540287545765));
#36327=CARTESIAN_POINT('Ctrl Pts',(31.7065592632635,-25.1587229846903,-3.10121432124958));
#36328=CARTESIAN_POINT('Ctrl Pts',(32.7737330382195,-25.7495178004988,-5.98129145449449));
#36329=CARTESIAN_POINT('Ctrl Pts',(33.5177631757263,-26.2306311757317,-7.2938940657433));
#36330=CARTESIAN_POINT('Ctrl Pts',(35.3429210732455,-27.4809015052035,-9.49113593806323));
#36331=CARTESIAN_POINT('Ctrl Pts',(36.4148497432471,-28.2461406190897,-10.3708286016404));
#36332=CARTESIAN_POINT('Ctrl Pts',(38.7579223665916,-29.9425080008996,-11.5604045562015));
#36333=CARTESIAN_POINT('Ctrl Pts',(40.0123393656451,-30.8653690604273,-11.8694761542045));
#36334=CARTESIAN_POINT('Ctrl Pts',(41.2641519184868,-31.7848057921744,-11.8687142284811));
#36335=CARTESIAN_POINT('Ctrl Pts',(29.2929893708795,-23.976947844554,1.59647090706345));
#36336=CARTESIAN_POINT('Ctrl Pts',(29.3017711927835,-23.9311433314999,1.15259179091383));
#36337=CARTESIAN_POINT('Ctrl Pts',(29.3034887354727,-23.8732845217247,0.635573104312268));
#36338=CARTESIAN_POINT('Ctrl Pts',(29.4153831213971,-23.7455006526079,-1.86858636174501));
#36339=CARTESIAN_POINT('Ctrl Pts',(29.7701745937406,-23.8932152178192,-3.71029995871809));
#36340=CARTESIAN_POINT('Ctrl Pts',(31.0201080010755,-24.6380470280742,-7.1693624749171));
#36341=CARTESIAN_POINT('Ctrl Pts',(31.8922209971975,-25.2329893514668,-8.73699595769651));
#36342=CARTESIAN_POINT('Ctrl Pts',(34.0494826673323,-26.7697561790021,-11.3730256982232));
#36343=CARTESIAN_POINT('Ctrl Pts',(35.3129551735408,-27.7038134835914,-12.4235805191652));
#36344=CARTESIAN_POINT('Ctrl Pts',(38.0954870861221,-29.776649395728,-13.852947082217));
#36345=CARTESIAN_POINT('Ctrl Pts',(39.5719833476427,-30.8954422364365,-14.2204718557261));
#36346=CARTESIAN_POINT('Ctrl Pts',(41.0611748464151,-32.0190184050858,-14.2198708430666));
#36347=CARTESIAN_POINT('Ctrl Pts',(27.7340963985793,-25.7769069069793,1.59674386441279));
#36348=CARTESIAN_POINT('Ctrl Pts',(27.7428752599197,-25.7311178357269,1.1530143904477));
#36349=CARTESIAN_POINT('Ctrl Pts',(27.7444892330823,-25.6731513926385,0.635579209488198));
#36350=CARTESIAN_POINT('Ctrl Pts',(27.8550468610688,-25.544209216253,-1.86860431097603));
#36351=CARTESIAN_POINT('Ctrl Pts',(28.2118877583879,-25.6936997595176,-3.7097911447087));
#36352=CARTESIAN_POINT('Ctrl Pts',(29.4595339978087,-26.4365494265727,-7.17014261468699));
#36353=CARTESIAN_POINT('Ctrl Pts',(30.3330499725326,-27.0327076275679,-8.73670574475587));
#36354=CARTESIAN_POINT('Ctrl Pts',(32.4898047694983,-28.5690351770659,-11.3734544105093));
#36355=CARTESIAN_POINT('Ctrl Pts',(33.7541073173447,-29.5038118395925,-12.4221714958948));
#36356=CARTESIAN_POINT('Ctrl Pts',(36.5357132425794,-31.5758452049236,-13.8545909094911));
#36357=CARTESIAN_POINT('Ctrl Pts',(38.0128405673532,-32.6951616910118,-14.2195188099676));
#36358=CARTESIAN_POINT('Ctrl Pts',(39.5018360737642,-33.8185912781322,-14.2201291128085));
#36359=CARTESIAN_POINT('Ctrl Pts',(29.3058064687036,-27.5484813091702,1.47327622041421));
#36360=CARTESIAN_POINT('Ctrl Pts',(29.3148550485227,-27.5012854314998,1.01591376687586));
#36361=CARTESIAN_POINT('Ctrl Pts',(29.318557330567,-27.4469333174927,0.52858849884309));
#36362=CARTESIAN_POINT('Ctrl Pts',(29.4277972482622,-27.3191602363946,-1.554051380104));
#36363=CARTESIAN_POINT('Ctrl Pts',(29.7422934066315,-27.428286091063,-3.10057294640268));
#36364=CARTESIAN_POINT('Ctrl Pts',(30.8065841399312,-28.016582357744,-5.98227484335018));
#36365=CARTESIAN_POINT('Ctrl Pts',(31.5523827727636,-28.4992283820367,-7.2935282438956));
#36366=CARTESIAN_POINT('Ctrl Pts',(33.3769017419044,-29.7489449887834,-9.49167634236224));
#36367=CARTESIAN_POINT('Ctrl Pts',(34.4498767035324,-30.5150908742602,-10.3690524868452));
#36368=CARTESIAN_POINT('Ctrl Pts',(36.7917820928971,-32.2104466224834,-11.5624766482694));
#36369=CARTESIAN_POINT('Ctrl Pts',(38.0469976785191,-33.1339647666031,-11.8682745705784));
#36370=CARTESIAN_POINT('Ctrl Pts',(39.2985600643044,-34.0532197137074,-11.8690397849988));
#36371=CARTESIAN_POINT('Ctrl Pts',(30.5013447592647,-29.5931790826757,1.35541241355805));
#36372=CARTESIAN_POINT('Ctrl Pts',(30.5106503524626,-29.5446426662435,0.885059162337716));
#36373=CARTESIAN_POINT('Ctrl Pts',(30.5163267680096,-29.4937213090679,0.426408625636832));
#36374=CARTESIAN_POINT('Ctrl Pts',(30.6240462289239,-29.3668377587659,-1.25364232216464));
#36375=CARTESIAN_POINT('Ctrl Pts',(30.8985028596502,-29.4377615342222,-2.51864171286706));
#36376=CARTESIAN_POINT('Ctrl Pts',(31.78723236954,-29.8780636984406,-4.84795915808689));
#36377=CARTESIAN_POINT('Ctrl Pts',(32.4113300033664,-30.2525386437955,-5.91517020465884));
#36378=CARTESIAN_POINT('Ctrl Pts',(33.9184490747708,-31.2284424726334,-7.69457540340442));
#36379=CARTESIAN_POINT('Ctrl Pts',(34.8088600301736,-31.8336791606447,-8.40795287046934));
#36380=CARTESIAN_POINT('Ctrl Pts',(36.7306496231999,-33.1691331027914,-9.37372383732036));
#36381=CARTESIAN_POINT('Ctrl Pts',(37.7740480457988,-33.905760273803,-9.62254086002536));
#36382=CARTESIAN_POINT('Ctrl Pts',(38.7988173067558,-34.6299874229484,-9.62369151535393));
#36383=CARTESIAN_POINT('Ctrl Pts',(31.2747661069635,-31.8324214200723,1.24768201173505));
#36384=CARTESIAN_POINT('Ctrl Pts',(31.2843061312878,-31.7826622501441,0.765479387889553));
#36385=CARTESIAN_POINT('Ctrl Pts',(31.2917666379653,-31.7348562317647,0.332966415967282));
#36386=CARTESIAN_POINT('Ctrl Pts',(31.3978213275647,-31.6085484626322,-0.978922014752047));
#36387=CARTESIAN_POINT('Ctrl Pts',(31.6360823820021,-31.6449008941856,-1.98636136649952));
#36388=CARTESIAN_POINT('Ctrl Pts',(32.3637918610291,-31.9494557448159,-3.81078790537729));
#36389=CARTESIAN_POINT('Ctrl Pts',(32.8768818719313,-32.2252577802596,-4.65460264913351));
#36390=CARTESIAN_POINT('Ctrl Pts',(34.0936348201865,-32.9506697646502,-6.05121512489931));
#36391=CARTESIAN_POINT('Ctrl Pts',(34.817261379824,-33.4089026595985,-6.61423873317492));
#36392=CARTESIAN_POINT('Ctrl Pts',(36.3546651863436,-34.4150618217887,-7.37244739468963));
#36393=CARTESIAN_POINT('Ctrl Pts',(37.2044809778681,-34.9808875866076,-7.56862230174318));
#36394=CARTESIAN_POINT('Ctrl Pts',(38.0218131772945,-35.526728920403,-7.57037421506017));
#36395=CARTESIAN_POINT('Ctrl Pts',(25.5825535213021,-27.9017241322582,1.59647090706388));
#36396=CARTESIAN_POINT('Ctrl Pts',(25.5977646187892,-27.8576356266642,1.15259179092905));
#36397=CARTESIAN_POINT('Ctrl Pts',(25.6076988465248,-27.8006101679573,0.635573104293147));
#36398=CARTESIAN_POINT('Ctrl Pts',(25.7366398496106,-27.6900511858228,-1.86858636168828));
#36399=CARTESIAN_POINT('Ctrl Pts',(26.0667980819016,-27.8867543207229,-3.71029995869047));
#36400=CARTESIAN_POINT('Ctrl Pts',(27.1980083507262,-28.8018888878774,-7.16936247494455));
#36401=CARTESIAN_POINT('Ctrl Pts',(27.9765753735429,-29.5148901762063,-8.73699595768931));
#36402=CARTESIAN_POINT('Ctrl Pts',(29.8931745078317,-31.3430252790121,-11.3730256982303));
#36403=CARTESIAN_POINT('Ctrl Pts',(31.0108564713313,-32.4473861125001,-12.4235805192179));
#36404=CARTESIAN_POINT('Ctrl Pts',(33.4700709138175,-34.895119122769,-13.8529470821642));
#36405=CARTESIAN_POINT('Ctrl Pts',(34.7723177498495,-36.2126515923945,-14.2204718557167));
#36406=CARTESIAN_POINT('Ctrl Pts',(36.0864498658144,-37.5367254229129,-14.2198708430666));
#36407=CARTESIAN_POINT('Ctrl Pts',(24.6306899881717,-27.8942941678688,1.62964634867148));
#36408=CARTESIAN_POINT('Ctrl Pts',(24.6457741833895,-27.8505734813151,1.18947040160635));
#36409=CARTESIAN_POINT('Ctrl Pts',(24.655263156581,-27.7924691428841,0.664244065094566));
#36410=CARTESIAN_POINT('Ctrl Pts',(24.784210314811,-27.6812026446474,-1.95287905118087));
#36411=CARTESIAN_POINT('Ctrl Pts',(25.124655079764,-27.8909128870729,-3.87337387077627));
#36412=CARTESIAN_POINT('Ctrl Pts',(26.297939168344,-28.8532656404736,-7.48792130214935));
#36413=CARTESIAN_POINT('Ctrl Pts',(27.1064590438596,-29.6017140576996,-9.12360836230742));
#36414=CARTESIAN_POINT('Ctrl Pts',(29.1001001803562,-31.5183666699225,-11.8774049927237));
#36415=CARTESIAN_POINT('Ctrl Pts',(30.2623381501061,-32.6750275471261,-12.9732563608774));
#36416=CARTESIAN_POINT('Ctrl Pts',(32.8235411736691,-35.2391241081266,-14.4676858045574));
#36417=CARTESIAN_POINT('Ctrl Pts',(34.1773627942034,-36.6172542487315,-14.8501851005199));
#36418=CARTESIAN_POINT('Ctrl Pts',(35.5466255754742,-38.0044776097613,-14.8499483202528));
#36419=CARTESIAN_POINT('Ctrl Pts',(23.9110153591926,-28.5182079571721,1.62975553161124));
#36420=CARTESIAN_POINT('Ctrl Pts',(23.9260975032016,-28.474493215928,1.18963944141743));
#36421=CARTESIAN_POINT('Ctrl Pts',(23.9355515973832,-28.4163403666077,0.664246507169477));
#36422=CARTESIAN_POINT('Ctrl Pts',(24.0640354326688,-28.3045391652297,-1.95288623088664));
#36423=CARTESIAN_POINT('Ctrl Pts',(24.4051905243227,-28.5150692335449,-3.87317034517924));
#36424=CARTESIAN_POINT('Ctrl Pts',(25.5776818931252,-29.4765070006461,-7.48823335805061));
#36425=CARTESIAN_POINT('Ctrl Pts',(26.3866880329899,-30.225516684417,-9.12349227713595));
#36426=CARTESIAN_POINT('Ctrl Pts',(28.3801534902278,-32.1419665196991,-11.8775764776333));
#36427=CARTESIAN_POINT('Ctrl Pts',(29.5426791470737,-33.29895946217,-12.9726927515289));
#36428=CARTESIAN_POINT('Ctrl Pts',(32.1035612314812,-35.8626855592309,-14.4683433355073));
#36429=CARTESIAN_POINT('Ctrl Pts',(33.457602658903,-37.2410591163324,-14.849803898472));
#36430=CARTESIAN_POINT('Ctrl Pts',(34.8267964255883,-38.6282131180514,-14.8500516281495));
#36431=CARTESIAN_POINT('Ctrl Pts',(23.7833669488542,-29.4615086055165,1.59674386441329));
#36432=CARTESIAN_POINT('Ctrl Pts',(23.7985729183117,-29.4174349631987,1.15301439045616));
#36433=CARTESIAN_POINT('Ctrl Pts',(23.8084199485279,-29.3602882272675,0.63557920948043));
#36434=CARTESIAN_POINT('Ctrl Pts',(23.9362026442621,-29.2483924872748,-1.86860431095269));
#36435=CARTESIAN_POINT('Ctrl Pts',(24.2681366932972,-29.447145186903,-3.70979114469791));
#36436=CARTESIAN_POINT('Ctrl Pts',(25.3973651626803,-30.3599922883086,-7.1701426146977));
#36437=CARTESIAN_POINT('Ctrl Pts',(26.1771478463626,-31.0743967430082,-8.73670574476063));
#36438=CARTESIAN_POINT('Ctrl Pts',(28.0933077825166,-32.9020249034454,-11.3734544105045));
#36439=CARTESIAN_POINT('Ctrl Pts',(29.2117089637491,-34.00721590011,-12.4221714958469));
#36440=CARTESIAN_POINT('Ctrl Pts',(31.670121058349,-36.4540227505297,-13.854590909539));
#36441=CARTESIAN_POINT('Ctrl Pts',(32.972918011877,-37.7721633453099,-14.2195188098581));
#36442=CARTESIAN_POINT('Ctrl Pts',(34.2868769910997,-39.0960641936384,-14.2201291128084));
#36443=CARTESIAN_POINT('Ctrl Pts',(25.6404249706855,-27.772549528674,0.));
#36444=CARTESIAN_POINT('Ctrl Pts',(25.7366398496106,-27.6900511858228,-1.86858636168828));
#36445=CARTESIAN_POINT('Ctrl Pts',(26.0667980819016,-27.8867543207229,-3.71029995869047));
#36446=CARTESIAN_POINT('Ctrl Pts',(27.1980083507262,-28.8018888878774,-7.16936247494455));
#36447=CARTESIAN_POINT('Ctrl Pts',(27.9765753735453,-29.5148901762039,-8.73699595768932));
#36448=CARTESIAN_POINT('Ctrl Pts',(29.0323578083518,-30.5219411006642,-10.1890856763515));
#36449=CARTESIAN_POINT('Ctrl Pts',(29.1314899558969,-30.6168936176694,-10.3203928635195));
#36450=CARTESIAN_POINT('Ctrl Pts',(29.2322214279089,-30.7137407645584,-10.4488603766032));
#36451=CARTESIAN_POINT('Ctrl Pts',(23.8408520862196,-29.3318883095344,-9.99200722162641E-16));
#36452=CARTESIAN_POINT('Ctrl Pts',(23.9362026442621,-29.2483924872748,-1.86860431095269));
#36453=CARTESIAN_POINT('Ctrl Pts',(24.2681366932972,-29.447145186903,-3.70979114469791));
#36454=CARTESIAN_POINT('Ctrl Pts',(25.3973651626803,-30.3599922883086,-7.1701426146977));
#36455=CARTESIAN_POINT('Ctrl Pts',(26.1771478463626,-31.0743967430082,-8.73670574476063));
#36456=CARTESIAN_POINT('Ctrl Pts',(27.2380760953776,-32.0863072351954,-10.1966053555702));
#36457=CARTESIAN_POINT('Ctrl Pts',(27.3427718639698,-32.1866090102816,-10.3350231942247));
#36458=CARTESIAN_POINT('Ctrl Pts',(27.4492538662197,-32.2890256406517,-10.4702558450961));
#36459=CARTESIAN_POINT('Ctrl Pts',(31.6397608122763,-31.4394459897282,1.24689105568321));
#36460=CARTESIAN_POINT('Ctrl Pts',(31.6563000607434,-31.3915079136663,0.764254809547067));
#36461=CARTESIAN_POINT('Ctrl Pts',(31.670740810667,-31.345601660819,0.332948724824433));
#36462=CARTESIAN_POINT('Ctrl Pts',(31.797047945423,-31.2395462388234,-0.978870002751864));
#36463=CARTESIAN_POINT('Ctrl Pts',(32.0225645221739,-31.3034976581367,-1.98783577088394));
#36464=CARTESIAN_POINT('Ctrl Pts',(32.7052670086901,-31.7151448890356,-3.80852727284086));
#36465=CARTESIAN_POINT('Ctrl Pts',(33.1703611269064,-32.0570939854067,-4.65544360718913));
#36466=CARTESIAN_POINT('Ctrl Pts',(34.2727650719446,-32.949753301686,-6.04997283346398));
#36467=CARTESIAN_POINT('Ctrl Pts',(34.9217287192798,-33.5038992564753,-6.61832169897661));
#36468=CARTESIAN_POINT('Ctrl Pts',(36.3026175786965,-34.721296302326,-7.36768403083967));
#36469=CARTESIAN_POINT('Ctrl Pts',(37.0616291372384,-35.4005693947735,-7.57138648704198));
#36470=CARTESIAN_POINT('Ctrl Pts',(37.7934972961795,-36.0576472036358,-7.56962581969431));
#36471=CARTESIAN_POINT('Ctrl Pts',(29.4001542854013,-30.6671178491339,1.35489343606322));
#36472=CARTESIAN_POINT('Ctrl Pts',(29.4162823633167,-30.6203715276518,0.884255668141129));
#36473=CARTESIAN_POINT('Ctrl Pts',(29.4293136556724,-30.5710069006846,0.426397017775727));
#36474=CARTESIAN_POINT('Ctrl Pts',(29.5561964051723,-30.4632865153995,-1.25360819502645));
#36475=CARTESIAN_POINT('Ctrl Pts',(29.8143895731129,-30.5686507749899,-2.51960912779365));
#36476=CARTESIAN_POINT('Ctrl Pts',(30.6351795887969,-31.1352998840589,-4.84647586782702));
#36477=CARTESIAN_POINT('Ctrl Pts',(31.1973201148578,-31.5921137090582,-5.91572199044493));
#36478=CARTESIAN_POINT('Ctrl Pts',(32.5510483450044,-32.7735335073319,-7.69376028694199));
#36479=CARTESIAN_POINT('Ctrl Pts',(33.3448945810284,-33.4977500491925,-8.41063186553761));
#36480=CARTESIAN_POINT('Ctrl Pts',(35.0585937299527,-35.094871091134,-9.37059840622839));
#36481=CARTESIAN_POINT('Ctrl Pts',(35.9854803115295,-35.9713447024497,-9.62435378637548));
#36482=CARTESIAN_POINT('Ctrl Pts',(36.8970924436847,-36.8343596268993,-9.62320046360544));
#36483=CARTESIAN_POINT('Ctrl Pts',(27.3548849305451,-29.4725749263797,1.47293214974064));
#36484=CARTESIAN_POINT('Ctrl Pts',(27.3705645465914,-29.4271284462517,1.0153810678876));
#36485=CARTESIAN_POINT('Ctrl Pts',(27.3820741720678,-29.3740093215554,0.528580803079223));
#36486=CARTESIAN_POINT('Ctrl Pts',(27.509846270387,-29.2647682695536,-1.55402875454047));
#36487=CARTESIAN_POINT('Ctrl Pts',(27.803372614337,-29.4149573143382,-3.10121432123038));
#36488=CARTESIAN_POINT('Ctrl Pts',(28.7756052302995,-30.1516133539791,-5.9812914545136));
#36489=CARTESIAN_POINT('Ctrl Pts',(29.4435926416543,-30.7337162174463,-7.29389406574569));
#36490=CARTESIAN_POINT('Ctrl Pts',(31.072241043673,-32.2310076487121,-9.49113593806079));
#36491=CARTESIAN_POINT('Ctrl Pts',(32.0243541446183,-33.1410090871316,-10.3708286017028));
#36492=CARTESIAN_POINT('Ctrl Pts',(34.1021594176341,-35.1535638963754,-11.5604045561392));
#36493=CARTESIAN_POINT('Ctrl Pts',(35.2124714377991,-36.2455537133498,-11.8694761542189));
#36494=CARTESIAN_POINT('Ctrl Pts',(36.3206928540894,-37.3337834058792,-11.8687142284812));
#36495=CARTESIAN_POINT('Ctrl Pts',(25.5825535213021,-27.9017241322582,1.59647090706388));
#36496=CARTESIAN_POINT('Ctrl Pts',(25.5977646187892,-27.8576356266642,1.15259179092905));
#36497=CARTESIAN_POINT('Ctrl Pts',(25.6076988465248,-27.8006101679573,0.635573104293147));
#36498=CARTESIAN_POINT('Ctrl Pts',(25.7366398496106,-27.6900511858228,-1.86858636168828));
#36499=CARTESIAN_POINT('Ctrl Pts',(26.0667980819016,-27.8867543207229,-3.71029995869047));
#36500=CARTESIAN_POINT('Ctrl Pts',(27.1980083507262,-28.8018888878774,-7.16936247494455));
#36501=CARTESIAN_POINT('Ctrl Pts',(27.9765753735453,-29.5148901762039,-8.73699595768932));
#36502=CARTESIAN_POINT('Ctrl Pts',(29.8931745078293,-31.3430252790145,-11.3730256982303));
#36503=CARTESIAN_POINT('Ctrl Pts',(31.010856471336,-32.4473861125001,-12.4235805192179));
#36504=CARTESIAN_POINT('Ctrl Pts',(33.4700709138127,-34.895119122769,-13.8529470821642));
#36505=CARTESIAN_POINT('Ctrl Pts',(34.7723177498585,-36.2126515923892,-14.2204718557167));
#36506=CARTESIAN_POINT('Ctrl Pts',(36.0864498658144,-37.5367254229129,-14.2198708430666));
#36507=CARTESIAN_POINT('Ctrl Pts',(23.7833669488542,-29.4615086055165,1.59674386441329));
#36508=CARTESIAN_POINT('Ctrl Pts',(23.7985729183117,-29.4174349631987,1.15301439045615));
#36509=CARTESIAN_POINT('Ctrl Pts',(23.8084199485278,-29.3602882272675,0.635579209480434));
#36510=CARTESIAN_POINT('Ctrl Pts',(23.9362026442621,-29.2483924872748,-1.86860431095269));
#36511=CARTESIAN_POINT('Ctrl Pts',(24.2681366932972,-29.447145186903,-3.70979114469911));
#36512=CARTESIAN_POINT('Ctrl Pts',(25.3973651626803,-30.3599922883086,-7.17014261469651));
#36513=CARTESIAN_POINT('Ctrl Pts',(26.1771478463602,-31.0743967430034,-8.73670574475585));
#36514=CARTESIAN_POINT('Ctrl Pts',(28.093307782519,-32.9020249034502,-11.3734544105093));
#36515=CARTESIAN_POINT('Ctrl Pts',(29.2117089637491,-34.00721590011,-12.4221714958517));
#36516=CARTESIAN_POINT('Ctrl Pts',(31.670121058349,-36.4540227505297,-13.8545909095342));
#36517=CARTESIAN_POINT('Ctrl Pts',(32.9729180118699,-37.772163345317,-14.2195188098628));
#36518=CARTESIAN_POINT('Ctrl Pts',(34.2868769910997,-39.0960641936384,-14.2201291128084));
#36519=CARTESIAN_POINT('Ctrl Pts',(25.0869579521465,-31.4387285991346,1.47327622041466));
#36520=CARTESIAN_POINT('Ctrl Pts',(25.1026311041632,-31.3933008545996,1.01591376687672));
#36521=CARTESIAN_POINT('Ctrl Pts',(25.1140308146305,-31.3400288564348,0.52858849884529));
#36522=CARTESIAN_POINT('Ctrl Pts',(25.2403428328606,-31.2291027822936,-1.55405138011005));
#36523=CARTESIAN_POINT('Ctrl Pts',(25.5361076454386,-31.3818753629957,-3.10057294640152));
#36524=CARTESIAN_POINT('Ctrl Pts',(26.5058421455966,-32.1156479855689,-5.98227484335136));
#36525=CARTESIAN_POINT('Ctrl Pts',(27.1753619328071,-32.6995195810239,-7.29352824390757));
#36526=CARTESIAN_POINT('Ctrl Pts',(28.8034567128163,-34.196171996717,-9.49167634235024));
#36527=CARTESIAN_POINT('Ctrl Pts',(29.7564764086093,-35.1072198799437,-10.3690524867829));
#36528=CARTESIAN_POINT('Ctrl Pts',(31.833270298808,-37.118607237774,-11.5624766483317));
#36529=CARTESIAN_POINT('Ctrl Pts',(32.944279264244,-38.2113611019662,-11.8682745704546));
#36530=CARTESIAN_POINT('Ctrl Pts',(34.0522789304532,-39.2993752576346,-11.8690397849988));
#36531=CARTESIAN_POINT('Ctrl Pts',(25.9793365537795,-33.6327571359873,1.35541241355846));
#36532=CARTESIAN_POINT('Ctrl Pts',(25.9954548817075,-33.5860390742511,0.885059162330388));
#36533=CARTESIAN_POINT('Ctrl Pts',(26.0083203842378,-33.5364438612596,0.426408625650778));
#36534=CARTESIAN_POINT('Ctrl Pts',(26.1330008283223,-33.4261818802092,-1.2536423222053));
#36535=CARTESIAN_POINT('Ctrl Pts',(26.3945703806216,-33.5354430048945,-2.51864171287673));
#36536=CARTESIAN_POINT('Ctrl Pts',(27.211592374269,-34.0977429244413,-4.84795915807732));
#36537=CARTESIAN_POINT('Ctrl Pts',(27.7760442527403,-34.5572246086001,-5.91517020467798));
#36538=CARTESIAN_POINT('Ctrl Pts',(29.1289374295578,-35.7376805505258,-7.69457540338525));
#36539=CARTESIAN_POINT('Ctrl Pts',(29.9241511239614,-36.4634754928305,-8.40795287036384));
#36540=CARTESIAN_POINT('Ctrl Pts',(31.6363247580161,-38.0588356145494,-9.37372383742583));
#36541=CARTESIAN_POINT('Ctrl Pts',(32.5642699125034,-38.9364560608574,-9.62254085984917));
#36542=CARTESIAN_POINT('Ctrl Pts',(33.4755402303451,-39.799151493507,-9.62369151535381));
#36543=CARTESIAN_POINT('Ctrl Pts',(26.426208176239,-35.9592765491249,1.24768201173542));
#36544=CARTESIAN_POINT('Ctrl Pts',(26.4427325650799,-35.9113815427798,0.765479387872765));
#36545=CARTESIAN_POINT('Ctrl Pts',(26.4569206403346,-35.8651238615762,0.332966415994299));
#36546=CARTESIAN_POINT('Ctrl Pts',(26.5798713158818,-35.7551948794137,-0.978922014831213));
#36547=CARTESIAN_POINT('Ctrl Pts',(26.81053372586,-35.8250853790502,-1.98636136652122));
#36548=CARTESIAN_POINT('Ctrl Pts',(27.487493497402,-36.2301041572641,-3.81078790535579));
#36549=CARTESIAN_POINT('Ctrl Pts',(27.9561102696818,-36.576119247571,-4.65460264916223));
#36550=CARTESIAN_POINT('Ctrl Pts',(29.0572415381562,-37.467309582976,-6.0512151248706));
#36551=CARTESIAN_POINT('Ctrl Pts',(29.7082892825749,-38.0238611245159,-6.61423873302147));
#36552=CARTESIAN_POINT('Ctrl Pts',(31.0868531563715,-39.2385744113942,-7.37244739484306));
#36553=CARTESIAN_POINT('Ctrl Pts',(31.847493646553,-39.9195822825653,-7.56862230150026));
#36554=CARTESIAN_POINT('Ctrl Pts',(32.5788252613912,-40.57618623849,-7.57037421506001));
#36555=CARTESIAN_POINT('Ctrl Pts',(21.3513306581891,-31.2585017743467,1.59647086199746));
#36556=CARTESIAN_POINT('Ctrl Pts',(21.3726613764945,-31.2170267923822,1.15259176012307));
#36557=CARTESIAN_POINT('Ctrl Pts',(21.3906100567637,-31.161995560763,0.635573083853244));
#36558=CARTESIAN_POINT('Ctrl Pts',(21.5339728087505,-31.0709121284164,-1.86858636172315));
#36559=CARTESIAN_POINT('Ctrl Pts',(21.8327767315744,-31.3125995244281,-3.71029995869404));
#36560=CARTESIAN_POINT('Ctrl Pts',(22.8222356829128,-32.3794073477002,-7.16936247494135));
#36561=CARTESIAN_POINT('Ctrl Pts',(23.4914073530124,-33.1959529509023,-8.73699595767989));
#36562=CARTESIAN_POINT('Ctrl Pts',(25.128327520199,-35.2782407701336,-11.3730256982401));
#36563=CARTESIAN_POINT('Ctrl Pts',(26.0774661593741,-36.5304235306262,-12.4235805192514));
#36564=CARTESIAN_POINT('Ctrl Pts',(28.1633006173374,-39.3032248537516,-13.8529470821311));
#36565=CARTESIAN_POINT('Ctrl Pts',(29.2647880382297,-40.7926757902223,-14.2204718555883));
#36566=CARTESIAN_POINT('Ctrl Pts',(30.3771088306736,-42.290292958107,-14.2198708430668));
#36567=CARTESIAN_POINT('Ctrl Pts',(20.4102131175326,-31.1156831315059,1.62964630360506));
#36568=CARTESIAN_POINT('Ctrl Pts',(20.4313658791523,-31.0745541646277,1.18947037067355));
#36569=CARTESIAN_POINT('Ctrl Pts',(20.4490273775128,-31.0183916683951,0.664244043735995));
#36570=CARTESIAN_POINT('Ctrl Pts',(20.5924969120299,-30.9266087974369,-1.95287905122728));
#36571=CARTESIAN_POINT('Ctrl Pts',(20.8996315610477,-31.1826348335737,-3.87337387078343));
#36572=CARTESIAN_POINT('Ctrl Pts',(21.9240162327731,-32.3021679589246,-7.48792130214246));
#36573=CARTESIAN_POINT('Ctrl Pts',(22.6177912263091,-33.1580626257345,-9.12360836229315));
#36574=CARTESIAN_POINT('Ctrl Pts',(24.3183718641675,-35.3389311938522,-11.8774049927382));
#36575=CARTESIAN_POINT('Ctrl Pts',(25.3041699214186,-36.6492226398526,-12.9732563608963));
#36576=CARTESIAN_POINT('Ctrl Pts',(27.4743946038814,-39.5517175889618,-14.4676858045386));
#36577=CARTESIAN_POINT('Ctrl Pts',(28.6183079046584,-41.10848925655,-14.8501851004819));
#36578=CARTESIAN_POINT('Ctrl Pts',(29.7762110964233,-42.6764590955605,-14.8499483202528));
#36579=CARTESIAN_POINT('Ctrl Pts',(19.6090715485701,-31.6308259996109,1.62975548654487));
#36580=CARTESIAN_POINT('Ctrl Pts',(19.6302214337609,-31.5897026256071,1.18963941047971));
#36581=CARTESIAN_POINT('Ctrl Pts',(19.6478553119351,-31.5334871484505,0.66424648581248));
#36582=CARTESIAN_POINT('Ctrl Pts',(19.7909423356753,-31.4411090791454,-1.95288623093789));
#36583=CARTESIAN_POINT('Ctrl Pts',(20.0986634078842,-31.6980476865377,-3.87317034519232));
#36584=CARTESIAN_POINT('Ctrl Pts',(21.1223936447217,-32.8165623230617,-7.48823335803764));
#36585=CARTESIAN_POINT('Ctrl Pts',(21.8165700765696,-33.6730817461624,-9.12349227711679));
#36586=CARTESIAN_POINT('Ctrl Pts',(23.5170056814996,-35.8537245995369,-11.8775764776525));
#36587=CARTESIAN_POINT('Ctrl Pts',(24.5030412397929,-37.1643856730114,-12.9726927515286));
#36588=CARTESIAN_POINT('Ctrl Pts',(26.6730009723108,-40.0664682545599,-14.4683433355076));
#36589=CARTESIAN_POINT('Ctrl Pts',(27.8170972008577,-41.6235121428201,-14.8498038985433));
#36590=CARTESIAN_POINT('Ctrl Pts',(28.9749419513877,-43.1914035066782,-14.8500516281494));
#36591=CARTESIAN_POINT('Ctrl Pts',(19.3484767357829,-32.5463589446092,1.59674381934696));
#36592=CARTESIAN_POINT('Ctrl Pts',(19.3698002630062,-32.5048979448321,1.15301435963818));
#36593=CARTESIAN_POINT('Ctrl Pts',(19.3876798928189,-32.4497342608979,0.635579189044451));
#36594=CARTESIAN_POINT('Ctrl Pts',(19.5300863678652,-32.3571628326983,-1.86860431099967));
#36595=CARTESIAN_POINT('Ctrl Pts',(19.8303563486669,-32.6011316568334,-3.70979114471326));
#36596=CARTESIAN_POINT('Ctrl Pts',(20.8181792127831,-33.6653932580479,-7.17014261468231));
#36597=CARTESIAN_POINT('Ctrl Pts',(21.4883544786661,-34.4835007519627,-8.7367057447366));
#36598=CARTESIAN_POINT('Ctrl Pts',(23.124912063527,-36.5652242843549,-11.3734544105284));
#36599=CARTESIAN_POINT('Ctrl Pts',(24.0746444553041,-37.8183311135135,-12.4221714958272));
#36600=CARTESIAN_POINT('Ctrl Pts',(26.1598165384169,-40.5901015177564,-13.8545909095583));
#36601=CARTESIAN_POINT('Ctrl Pts',(27.2617619321778,-42.0802326794159,-14.2195188100387));
#36602=CARTESIAN_POINT('Ctrl Pts',(28.3739359680845,-43.5776539859013,-14.2201291128083));
#36603=CARTESIAN_POINT('Ctrl Pts',(21.4269965203137,-31.1388779521432,0.));
#36604=CARTESIAN_POINT('Ctrl Pts',(21.5339728087505,-31.0709121284164,-1.86858636172315));
#36605=CARTESIAN_POINT('Ctrl Pts',(21.8327767315744,-31.3125995244281,-3.71029995869284));
#36606=CARTESIAN_POINT('Ctrl Pts',(22.8222356829128,-32.3794073477002,-7.16936247494255));
#36607=CARTESIAN_POINT('Ctrl Pts',(23.4914073530124,-33.1959529508975,-8.7369959576799));
#36608=CARTESIAN_POINT('Ctrl Pts',(24.3931251555408,-34.3430070554509,-10.1890856763512));
#36609=CARTESIAN_POINT('Ctrl Pts',(24.4777351286612,-34.4511010682878,-10.320392863519));
#36610=CARTESIAN_POINT('Ctrl Pts',(24.5636585134848,-34.5612980340113,-10.4488603766026));
#36611=CARTESIAN_POINT('Ctrl Pts',(19.4238236466304,-32.4262389885815,-1.83186799063151E-15));
#36612=CARTESIAN_POINT('Ctrl Pts',(19.5300863678652,-32.3571628326983,-1.86860431099967));
#36613=CARTESIAN_POINT('Ctrl Pts',(19.8303563486669,-32.6011316568334,-3.70979114471326));
#36614=CARTESIAN_POINT('Ctrl Pts',(20.8181792127831,-33.6653932580479,-7.17014261468231));
#36615=CARTESIAN_POINT('Ctrl Pts',(21.4883544786661,-34.4835007519627,-8.7367057447366));
#36616=CARTESIAN_POINT('Ctrl Pts',(22.3944741298276,-35.6360972865638,-10.1966053555717));
#36617=CARTESIAN_POINT('Ctrl Pts',(22.4838298155557,-35.750277895577,-10.3350231942271));
#36618=CARTESIAN_POINT('Ctrl Pts',(22.5746525783696,-35.8668060412515,-10.4702558450987));
#36619=CARTESIAN_POINT('Ctrl Pts',(26.8434139987109,-35.6222452002844,1.24689101061693));
#36620=CARTESIAN_POINT('Ctrl Pts',(26.866607200265,-35.5771488466461,0.764254780049364));
#36621=CARTESIAN_POINT('Ctrl Pts',(26.8874341048552,-35.5337649883207,0.332948714090238));
#36622=CARTESIAN_POINT('Ctrl Pts',(27.0275488741942,-35.4467644376545,-0.978870002691829));
#36623=CARTESIAN_POINT('Ctrl Pts',(27.2416687814358,-35.5421592790288,-1.9878357708727));
#36624=CARTESIAN_POINT('Ctrl Pts',(27.8588388319676,-36.0467752284862,-3.80852727285255));
#36625=CARTESIAN_POINT('Ctrl Pts',(28.2705345323081,-36.4514335703569,-4.6554436072038));
#36626=CARTESIAN_POINT('Ctrl Pts',(29.2346789284779,-37.4918953411199,-6.04997283344998));
#36627=CARTESIAN_POINT('Ctrl Pts',(29.7981738697234,-38.1327580455423,-6.61832169904879));
#36628=CARTESIAN_POINT('Ctrl Pts',(30.9917536078527,-39.5342847195952,-7.36768403076832));
#36629=CARTESIAN_POINT('Ctrl Pts',(31.6463688825543,-40.3146623988151,-7.57138648661861));
#36630=CARTESIAN_POINT('Ctrl Pts',(32.2772757571271,-41.0692078014243,-7.56962581969465));
#36631=CARTESIAN_POINT('Ctrl Pts',(24.7365171914562,-34.539049005888,1.35489339099691));
#36632=CARTESIAN_POINT('Ctrl Pts',(24.7591338032426,-34.4950737607861,0.884255638235974));
#36633=CARTESIAN_POINT('Ctrl Pts',(24.7790577744578,-34.4480661428797,0.426397004045326));
#36634=CARTESIAN_POINT('Ctrl Pts',(24.9199792485556,-34.3594994944374,-1.25360819499821));
#36635=CARTESIAN_POINT('Ctrl Pts',(25.1605494847799,-34.5005360168067,-2.5196091277897));
#36636=CARTESIAN_POINT('Ctrl Pts',(25.8923424652774,-35.1782280532491,-4.84647586783132));
#36637=CARTESIAN_POINT('Ctrl Pts',(26.3837498256842,-35.7103931102545,-5.91572199044753));
#36638=CARTESIAN_POINT('Ctrl Pts',(27.5555654868577,-37.0724433726229,-7.69376028693985));
#36639=CARTESIAN_POINT('Ctrl Pts',(28.2382647528021,-37.9022645329766,-8.41063186558564));
#36640=CARTESIAN_POINT('Ctrl Pts',(29.7072268925326,-39.7270140028395,-9.37059840618092));
#36641=CARTESIAN_POINT('Ctrl Pts',(30.4999439048052,-40.7264760905893,-9.62435378611397));
#36642=CARTESIAN_POINT('Ctrl Pts',(31.27945731062,-41.7104427005358,-9.62320046360565));
#36643=CARTESIAN_POINT('Ctrl Pts',(22.8820669124599,-33.065592630237,1.47293210467427));
#36644=CARTESIAN_POINT('Ctrl Pts',(22.9040546403826,-33.0228401731498,1.01538103754122));
#36645=CARTESIAN_POINT('Ctrl Pts',(22.9230067538248,-32.9718997171416,0.528580786071612));
#36646=CARTESIAN_POINT('Ctrl Pts',(23.0650249378515,-32.8819544477584,-1.55402875454427));
#36647=CARTESIAN_POINT('Ctrl Pts',(23.3341894772925,-33.072387938809,-3.10121432123136));
#36648=CARTESIAN_POINT('Ctrl Pts',(24.1916890818784,-33.9399090096345,-5.98129145451293));
#36649=CARTESIAN_POINT('Ctrl Pts',(24.7700354696729,-34.6111514256828,-7.29389406574346));
#36650=CARTESIAN_POINT('Ctrl Pts',(26.1690197914296,-36.3249834230533,-9.4911359380634));
#36651=CARTESIAN_POINT('Ctrl Pts',(26.981935046259,-37.3612221809256,-10.3708286017411));
#36652=CARTESIAN_POINT('Ctrl Pts',(28.7521748453974,-39.6489946054402,-11.5604045561013));
#36653=CARTESIAN_POINT('Ctrl Pts',(29.6957791360107,-40.8878834161155,-11.869476154062));
#36654=CARTESIAN_POINT('Ctrl Pts',(30.6378492234115,-42.1227528511813,-11.8687142284813));
#36655=CARTESIAN_POINT('Ctrl Pts',(21.3513306581891,-31.2585017743466,1.59647086199746));
#36656=CARTESIAN_POINT('Ctrl Pts',(21.3726613764946,-31.2170267923868,1.15259176012262));
#36657=CARTESIAN_POINT('Ctrl Pts',(21.3906100567637,-31.161995560763,0.635573083853244));
#36658=CARTESIAN_POINT('Ctrl Pts',(21.5339728087505,-31.0709121284164,-1.86858636172315));
#36659=CARTESIAN_POINT('Ctrl Pts',(21.8327767315744,-31.3125995244281,-3.71029995869284));
#36660=CARTESIAN_POINT('Ctrl Pts',(22.8222356829128,-32.3794073477002,-7.16936247494255));
#36661=CARTESIAN_POINT('Ctrl Pts',(23.4914073530124,-33.1959529508975,-8.7369959576799));
#36662=CARTESIAN_POINT('Ctrl Pts',(25.1283275201989,-35.2782407701384,-11.3730256982401));
#36663=CARTESIAN_POINT('Ctrl Pts',(26.0774661593717,-36.5304235306214,-12.4235805192514));
#36664=CARTESIAN_POINT('Ctrl Pts',(28.1633006173398,-39.3032248537564,-13.8529470821311));
#36665=CARTESIAN_POINT('Ctrl Pts',(29.2647880382258,-40.7926757902203,-14.2204718555836));
#36666=CARTESIAN_POINT('Ctrl Pts',(30.3771088306736,-42.290292958107,-14.2198708430668));
#36667=CARTESIAN_POINT('Ctrl Pts',(19.3484767357829,-32.5463589446092,1.59674381934696));
#36668=CARTESIAN_POINT('Ctrl Pts',(19.3698002630062,-32.5048979448321,1.15301435963818));
#36669=CARTESIAN_POINT('Ctrl Pts',(19.3876798928189,-32.4497342608979,0.635579189044451));
#36670=CARTESIAN_POINT('Ctrl Pts',(19.5300863678652,-32.3571628326983,-1.86860431099967));
#36671=CARTESIAN_POINT('Ctrl Pts',(19.8303563486669,-32.6011316568334,-3.70979114471326));
#36672=CARTESIAN_POINT('Ctrl Pts',(20.8181792127831,-33.6653932580479,-7.17014261468231));
#36673=CARTESIAN_POINT('Ctrl Pts',(21.4883544786661,-34.4835007519627,-8.7367057447366));
#36674=CARTESIAN_POINT('Ctrl Pts',(23.124912063527,-36.5652242843549,-11.3734544105284));
#36675=CARTESIAN_POINT('Ctrl Pts',(24.0746444553089,-37.8183311135135,-12.4221714958272));
#36676=CARTESIAN_POINT('Ctrl Pts',(26.1598165384121,-40.5901015177564,-13.8545909095583));
#36677=CARTESIAN_POINT('Ctrl Pts',(27.261761932179,-42.0802326794176,-14.2195188100435));
#36678=CARTESIAN_POINT('Ctrl Pts',(28.3739359680845,-43.5776539859013,-14.2201291128083));
#36679=CARTESIAN_POINT('Ctrl Pts',(20.3574113186621,-34.6889740324162,1.47327617534843));
#36680=CARTESIAN_POINT('Ctrl Pts',(20.379389982015,-34.6462392002803,1.01591373651561));
#36681=CARTESIAN_POINT('Ctrl Pts',(20.398255055351,-34.5951317842797,0.528588481842604));
#36682=CARTESIAN_POINT('Ctrl Pts',(20.539067824495,-34.5033108528715,-1.55405138012912));
#36683=CARTESIAN_POINT('Ctrl Pts',(20.8100803726341,-34.6966201503891,-3.10057294642143));
#36684=CARTESIAN_POINT('Ctrl Pts',(21.6655176417181,-35.5609316342938,-5.98227484333125));
#36685=CARTESIAN_POINT('Ctrl Pts',(22.2451290911725,-36.234142858994,-7.29352824388825));
#36686=CARTESIAN_POINT('Ctrl Pts',(23.6436563673638,-37.9472635563897,-9.49167634236925));
#36687=CARTESIAN_POINT('Ctrl Pts',(24.457320064615,-38.9846671296937,-10.3690524867584));
#36688=CARTESIAN_POINT('Ctrl Pts',(26.2267249209897,-41.2711400509677,-11.5624766483557));
#36689=CARTESIAN_POINT('Ctrl Pts',(27.1709103277658,-42.5108843176116,-11.86827457064));
#36690=CARTESIAN_POINT('Ctrl Pts',(28.1127915962414,-43.7455088513561,-11.8690397849986));
#36691=CARTESIAN_POINT('Ctrl Pts',(20.9284639764449,-36.9876692386616,1.35541236849233));
#36692=CARTESIAN_POINT('Ctrl Pts',(20.9510669157225,-36.9437205780704,0.885059132402747));
#36693=CARTESIAN_POINT('Ctrl Pts',(20.9708596003777,-36.8964611268003,0.426408611927824));
#36694=CARTESIAN_POINT('Ctrl Pts',(21.1099628922185,-36.8050653317413,-1.25364232220009));
#36695=CARTESIAN_POINT('Ctrl Pts',(21.353320564272,-36.950439564209,-2.51864171289876));
#36696=CARTESIAN_POINT('Ctrl Pts',(22.0820028300379,-37.6232904342815,-4.84795915805486));
#36697=CARTESIAN_POINT('Ctrl Pts',(22.575318340659,-38.1584251351965,-5.91517020465855));
#36698=CARTESIAN_POINT('Ctrl Pts',(23.7464446191649,-39.5194025113536,-7.69457540340414));
#36699=CARTESIAN_POINT('Ctrl Pts',(24.430272794963,-40.3509806159742,-8.40795287032015));
#36700=CARTESIAN_POINT('Ctrl Pts',(25.8979755524144,-42.1737699858021,-9.37372383746887));
#36701=CARTESIAN_POINT('Ctrl Pts',(26.6915771512776,-43.1745178860539,-9.62254086016299));
#36702=CARTESIAN_POINT('Ctrl Pts',(27.470797690331,-44.1581196109332,-9.6236915153536));
#36703=CARTESIAN_POINT('Ctrl Pts',(21.0396888561029,-39.3541045014167,1.24768196666942));
#36704=CARTESIAN_POINT('Ctrl Pts',(21.0628612198541,-39.3090486643396,0.765479358340059));
#36705=CARTESIAN_POINT('Ctrl Pts',(21.0834880350321,-39.2652809952898,0.332966405271473));
#36706=CARTESIAN_POINT('Ctrl Pts',(21.2208317742708,-39.1739686379383,-0.978922014806281));
#36707=CARTESIAN_POINT('Ctrl Pts',(21.4391999182059,-39.2759744365989,-1.98636136655255));
#36708=CARTESIAN_POINT('Ctrl Pts',(22.0516290336034,-39.773212128077,-3.81078790532374));
#36709=CARTESIAN_POINT('Ctrl Pts',(22.4662328811655,-40.182396403819,-4.65460264913786));
#36710=CARTESIAN_POINT('Ctrl Pts',(23.4293266125158,-41.2212230249917,-6.05121512489411));
#36711=CARTESIAN_POINT('Ctrl Pts',(23.9945420870899,-41.8647634287527,-6.61423873295368));
#36712=CARTESIAN_POINT('Ctrl Pts',(25.1862024432922,-43.2633027806342,-7.37244739490986));
#36713=CARTESIAN_POINT('Ctrl Pts',(25.8421831847501,-44.0456294021952,-7.56862230195687));
#36714=CARTESIAN_POINT('Ctrl Pts',(26.4726264127399,-44.7996294168198,-7.57037421505967));
#36715=CARTESIAN_POINT('Ctrl Pts',(16.6854562787119,-33.9789464595044,1.5964707761033));
#36716=CARTESIAN_POINT('Ctrl Pts',(16.7124723847588,-33.9409293131124,1.15259170142611));
#36717=CARTESIAN_POINT('Ctrl Pts',(16.7380701329864,-33.8890125875568,0.635573044868113));
#36718=CARTESIAN_POINT('Ctrl Pts',(16.8929361804822,-33.8192589011466,-1.86858636170883));
#36719=CARTESIAN_POINT('Ctrl Pts',(17.1543030075059,-34.1010104999082,-3.71029995866542));
#36720=CARTESIAN_POINT('Ctrl Pts',(17.9818681105058,-35.297774448411,-7.16936247496946));
#36721=CARTESIAN_POINT('Ctrl Pts',(18.5280220223184,-36.2012418527466,-8.7369959577178));
#36722=CARTESIAN_POINT('Ctrl Pts',(19.8519402484503,-38.4952930132141,-11.3730256982018));
#36723=CARTESIAN_POINT('Ctrl Pts',(20.6132138377593,-39.8698068705691,-12.4235805191893));
#36724=CARTESIAN_POINT('Ctrl Pts',(22.2832067363974,-42.9112302679935,-13.8529470821929));
#36725=CARTESIAN_POINT('Ctrl Pts',(23.1615116341715,-44.5422787457887,-14.2204718557452));
#36726=CARTESIAN_POINT('Ctrl Pts',(24.0493774600887,-46.1829520838075,-14.2198708430667));
#36727=CARTESIAN_POINT('Ctrl Pts',(15.7742431696982,-33.7036465139256,1.62964621771091));
#36728=CARTESIAN_POINT('Ctrl Pts',(15.801033887339,-33.6659465347865,1.18947031174229));
#36729=CARTESIAN_POINT('Ctrl Pts',(15.8265083724794,-33.6128691890278,0.66424400298923));
#36730=CARTESIAN_POINT('Ctrl Pts',(15.9815796561098,-33.5424383800186,-1.9528790512035));
#36731=CARTESIAN_POINT('Ctrl Pts',(16.2491518132913,-33.8395682581736,-3.8733738707548));
#36732=CARTESIAN_POINT('Ctrl Pts',(17.103783550365,-35.0934912894727,-7.48792130217063));
#36733=CARTESIAN_POINT('Ctrl Pts',(17.6686904036183,-36.0394086587071,-9.12360836231914));
#36734=CARTESIAN_POINT('Ctrl Pts',(19.041591625316,-38.4400969876946,-11.8774049927119));
#36735=CARTESIAN_POINT('Ctrl Pts',(19.8308817645067,-39.8773452471076,-12.9732563608583));
#36736=CARTESIAN_POINT('Ctrl Pts',(21.5659485893962,-43.0591521575738,-14.4676858045765));
#36737=CARTESIAN_POINT('Ctrl Pts',(22.4766667937634,-44.7628739707726,-14.8501851005341));
#36738=CARTESIAN_POINT('Ctrl Pts',(23.3996388269518,-46.4796709429186,-14.8499483202528));
#36739=CARTESIAN_POINT('Ctrl Pts',(14.907943592795,-34.099531637587,1.62975540065068));
#36740=CARTESIAN_POINT('Ctrl Pts',(14.934730667332,-34.0618367850497,1.18963935154091));
#36741=CARTESIAN_POINT('Ctrl Pts',(14.9601853533923,-34.008703066853,0.664246445062532));
#36742=CARTESIAN_POINT('Ctrl Pts',(15.1149627252082,-33.9376286807998,-1.9528862309052));
#36743=CARTESIAN_POINT('Ctrl Pts',(15.3829854642134,-34.2357452982714,-3.87317034516976));
#36744=CARTESIAN_POINT('Ctrl Pts',(16.237114373674,-35.4885670717109,-7.48823335805989));
#36745=CARTESIAN_POINT('Ctrl Pts',(16.8023296670996,-36.4351599687639,-9.12349227712133));
#36746=CARTESIAN_POINT('Ctrl Pts',(18.1751194546256,-38.8356042400712,-11.8775764776479));
#36747=CARTESIAN_POINT('Ctrl Pts',(18.9645920739779,-40.2732521646236,-12.9726927515242));
#36748=CARTESIAN_POINT('Ctrl Pts',(20.6994553317568,-43.4546131985424,-14.468343335512));
#36749=CARTESIAN_POINT('Ctrl Pts',(21.6103158609142,-45.1586304949195,-14.8498038985005));
#36750=CARTESIAN_POINT('Ctrl Pts',(22.53324121589,-46.8753414736306,-14.8500516281495));
#36751=CARTESIAN_POINT('Ctrl Pts',(14.5197073364539,-34.968659268658,1.5967437334527));
#36752=CARTESIAN_POINT('Ctrl Pts',(14.5467143347417,-34.9306549387484,1.15301430092464));
#36753=CARTESIAN_POINT('Ctrl Pts',(14.5722625852684,-34.8785972821207,0.635579150051368));
#36754=CARTESIAN_POINT('Ctrl Pts',(14.7263938532288,-34.8072346530974,-1.86860431096307));
#36755=CARTESIAN_POINT('Ctrl Pts',(14.9888871348065,-35.0914531001455,-3.70979114469921));
#36756=CARTESIAN_POINT('Ctrl Pts',(15.8151951687831,-36.2854639040137,-7.17014261469621));
#36757=CARTESIAN_POINT('Ctrl Pts',(16.3621201810158,-37.190620127891,-8.73670574472687));
#36758=CARTESIAN_POINT('Ctrl Pts',(17.6857598217302,-39.4840611441532,-11.3734544105381));
#36759=CARTESIAN_POINT('Ctrl Pts',(18.4474896114335,-40.8595741643688,-12.4221714958517));
#36760=CARTESIAN_POINT('Ctrl Pts',(20.1169735923025,-43.8998828704052,-13.854590909534));
#36761=CARTESIAN_POINT('Ctrl Pts',(20.995634995294,-45.5316698260174,-14.2195188099104));
#36762=CARTESIAN_POINT('Ctrl Pts',(21.8833834324342,-47.1721284105875,-14.2201291128084));
#36763=CARTESIAN_POINT('Ctrl Pts',(16.7773762111438,-33.8713086176154,0.));
#36764=CARTESIAN_POINT('Ctrl Pts',(16.8929361804822,-33.8192589011466,-1.86858636170883));
#36765=CARTESIAN_POINT('Ctrl Pts',(17.1543030075107,-34.1010104999082,-3.71029995866542));
#36766=CARTESIAN_POINT('Ctrl Pts',(17.981868110501,-35.297774448411,-7.16936247496945));
#36767=CARTESIAN_POINT('Ctrl Pts',(18.5280220223185,-36.2012418527466,-8.73699595771779));
#36768=CARTESIAN_POINT('Ctrl Pts',(19.2573188185374,-37.4649484236423,-10.1890856763477));
#36769=CARTESIAN_POINT('Ctrl Pts',(19.3256842021847,-37.5839834499261,-10.3203928635122));
#36770=CARTESIAN_POINT('Ctrl Pts',(19.3950503474966,-37.7052869420423,-10.4488603765928));
#36771=CARTESIAN_POINT('Ctrl Pts',(14.6113821712778,-34.8604849513725,1.33226762955019E-15));
#36772=CARTESIAN_POINT('Ctrl Pts',(14.7263938532288,-34.8072346530974,-1.86860431096307));
#36773=CARTESIAN_POINT('Ctrl Pts',(14.9888871348065,-35.0914531001455,-3.70979114469921));
#36774=CARTESIAN_POINT('Ctrl Pts',(15.8151951687831,-36.2854639040137,-7.17014261469621));
#36775=CARTESIAN_POINT('Ctrl Pts',(16.3621201810158,-37.190620127891,-8.73670574472687));
#36776=CARTESIAN_POINT('Ctrl Pts',(17.094985251334,-38.4604391631886,-10.1966053555743));
#36777=CARTESIAN_POINT('Ctrl Pts',(17.1671818301258,-38.5861742181928,-10.3350231942322));
#36778=CARTESIAN_POINT('Ctrl Pts',(17.2404964639728,-38.7144417021593,-10.4702558451063));
#36779=CARTESIAN_POINT('Ctrl Pts',(21.5006126898289,-39.0798782217545,1.24689092472231));
#36780=CARTESIAN_POINT('Ctrl Pts',(21.5299876965087,-39.0385416232163,0.764254723798825));
#36781=CARTESIAN_POINT('Ctrl Pts',(21.5567767789514,-38.9985633313588,0.332948693682486));
#36782=CARTESIAN_POINT('Ctrl Pts',(21.707846848885,-38.9323887327204,-0.978870002727929));
#36783=CARTESIAN_POINT('Ctrl Pts',(21.9062112227949,-39.0572850320887,-1.98783577086018));
#36784=CARTESIAN_POINT('Ctrl Pts',(22.4452850348812,-39.6445971746381,-3.80852727286484));
#36785=CARTESIAN_POINT('Ctrl Pts',(22.7952013801788,-40.1037270849617,-4.65544360727524));
#36786=CARTESIAN_POINT('Ctrl Pts',(23.6014590278217,-41.2708105092157,-6.04997283337807));
#36787=CARTESIAN_POINT('Ctrl Pts',(24.0680141308967,-41.9853438467174,-6.61832169891444));
#36788=CARTESIAN_POINT('Ctrl Pts',(25.0499869065097,-43.5424691073157,-7.36768403090209));
#36789=CARTESIAN_POINT('Ctrl Pts',(25.5868798186132,-44.4080651338149,-7.57138648702774));
#36790=CARTESIAN_POINT('Ctrl Pts',(26.1039819636362,-45.2447177621913,-7.56962581969438));
#36791=CARTESIAN_POINT('Ctrl Pts',(19.5693159454015,-37.7078647243941,1.35489330510241));
#36792=CARTESIAN_POINT('Ctrl Pts',(19.5979606808328,-37.6675557657759,0.8842555812278));
#36793=CARTESIAN_POINT('Ctrl Pts',(19.6243717351794,-37.6238620982266,0.426396977899446));
#36794=CARTESIAN_POINT('Ctrl Pts',(19.7764631777508,-37.5562521484589,-1.25360819501416));
#36795=CARTESIAN_POINT('Ctrl Pts',(19.9945131659745,-37.7300898366309,-2.51960912777466));
#36796=CARTESIAN_POINT('Ctrl Pts',(20.6224119165102,-38.5050289449296,-4.84647586784612));
#36797=CARTESIAN_POINT('Ctrl Pts',(21.0330824745289,-39.1017118879348,-5.91572199049987));
#36798=CARTESIAN_POINT('Ctrl Pts',(21.9991307790699,-40.6166651990075,-7.69376028688717));
#36799=CARTESIAN_POINT('Ctrl Pts',(22.5567852866068,-41.5351982120271,-8.41063186549458));
#36800=CARTESIAN_POINT('Ctrl Pts',(23.7511065841813,-43.5504294726429,-9.37059840627156));
#36801=CARTESIAN_POINT('Ctrl Pts',(24.3935165949966,-44.6525338708106,-9.62435378636601));
#36802=CARTESIAN_POINT('Ctrl Pts',(25.025062629217,-45.7374214437733,-9.62320046360548));
#36803=CARTESIAN_POINT('Ctrl Pts',(17.9434360021525,-35.9854902185573,1.47293201877993));
#36804=CARTESIAN_POINT('Ctrl Pts',(17.9712842340237,-35.9463021021765,1.01538097970665));
#36805=CARTESIAN_POINT('Ctrl Pts',(17.9972930238881,-35.8985773174066,0.528580753652916));
#36806=CARTESIAN_POINT('Ctrl Pts',(18.1506662116866,-35.8297588571569,-1.5540287545432));
#36807=CARTESIAN_POINT('Ctrl Pts',(18.3899895327298,-36.0565601177377,-3.10121432121015));
#36808=CARTESIAN_POINT('Ctrl Pts',(19.1152999068282,-37.0372859924681,-5.9812914545338));
#36809=CARTESIAN_POINT('Ctrl Pts',(19.592231806385,-37.7840034012006,-7.29389406577903));
#36810=CARTESIAN_POINT('Ctrl Pts',(20.7330727614825,-39.6794872875133,-9.49113593802749));
#36811=CARTESIAN_POINT('Ctrl Pts',(21.3902415598918,-40.8208685319424,-10.3708286016693));
#36812=CARTESIAN_POINT('Ctrl Pts',(22.8168789076759,-43.3372861226379,-11.5604045561727));
#36813=CARTESIAN_POINT('Ctrl Pts',(23.5745664063873,-44.6978537235901,-11.8694761542189));
#36814=CARTESIAN_POINT('Ctrl Pts',(24.3313073348065,-46.0542245204215,-11.8687142284812));
#36815=CARTESIAN_POINT('Ctrl Pts',(16.6854562787119,-33.9789464595044,1.5964707761033));
#36816=CARTESIAN_POINT('Ctrl Pts',(16.7124723847588,-33.9409293131124,1.15259170142612));
#36817=CARTESIAN_POINT('Ctrl Pts',(16.7380701329864,-33.8890125875568,0.635573044868113));
#36818=CARTESIAN_POINT('Ctrl Pts',(16.8929361804822,-33.8192589011466,-1.86858636170883));
#36819=CARTESIAN_POINT('Ctrl Pts',(17.1543030075107,-34.1010104999082,-3.71029995866542));
#36820=CARTESIAN_POINT('Ctrl Pts',(17.981868110501,-35.297774448411,-7.16936247496945));
#36821=CARTESIAN_POINT('Ctrl Pts',(18.5280220223185,-36.2012418527466,-8.73699595771779));
#36822=CARTESIAN_POINT('Ctrl Pts',(19.8519402484503,-38.4952930132141,-11.3730256982018));
#36823=CARTESIAN_POINT('Ctrl Pts',(20.6132138377593,-39.8698068705739,-12.4235805191845));
#36824=CARTESIAN_POINT('Ctrl Pts',(22.2832067363974,-42.9112302679887,-13.8529470821977));
#36825=CARTESIAN_POINT('Ctrl Pts',(23.161511634173,-44.5422787457915,-14.2204718557262));
#36826=CARTESIAN_POINT('Ctrl Pts',(24.0493774600887,-46.1829520838075,-14.2198708430667));
#36827=CARTESIAN_POINT('Ctrl Pts',(14.5197073364539,-34.968659268658,1.5967437334527));
#36828=CARTESIAN_POINT('Ctrl Pts',(14.5467143347417,-34.9306549387484,1.15301430092464));
#36829=CARTESIAN_POINT('Ctrl Pts',(14.5722625852684,-34.8785972821207,0.635579150051368));
#36830=CARTESIAN_POINT('Ctrl Pts',(14.7263938532288,-34.8072346530974,-1.86860431096307));
#36831=CARTESIAN_POINT('Ctrl Pts',(14.9888871348065,-35.0914531001455,-3.70979114469921));
#36832=CARTESIAN_POINT('Ctrl Pts',(15.8151951687831,-36.2854639040137,-7.17014261469621));
#36833=CARTESIAN_POINT('Ctrl Pts',(16.3621201810157,-37.1906201278862,-8.73670574472927));
#36834=CARTESIAN_POINT('Ctrl Pts',(17.6857598217302,-39.4840611441579,-11.3734544105357));
#36835=CARTESIAN_POINT('Ctrl Pts',(18.4474896114359,-40.8595741643688,-12.4221714958517));
#36836=CARTESIAN_POINT('Ctrl Pts',(20.1169735923001,-43.8998828704052,-13.854590909534));
#36837=CARTESIAN_POINT('Ctrl Pts',(20.9956349952846,-45.5316698260234,-14.2195188099104));
#36838=CARTESIAN_POINT('Ctrl Pts',(21.8833834324342,-47.1721284105874,-14.2201291128084));
#36839=CARTESIAN_POINT('Ctrl Pts',(15.2134465003397,-37.2330519862578,1.47327608945396));
#36840=CARTESIAN_POINT('Ctrl Pts',(15.2412832516114,-37.1938800254387,1.0159136786583));
#36841=CARTESIAN_POINT('Ctrl Pts',(15.2672296481897,-37.1459775929453,0.528588449413895));
#36842=CARTESIAN_POINT('Ctrl Pts',(15.4196766250218,-37.0751310137469,-1.55405138009996));
#36843=CARTESIAN_POINT('Ctrl Pts',(15.6604198747747,-37.3050418083239,-3.10057294641483));
#36844=CARTESIAN_POINT('Ctrl Pts',(16.3841456768324,-38.2822972641882,-5.98227484333796));
#36845=CARTESIAN_POINT('Ctrl Pts',(16.8620495708872,-39.0311434790522,-7.29352824387148));
#36846=CARTESIAN_POINT('Ctrl Pts',(18.002539360956,-40.925858260867,-9.49167634238626));
#36847=CARTESIAN_POINT('Ctrl Pts',(18.6602832132299,-42.0684989791172,-10.3690524867973));
#36848=CARTESIAN_POINT('Ctrl Pts',(20.0862790553718,-44.5835114689251,-11.5624766483172));
#36849=CARTESIAN_POINT('Ctrl Pts',(20.8444200112022,-45.9450085199817,-11.8682745704784));
#36850=CARTESIAN_POINT('Ctrl Pts',(21.6010088957266,-47.301110036494,-11.8690397849987));
#36851=CARTESIAN_POINT('Ctrl Pts',(15.4515482289397,-39.5896190563863,1.35541228259766));
#36852=CARTESIAN_POINT('Ctrl Pts',(15.4801756476595,-39.5493344659312,0.885059075360922));
#36853=CARTESIAN_POINT('Ctrl Pts',(15.5064925913678,-39.505372844223,0.426408585766831));
#36854=CARTESIAN_POINT('Ctrl Pts',(15.6571869876725,-39.434703790117,-1.25364232217367));
#36855=CARTESIAN_POINT('Ctrl Pts',(15.8773787191569,-39.6132317302722,-2.51864171290804));
#36856=CARTESIAN_POINT('Ctrl Pts',(16.5028873873922,-40.3829362474817,-4.84795915804603));
#36857=CARTESIAN_POINT('Ctrl Pts',(16.9150240490585,-40.9828301658884,-5.9151702046228));
#36858=CARTESIAN_POINT('Ctrl Pts',(17.880542675362,-42.496623401559,-7.69457540344039));
#36859=CARTESIAN_POINT('Ctrl Pts',(18.4390645628778,-43.4170561363982,-8.40795287039259));
#36860=CARTESIAN_POINT('Ctrl Pts',(19.6324182482298,-45.4301680192512,-9.37372383739693));
#36861=CARTESIAN_POINT('Ctrl Pts',(20.2755208515495,-46.533671031965,-9.62254085992524));
#36862=CARTESIAN_POINT('Ctrl Pts',(20.9068289285804,-47.6181557545822,-9.62369151535379));
#36863=CARTESIAN_POINT('Ctrl Pts',(15.2248621479926,-41.9477963710449,1.24768188077453));
#36864=CARTESIAN_POINT('Ctrl Pts',(15.254210762862,-41.9064969112026,0.765479302038377));
#36865=CARTESIAN_POINT('Ctrl Pts',(15.2808564144573,-41.8661102394704,0.33296638484066));
#36866=CARTESIAN_POINT('Ctrl Pts',(15.4297972934209,-41.7952733633443,-0.978922014777797));
#36867=CARTESIAN_POINT('Ctrl Pts',(15.6314258258188,-41.9273179171776,-1.98636136657411));
#36868=CARTESIAN_POINT('Ctrl Pts',(16.1668569942704,-42.5066521964322,-3.81078790530298));
#36869=CARTESIAN_POINT('Ctrl Pts',(16.5190077785595,-42.9706758457974,-4.65460264908077));
#36870=CARTESIAN_POINT('Ctrl Pts',(17.3244581615362,-44.1359912383599,-6.05121512495203));
#36871=CARTESIAN_POINT('Ctrl Pts',(17.7923352090986,-44.8534198776545,-6.61423873307417));
#36872=CARTESIAN_POINT('Ctrl Pts',(18.772833279635,-46.4073150662578,-7.37244739479018));
#36873=CARTESIAN_POINT('Ctrl Pts',(19.3108003965517,-47.275034523802,-7.56862230160965));
#36874=CARTESIAN_POINT('Ctrl Pts',(19.8275212310755,-48.1110813316864,-7.57037421505997));
#36875=CARTESIAN_POINT('Ctrl Pts',(11.6799141290245,-36.0076777827442,1.59647068126611));
#36876=CARTESIAN_POINT('Ctrl Pts',(11.7120656519303,-35.9738923911144,1.15259163659876));
#36877=CARTESIAN_POINT('Ctrl Pts',(11.7447913705197,-35.9261470465052,0.635573001855381));
#36878=CARTESIAN_POINT('Ctrl Pts',(11.9080080866776,-35.8791430893826,-1.86858636178463));
#36879=CARTESIAN_POINT('Ctrl Pts',(12.1266171429838,-36.1952232408468,-3.71029995873377));
#36880=CARTESIAN_POINT('Ctrl Pts',(12.7754415589391,-37.4975806516859,-7.16936247490142));
#36881=CARTESIAN_POINT('Ctrl Pts',(13.1874595938576,-38.4695778662026,-8.73699595770811));
#36882=CARTESIAN_POINT('Ctrl Pts',(14.1714247213063,-40.9286921018315,-11.3730256982117));
#36883=CARTESIAN_POINT('Ctrl Pts',(14.7293359257928,-42.3975559178223,-12.4235805192562));
#36884=CARTESIAN_POINT('Ctrl Pts',(15.9494910259804,-45.645686779583,-13.8529470821261));
#36885=CARTESIAN_POINT('Ctrl Pts',(16.5867336458242,-47.3851293552256,-14.2204718557262));
#36886=CARTESIAN_POINT('Ctrl Pts',(17.2320701170938,-49.1354594857183,-14.2198708430667));
#36887=CARTESIAN_POINT('Ctrl Pts',(10.8171551228315,-35.6055008474197,1.6296461228737));
#36888=CARTESIAN_POINT('Ctrl Pts',(10.8490384138683,-35.5719973186181,1.18947024665146));
#36889=CARTESIAN_POINT('Ctrl Pts',(10.8818072974792,-35.5230856250726,0.664243958035779));
#36890=CARTESIAN_POINT('Ctrl Pts',(11.0453235253478,-35.4754406456448,-1.95287905128153));
#36891=CARTESIAN_POINT('Ctrl Pts',(11.2678861931429,-35.8076256583718,-3.87337387082083));
#36892=CARTESIAN_POINT('Ctrl Pts',(11.9353671582668,-37.170412338562,-7.48792130210496));
#36893=CARTESIAN_POINT('Ctrl Pts',(12.3599059968312,-38.1870962603733,-9.12360836232141));
#36894=CARTESIAN_POINT('Ctrl Pts',(13.3771794921622,-40.758733259042,-11.8774049927098));
#36895=CARTESIAN_POINT('Ctrl Pts',(13.9538940421623,-42.2936801020862,-12.9732563609012));
#36896=CARTESIAN_POINT('Ctrl Pts',(15.2184820529382,-45.6900265604125,-14.4676858045336));
#36897=CARTESIAN_POINT('Ctrl Pts',(15.8774655646438,-47.5060156561953,-14.8501851005531));
#36898=CARTESIAN_POINT('Ctrl Pts',(16.5467173899495,-49.3366907261821,-14.8499483202528));
#36899=CARTESIAN_POINT('Ctrl Pts',(9.90333289917165,-35.8740691471583,1.62975530581346));
#36900=CARTESIAN_POINT('Ctrl Pts',(9.93521185458921,-35.840570174317,1.18963928644335));
#36901=CARTESIAN_POINT('Ctrl Pts',(9.96796916328224,-35.7915998643985,0.664246400104493));
#36902=CARTESIAN_POINT('Ctrl Pts',(10.1312860615024,-35.7432760306242,-1.95288623097023));
#36903=CARTESIAN_POINT('Ctrl Pts',(10.354154297206,-36.0765018635817,-3.87317034521659));
#36904=CARTESIAN_POINT('Ctrl Pts',(11.0212942781007,-37.4381269352451,-7.48823335801339));
#36905=CARTESIAN_POINT('Ctrl Pts',(11.446042279729,-38.4555234045924,-9.12349227713555));
#36906=CARTESIAN_POINT('Ctrl Pts',(12.4632402081669,-41.0269029710472,-11.8775764776338));
#36907=CARTESIAN_POINT('Ctrl Pts',(13.0400785026582,-42.5622713808391,-12.9726927515287));
#36908=CARTESIAN_POINT('Ctrl Pts',(14.3045284731933,-45.9581475303539,-14.4683433355075));
#36909=CARTESIAN_POINT('Ctrl Pts',(14.9636108093825,-47.7744493566741,-14.8498038984862));
#36910=CARTESIAN_POINT('Ctrl Pts',(15.6328286697383,-49.6050326655026,-14.8500516281495));
#36911=CARTESIAN_POINT('Ctrl Pts',(9.39535856987488,-36.6790985320905,1.59674363861551));
#36912=CARTESIAN_POINT('Ctrl Pts',(9.42749925373743,-36.6453245303473,1.15301423607977));
#36913=CARTESIAN_POINT('Ctrl Pts',(9.46019603502518,-36.5974326448213,0.635579107027166));
#36914=CARTESIAN_POINT('Ctrl Pts',(9.62291442707024,-36.5487315518261,-1.86860431100636));
#36915=CARTESIAN_POINT('Ctrl Pts',(9.8422874031409,-36.8674137538596,-3.70979114472798));
#36916=CARTESIAN_POINT('Ctrl Pts',(10.4902593585244,-38.1668671434055,-7.17014261466771));
#36917=CARTESIAN_POINT('Ctrl Pts',(10.9028003010987,-39.1406457267576,-8.73670574474347));
#36918=CARTESIAN_POINT('Ctrl Pts',(11.8865765113215,-41.5991163818375,-11.3734544105217));
#36919=CARTESIAN_POINT('Ctrl Pts',(12.4447970770368,-43.0690341146998,-12.4221714958274));
#36920=CARTESIAN_POINT('Ctrl Pts',(13.6646070766139,-46.3159892044412,-13.8545909095583));
#36921=CARTESIAN_POINT('Ctrl Pts',(14.3020974766102,-48.0562134772786,-14.2195188098913));
#36922=CARTESIAN_POINT('Ctrl Pts',(14.9473483165659,-49.8063143340195,-14.2201291128083));
#36923=CARTESIAN_POINT('Ctrl Pts',(11.7862169042728,-35.9142171164212,0.));
#36924=CARTESIAN_POINT('Ctrl Pts',(11.9080080866776,-35.8791430893826,-1.86858636178463));
#36925=CARTESIAN_POINT('Ctrl Pts',(12.1266171429838,-36.1952232408468,-3.71029995873257));
#36926=CARTESIAN_POINT('Ctrl Pts',(12.7754415589391,-37.4975806516859,-7.16936247490261));
#36927=CARTESIAN_POINT('Ctrl Pts',(13.1874595938576,-38.4695778662026,-8.73699595770572));
#36928=CARTESIAN_POINT('Ctrl Pts',(13.7294890038888,-39.8242114819216,-10.1890856763496));
#36929=CARTESIAN_POINT('Ctrl Pts',(13.7802180759825,-39.9517643117901,-10.3203928635163));
#36930=CARTESIAN_POINT('Ctrl Pts',(13.8316148870825,-40.0817049410147,-10.4488603765993));
#36931=CARTESIAN_POINT('Ctrl Pts',(9.50149509066468,-36.5850719698906,-1.49880108324396E-15));
#36932=CARTESIAN_POINT('Ctrl Pts',(9.62291442707024,-36.5487315518261,-1.86860431100636));
#36933=CARTESIAN_POINT('Ctrl Pts',(9.8422874031409,-36.8674137538596,-3.70979114472798));
#36934=CARTESIAN_POINT('Ctrl Pts',(10.4902593585244,-38.1668671434055,-7.17014261466771));
#36935=CARTESIAN_POINT('Ctrl Pts',(10.9028003010987,-39.1406457267576,-8.73670574474347));
#36936=CARTESIAN_POINT('Ctrl Pts',(11.447491770971,-40.5018374092138,-10.1966053555721));
#36937=CARTESIAN_POINT('Ctrl Pts',(11.5010595286631,-40.6365673070921,-10.3350231942278));
#36938=CARTESIAN_POINT('Ctrl Pts',(11.5553735590044,-40.7739629732814,-10.4702558450999));
#36939=CARTESIAN_POINT('Ctrl Pts',(15.7201209119704,-41.7419576204998,1.24689082988543));
#36940=CARTESIAN_POINT('Ctrl Pts',(15.7550797324069,-41.7052222707071,0.764254661705176));
#36941=CARTESIAN_POINT('Ctrl Pts',(15.7872856429791,-41.6694633881789,0.332948671129717));
#36942=CARTESIAN_POINT('Ctrl Pts',(15.9462356620245,-41.6254618648069,-0.978870002708));
#36943=CARTESIAN_POINT('Ctrl Pts',(16.124806376022,-41.7773170936442,-1.9878357708918));
#36944=CARTESIAN_POINT('Ctrl Pts',(16.5748099612742,-42.4353694480507,-3.80852727283301));
#36945=CARTESIAN_POINT('Ctrl Pts',(16.855823663794,-42.939624365945,-4.65544360722247));
#36946=CARTESIAN_POINT('Ctrl Pts',(17.4877814824343,-44.2095709903027,-6.04997283343079));
#36947=CARTESIAN_POINT('Ctrl Pts',(17.8478990309574,-44.9832291227579,-6.61832169904376));
#36948=CARTESIAN_POINT('Ctrl Pts',(18.5982747097764,-46.6642543902711,-7.36768403077276));
#36949=CARTESIAN_POINT('Ctrl Pts',(19.0065156677573,-47.597447725177,-7.57138648702772));
#36950=CARTESIAN_POINT('Ctrl Pts',(19.3992863750335,-48.4991757443116,-7.56962581969437));
#36951=CARTESIAN_POINT('Ctrl Pts',(14.0037398626871,-40.1090570584214,1.35489321026543));
#36952=CARTESIAN_POINT('Ctrl Pts',(14.0378295966279,-40.0732349601815,0.884255518285286));
#36953=CARTESIAN_POINT('Ctrl Pts',(14.0701900799508,-40.0337447201333,0.426396949026514));
#36954=CARTESIAN_POINT('Ctrl Pts',(14.2303553472453,-39.9884678119657,-1.25360819501712));
#36955=CARTESIAN_POINT('Ctrl Pts',(14.4214462185236,-40.191567831885,-2.51960912780892));
#36956=CARTESIAN_POINT('Ctrl Pts',(14.9326685312488,-41.0479784867153,-4.84647586781181));
#36957=CARTESIAN_POINT('Ctrl Pts',(15.2542422185937,-41.6970325717334,-5.91572199047102));
#36958=CARTESIAN_POINT('Ctrl Pts',(15.9948572088741,-43.3340488505992,-7.69376028691602));
#36959=CARTESIAN_POINT('Ctrl Pts',(16.4161147204243,-44.3225950330452,-8.41063186558551));
#36960=CARTESIAN_POINT('Ctrl Pts',(17.3114822382606,-46.487283787507,-9.37059840618065));
#36961=CARTESIAN_POINT('Ctrl Pts',(17.7905076322893,-47.6695948287687,-9.62435378637549));
#36962=CARTESIAN_POINT('Ctrl Pts',(18.2612298390044,-48.8333181822475,-9.62320046360547));
#36963=CARTESIAN_POINT('Ctrl Pts',(12.6395284821794,-38.1728270004197,1.47293192394286));
#36964=CARTESIAN_POINT('Ctrl Pts',(12.6726703074,-38.1380009815193,1.0153809158411));
#36965=CARTESIAN_POINT('Ctrl Pts',(12.7052063084752,-38.0944634070469,0.528580717871503));
#36966=CARTESIAN_POINT('Ctrl Pts',(12.8668122636039,-38.0481727007019,-1.55402875457849));
#36967=CARTESIAN_POINT('Ctrl Pts',(13.0714224335629,-38.3067247111899,-3.10121432125906));
#36968=CARTESIAN_POINT('Ctrl Pts',(13.6497783497158,-39.3806906392206,-5.98129145448502));
#36969=CARTESIAN_POINT('Ctrl Pts',(14.0155868029404,-40.187682027567,-7.29389406575976));
#36970=CARTESIAN_POINT('Ctrl Pts',(14.8750601592654,-42.2262312169631,-9.49113593804686));
#36971=CARTESIAN_POINT('Ctrl Pts',(15.3631044396506,-43.4495197173632,-10.370828601741));
#36972=CARTESIAN_POINT('Ctrl Pts',(16.4170971139165,-46.1433554687416,-11.560404556101));
#36973=CARTESIAN_POINT('Ctrl Pts',(16.9734434882197,-47.5979046271707,-11.8694761542236));
#36974=CARTESIAN_POINT('Ctrl Pts',(17.5294501945609,-49.0481649878424,-11.8687142284812));
#36975=CARTESIAN_POINT('Ctrl Pts',(11.6799141290245,-36.0076777827442,1.59647068126611));
#36976=CARTESIAN_POINT('Ctrl Pts',(11.7120656519303,-35.9738923911144,1.15259163659876));
#36977=CARTESIAN_POINT('Ctrl Pts',(11.7447913705197,-35.9261470465052,0.635573001855381));
#36978=CARTESIAN_POINT('Ctrl Pts',(11.9080080866776,-35.8791430893826,-1.86858636178463));
#36979=CARTESIAN_POINT('Ctrl Pts',(12.1266171429838,-36.1952232408468,-3.71029995873257));
#36980=CARTESIAN_POINT('Ctrl Pts',(12.7754415589391,-37.4975806516859,-7.16936247490261));
#36981=CARTESIAN_POINT('Ctrl Pts',(13.1874595938576,-38.4695778662026,-8.73699595770572));
#36982=CARTESIAN_POINT('Ctrl Pts',(14.1714247213063,-40.9286921018316,-11.3730256982141));
#36983=CARTESIAN_POINT('Ctrl Pts',(14.7293359257928,-42.3975559178223,-12.4235805192514));
#36984=CARTESIAN_POINT('Ctrl Pts',(15.9494910259804,-45.645686779583,-13.8529470821309));
#36985=CARTESIAN_POINT('Ctrl Pts',(16.5867336458133,-47.3851293552296,-14.2204718557262));
#36986=CARTESIAN_POINT('Ctrl Pts',(17.2320701170938,-49.1354594857183,-14.2198708430667));
#36987=CARTESIAN_POINT('Ctrl Pts',(9.39535856987487,-36.6790985320905,1.59674363861551));
#36988=CARTESIAN_POINT('Ctrl Pts',(9.42749925373742,-36.6453245303473,1.15301423607977));
#36989=CARTESIAN_POINT('Ctrl Pts',(9.46019603502516,-36.5974326448213,0.635579107027166));
#36990=CARTESIAN_POINT('Ctrl Pts',(9.62291442707023,-36.5487315518261,-1.86860431100636));
#36991=CARTESIAN_POINT('Ctrl Pts',(9.84228740314089,-36.8674137538596,-3.70979114472798));
#36992=CARTESIAN_POINT('Ctrl Pts',(10.4902593585244,-38.1668671434055,-7.17014261466771));
#36993=CARTESIAN_POINT('Ctrl Pts',(10.9028003010999,-39.1406457267528,-8.73670574474347));
#36994=CARTESIAN_POINT('Ctrl Pts',(11.8865765113203,-41.5991163818423,-11.3734544105217));
#36995=CARTESIAN_POINT('Ctrl Pts',(12.4447970770392,-43.069034114695,-12.4221714958274));
#36996=CARTESIAN_POINT('Ctrl Pts',(13.6646070766115,-46.3159892044461,-13.8545909095583));
#36997=CARTESIAN_POINT('Ctrl Pts',(14.3020974766134,-48.0562134772745,-14.2195188098913));
#36998=CARTESIAN_POINT('Ctrl Pts',(14.9473483165659,-49.8063143340195,-14.2201291128083));
#36999=CARTESIAN_POINT('Ctrl Pts',(9.75977978596898,-39.0191723737221,1.47327599461687));
#37000=CARTESIAN_POINT('Ctrl Pts',(9.79290794825892,-38.9843607121039,1.0159136147723));
#37001=CARTESIAN_POINT('Ctrl Pts',(9.82540747302648,-38.9406384185465,0.528588413618024));
#37002=CARTESIAN_POINT('Ctrl Pts',(9.98638527612132,-38.8922084230982,-1.55405138009428));
#37003=CARTESIAN_POINT('Ctrl Pts',(10.1919583891532,-39.154040393972,-3.10057294641215));
#37004=CARTESIAN_POINT('Ctrl Pts',(10.7692397539741,-40.2243457187397,-5.9822748433407));
#37005=CARTESIAN_POINT('Ctrl Pts',(11.1357073475001,-41.033582574293,-7.29352824388565));
#37006=CARTESIAN_POINT('Ctrl Pts',(11.9949425681694,-43.07132051169,-9.49167634237209));
#37007=CARTESIAN_POINT('Ctrl Pts',(12.4833768073745,-44.295937504943,-10.369052486749));
#37008=CARTESIAN_POINT('Ctrl Pts',(13.5369344722939,-46.9882911615219,-11.5624766483653));
#37009=CARTESIAN_POINT('Ctrl Pts',(14.0935974136572,-48.4438248433017,-11.8682745704593));
#37010=CARTESIAN_POINT('Ctrl Pts',(14.6494919462604,-49.8937970264263,-11.8690397849987));
#37011=CARTESIAN_POINT('Ctrl Pts',(9.6600835208205,-41.385638397964,1.35541218776066));
#37012=CARTESIAN_POINT('Ctrl Pts',(9.69415264633907,-41.3498379554702,0.885059012386701));
#37013=CARTESIAN_POINT('Ctrl Pts',(9.72645811078361,-41.3100690951929,0.426408556872093));
#37014=CARTESIAN_POINT('Ctrl Pts',(9.88567590770692,-41.2615653996831,-1.25364232211483));
#37015=CARTESIAN_POINT('Ctrl Pts',(10.0782192299531,-41.4696127334993,-2.51864171286793));
#37016=CARTESIAN_POINT('Ctrl Pts',(10.587820747883,-42.3205019333899,-4.847959158086));
#37017=CARTESIAN_POINT('Ctrl Pts',(10.9103886466144,-42.9729429590446,-5.9151702046465));
#37018=CARTESIAN_POINT('Ctrl Pts',(11.6506444460221,-44.6087355895318,-7.69457540341655));
#37019=CARTESIAN_POINT('Ctrl Pts',(12.0724901502524,-45.5992855983477,-8.40795287032041));
#37020=CARTESIAN_POINT('Ctrl Pts',(12.9672015236417,-47.7617388416025,-9.37372383746897));
#37021=CARTESIAN_POINT('Ctrl Pts',(13.446713417008,-48.9455328277857,-9.62254085987295));
#37022=CARTESIAN_POINT('Ctrl Pts',(13.9172574201599,-50.1088235664896,-9.62369151535376));
#37023=CARTESIAN_POINT('Ctrl Pts',(9.10010115416748,-43.6875520748215,1.24768178593761));
#37024=CARTESIAN_POINT('Ctrl Pts',(9.13502856600687,-43.6508497298264,0.76547923989595));
#37025=CARTESIAN_POINT('Ctrl Pts',(9.16715062416417,-43.6146662116234,0.332966362254671));
#37026=CARTESIAN_POINT('Ctrl Pts',(9.32465663565536,-43.5657468507608,-0.978922014663684));
#37027=CARTESIAN_POINT('Ctrl Pts',(9.50544098106106,-43.7251421134196,-1.9863613664906));
#37028=CARTESIAN_POINT('Ctrl Pts',(9.95297436776755,-44.3747794050744,-3.81078790538617));
#37029=CARTESIAN_POINT('Ctrl Pts',(10.2355033142436,-44.8841962446728,-4.65460264910923));
#37030=CARTESIAN_POINT('Ctrl Pts',(10.8669137022235,-46.1522779478823,-6.0512151249233));
#37031=CARTESIAN_POINT('Ctrl Pts',(11.2279276953183,-46.9289900443738,-6.61423873295882));
#37032=CARTESIAN_POINT('Ctrl Pts',(11.9773033665753,-48.6066082448324,-7.37244739490529));
#37033=CARTESIAN_POINT('Ctrl Pts',(12.3863053997921,-49.5420562727077,-7.5686223015431));
#37034=CARTESIAN_POINT('Ctrl Pts',(12.7787848949961,-50.4431303715412,-7.57037421505993));
#37035=CARTESIAN_POINT('Ctrl Pts',(6.43660260973332,-37.3033966274915,1.59647061166181));
#37036=CARTESIAN_POINT('Ctrl Pts',(6.44564064573105,-37.2962747755321,1.48695576755787));
#37037=CARTESIAN_POINT('Ctrl Pts',(6.45467756855567,-37.2891542935595,1.37746396776832));
#37038=CARTESIAN_POINT('Ctrl Pts',(6.49319539523223,-37.2588006588781,0.91069863508483));
#37039=CARTESIAN_POINT('Ctrl Pts',(6.52244162562218,-37.2305413795555,0.486448413028126));
#37040=CARTESIAN_POINT('Ctrl Pts',(6.68066728816074,-37.2086313911891,-1.86858636176938));
#37041=CARTESIAN_POINT('Ctrl Pts',(6.85206832383191,-37.5526056149563,-3.71029995872546));
#37042=CARTESIAN_POINT('Ctrl Pts',(7.30894385843816,-38.934044247035,-7.16936247490972));
#37043=CARTESIAN_POINT('Ctrl Pts',(7.57843851746451,-39.9547842114019,-8.73699595769907));
#37044=CARTESIAN_POINT('Ctrl Pts',(8.20241985394517,-42.5289010478592,-11.3730256982207));
#37045=CARTESIAN_POINT('Ctrl Pts',(8.54561121045842,-44.0622129909516,-12.423580519233));
#37046=CARTESIAN_POINT('Ctrl Pts',(9.29108967262444,-47.4509287397228,-13.8529470821493));
#37047=CARTESIAN_POINT('Ctrl Pts',(9.67429759303427,-49.2633553783165,-14.2204718555978));
#37048=CARTESIAN_POINT('Ctrl Pts',(10.0639675197015,-51.0877106274639,-14.2198708430667));
#37049=CARTESIAN_POINT('Ctrl Pts',(5.63986099173555,-36.7825298650421,1.62964605326942));
#37050=CARTESIAN_POINT('Ctrl Pts',(5.64889912474545,-36.77540793664,1.52013003366147));
#37051=CARTESIAN_POINT('Ctrl Pts',(5.65793595641857,-36.7682876225861,1.41064098633233));
#37052=CARTESIAN_POINT('Ctrl Pts',(5.69645375811678,-36.7379335980319,0.943868932617261));
#37053=CARTESIAN_POINT('Ctrl Pts',(5.72562619436981,-36.7087318569752,0.508392298457236));
#37054=CARTESIAN_POINT('Ctrl Pts',(5.88421645976751,-36.6862652424053,-1.95287905126922));
#37055=CARTESIAN_POINT('Ctrl Pts',(6.05723890413859,-37.0467430607592,-3.87337387081251));
#37056=CARTESIAN_POINT('Ctrl Pts',(6.52398110944683,-38.4906509831273,-7.48792130211325));
#37057=CARTESIAN_POINT('Ctrl Pts',(6.79950954687151,-39.5574047046894,-9.12360836231237));
#37058=CARTESIAN_POINT('Ctrl Pts',(7.44044656125075,-42.2476392596962,-11.8774049927188));
#37059=CARTESIAN_POINT('Ctrl Pts',(7.79284527703385,-43.8490375949744,-12.9732563608828));
#37060=CARTESIAN_POINT('Ctrl Pts',(8.56121110815365,-47.3907837817508,-14.4676858045521));
#37061=CARTESIAN_POINT('Ctrl Pts',(8.95504492393713,-49.2820718587611,-14.8501851004818));
#37062=CARTESIAN_POINT('Ctrl Pts',(9.35695250368037,-51.1893577615277,-14.8499483202528));
#37063=CARTESIAN_POINT('Ctrl Pts',(4.69711890654707,-36.9183140647621,1.62975523620918));
#37064=CARTESIAN_POINT('Ctrl Pts',(4.70615704022186,-36.9111921358362,1.52023920855111));
#37065=CARTESIAN_POINT('Ctrl Pts',(4.71519387290942,-36.9040718339574,1.41075017948988));
#37066=CARTESIAN_POINT('Ctrl Pts',(4.7537116674503,-36.8737177597449,0.943978082226359));
#37067=CARTESIAN_POINT('Ctrl Pts',(4.78287005804029,-36.8444185781148,0.508394167544101));
#37068=CARTESIAN_POINT('Ctrl Pts',(4.94136562987512,-36.8212933555072,-1.95288623096214));
#37069=CARTESIAN_POINT('Ctrl Pts',(5.11454240774922,-37.1828448868836,-3.87317034521066));
#37070=CARTESIAN_POINT('Ctrl Pts',(5.58111241368669,-38.6255544971264,-7.48823335801928));
#37071=CARTESIAN_POINT('Ctrl Pts',(5.8567464791066,-39.6930432805223,-9.1234922771265));
#37072=CARTESIAN_POINT('Ctrl Pts',(6.49764533218352,-42.3830122693035,-11.8775764776428));
#37073=CARTESIAN_POINT('Ctrl Pts',(6.85010653771311,-43.9848454910638,-12.9726927515343));
#37074=CARTESIAN_POINT('Ctrl Pts',(7.61840266556165,-47.5261065109322,-14.4683433355019));
#37075=CARTESIAN_POINT('Ctrl Pts',(8.01228979375816,-49.417718199511,-14.8498038985623));
#37076=CARTESIAN_POINT('Ctrl Pts',(8.4141768132259,-51.3249084414064,-14.8500516281495));
#37077=CARTESIAN_POINT('Ctrl Pts',(4.07974739676214,-37.6428571267913,1.59674356901121));
#37078=CARTESIAN_POINT('Ctrl Pts',(4.08878543442164,-37.6357352735241,1.48722870478182));
#37079=CARTESIAN_POINT('Ctrl Pts',(4.09782235978292,-37.6286148219883,1.37773695066217));
#37080=CARTESIAN_POINT('Ctrl Pts',(4.13634016856563,-37.5982610631587,0.910971509107631));
#37081=CARTESIAN_POINT('Ctrl Pts',(4.16555128479877,-37.5697581824064,0.486453085745287));
#37082=CARTESIAN_POINT('Ctrl Pts',(4.32354021342829,-37.5462016739366,-1.86860431100168));
#37083=CARTESIAN_POINT('Ctrl Pts',(4.4953270828591,-37.8928601802674,-3.70979114472205));
#37084=CARTESIAN_POINT('Ctrl Pts',(4.95177211903725,-39.2713030320329,-7.1701426146736));
#37085=CARTESIAN_POINT('Ctrl Pts',(5.22153084805404,-40.2938806509769,-8.73670574474158));
#37086=CARTESIAN_POINT('Ctrl Pts',(5.84541678127528,-42.8673335718846,-11.3734544105235));
#37087=CARTESIAN_POINT('Ctrl Pts',(6.18876436215572,-44.4017327311633,-12.4221714958474));
#37088=CARTESIAN_POINT('Ctrl Pts',(6.93406856614537,-47.7892355626883,-13.8545909095384));
#37089=CARTESIAN_POINT('Ctrl Pts',(7.31741049756817,-49.6024712046744,-14.2195188100245));
#37090=CARTESIAN_POINT('Ctrl Pts',(7.70702829356537,-51.4265873271607,-14.2201291128084));
#37091=CARTESIAN_POINT('Ctrl Pts',(6.55512420987355,-37.2260157227863,0.));
#37092=CARTESIAN_POINT('Ctrl Pts',(6.68066728816073,-37.2086313911891,-1.86858636176938));
#37093=CARTESIAN_POINT('Ctrl Pts',(6.85206832383192,-37.5526056149563,-3.71029995872546));
#37094=CARTESIAN_POINT('Ctrl Pts',(7.30894385843816,-38.934044247035,-7.16936247490972));
#37095=CARTESIAN_POINT('Ctrl Pts',(7.57843851746451,-39.9547842114019,-8.73699595769907));
#37096=CARTESIAN_POINT('Ctrl Pts',(7.92216638570706,-41.3727684379704,-10.1890856763497));
#37097=CARTESIAN_POINT('Ctrl Pts',(7.95422644863896,-41.5062424636377,-10.3203928635162));
#37098=CARTESIAN_POINT('Ctrl Pts',(7.98660763467823,-41.642175013475,-10.4488603765986));
#37099=CARTESIAN_POINT('Ctrl Pts',(4.198184970543,-37.5648924254994,-4.877668582392E-9));
#37100=CARTESIAN_POINT('Ctrl Pts',(4.32354021386282,-37.5462016743808,-1.86860431422771));
#37101=CARTESIAN_POINT('Ctrl Pts',(4.49532708316823,-37.8928601807419,-3.70979114625979));
#37102=CARTESIAN_POINT('Ctrl Pts',(4.72354960103335,-38.5820816060563,-5.4399668797283));
#37103=CARTESIAN_POINT('Ctrl Pts',(4.95177211909771,-39.2713030319724,-7.17014261470724));
#37104=CARTESIAN_POINT('Ctrl Pts',(5.22153084808902,-40.2938806509466,-8.73670574476508));
#37105=CARTESIAN_POINT('Ctrl Pts',(5.53347381467321,-41.5806071114236,-10.0550800776385));
#37106=CARTESIAN_POINT('Ctrl Pts',(5.56696037000555,-41.7187350432317,-10.196605355576));
#37107=CARTESIAN_POINT('Ctrl Pts',(5.60080882153369,-41.8597170717893,-10.3350231942299));
#37108=CARTESIAN_POINT('Ctrl Pts',(5.63501657134591,-42.0034439406511,-10.4702558451003));
#37109=CARTESIAN_POINT('Ctrl Pts',(9.61961280540157,-43.5542911395533,1.24689076028094));
#37110=CARTESIAN_POINT('Ctrl Pts',(9.62864982106753,-43.5471700916028,1.13738827963977));
#37111=CARTESIAN_POINT('Ctrl Pts',(9.63768771167183,-43.5400479046461,1.02786752738893));
#37112=CARTESIAN_POINT('Ctrl Pts',(9.67620576232687,-43.509698109946,0.561172897473927));
#37113=CARTESIAN_POINT('Ctrl Pts',(9.70615305455088,-43.4908467778853,0.254828874441861));
#37114=CARTESIAN_POINT('Ctrl Pts',(9.86000510220678,-43.4711606313058,-0.978870002685296));
#37115=CARTESIAN_POINT('Ctrl Pts',(10.0151469714872,-43.6468834551436,-1.9878357708895));
#37116=CARTESIAN_POINT('Ctrl Pts',(10.3669195547086,-44.3622799728645,-3.80852727283542));
#37117=CARTESIAN_POINT('Ctrl Pts',(10.5733099858207,-44.9013947224069,-4.65544360722759));
#37118=CARTESIAN_POINT('Ctrl Pts',(11.0181031366371,-46.2483520959844,-6.04997283342579));
#37119=CARTESIAN_POINT('Ctrl Pts',(11.2644521757028,-47.0653855748928,-6.61832169899626));
#37120=CARTESIAN_POINT('Ctrl Pts',(11.767955273083,-48.8360900223252,-7.36768403082038));
#37121=CARTESIAN_POINT('Ctrl Pts',(12.0392336678346,-49.817883540689,-7.57138648665654));
#37122=CARTESIAN_POINT('Ctrl Pts',(12.2996772587575,-50.7663303683513,-7.56962581969443));
#37123=CARTESIAN_POINT('Ctrl Pts',(8.15308801979152,-41.6937446593045,1.354893140661));
#37124=CARTESIAN_POINT('Ctrl Pts',(8.16212535086541,-41.6866233628175,1.24538683819019));
#37125=CARTESIAN_POINT('Ctrl Pts',(8.17116294315093,-41.6795017085853,1.13587503550903));
#37126=CARTESIAN_POINT('Ctrl Pts',(8.20968092097156,-41.649150702668,0.669158551024819));
#37127=CARTESIAN_POINT('Ctrl Pts',(8.23940452738148,-41.6273443121243,0.32635136887054));
#37128=CARTESIAN_POINT('Ctrl Pts',(8.39455851883134,-41.6066335880765,-1.25360819499889));
#37129=CARTESIAN_POINT('Ctrl Pts',(8.55480021408119,-41.8348614090738,-2.5196091278042));
#37130=CARTESIAN_POINT('Ctrl Pts',(8.93893907695026,-42.7553095590252,-4.84647586781658));
#37131=CARTESIAN_POINT('Ctrl Pts',(9.16486958068117,-43.4435219166315,-5.91572199046901));
#37132=CARTESIAN_POINT('Ctrl Pts',(9.66497447127398,-45.1692762327225,-7.69376028691809));
#37133=CARTESIAN_POINT('Ctrl Pts',(9.94125939865908,-46.2077116350436,-8.41063186554769));
#37134=CARTESIAN_POINT('Ctrl Pts',(10.5194460362019,-48.4777910626699,-9.37059840621854));
#37135=CARTESIAN_POINT('Ctrl Pts',(10.8253352376655,-49.7162403038184,-9.62435378615668));
#37136=CARTESIAN_POINT('Ctrl Pts',(11.1256510703081,-50.9351093861918,-9.62320046360551));
#37137=CARTESIAN_POINT('Ctrl Pts',(7.07831661167153,-39.5830751094924,1.47293185433849));
#37138=CARTESIAN_POINT('Ctrl Pts',(7.08735428726966,-39.5759535415238,1.36342137723571));
#37139=CARTESIAN_POINT('Ctrl Pts',(7.09639155277543,-39.5688324629961,1.25391935060785));
#37140=CARTESIAN_POINT('Ctrl Pts',(7.13490945496847,-39.5384801604726,0.787178992711653));
#37141=CARTESIAN_POINT('Ctrl Pts',(7.16439634167976,-39.5134970937345,0.404559744694547));
#37142=CARTESIAN_POINT('Ctrl Pts',(7.32102712268645,-39.4920354699275,-1.55402875456277));
#37143=CARTESIAN_POINT('Ctrl Pts',(7.48675886857651,-39.7770748569936,-3.10121432125195));
#37144=CARTESIAN_POINT('Ctrl Pts',(7.90638666805501,-40.9224179890928,-5.98129145449216));
#37145=CARTESIAN_POINT('Ctrl Pts',(8.15362486975768,-41.7732553395465,-7.29389406576022));
#37146=CARTESIAN_POINT('Ctrl Pts',(8.71423422838196,-43.9133708492413,-9.49113593804644));
#37147=CARTESIAN_POINT('Ctrl Pts',(9.02321881661921,-45.1936639793806,-10.3708286017129));
#37148=CARTESIAN_POINT('Ctrl Pts',(9.68311056585015,-48.0100791639764,-11.5604045561292));
#37149=CARTESIAN_POINT('Ctrl Pts',(10.0267902081664,-49.5289994535186,-11.8694761540572));
#37150=CARTESIAN_POINT('Ctrl Pts',(10.370743999114,-51.0436262593386,-11.8687142284812));
#37151=CARTESIAN_POINT('Ctrl Pts',(6.43660260973332,-37.3033966274915,1.59647061166181));
#37152=CARTESIAN_POINT('Ctrl Pts',(6.44564064573105,-37.2962747755321,1.48695576755787));
#37153=CARTESIAN_POINT('Ctrl Pts',(6.45467756855567,-37.2891542935595,1.37746396776832));
#37154=CARTESIAN_POINT('Ctrl Pts',(6.49319539523223,-37.2588006588781,0.91069863508483));
#37155=CARTESIAN_POINT('Ctrl Pts',(6.52244162562218,-37.2305413795555,0.486448413028126));
#37156=CARTESIAN_POINT('Ctrl Pts',(6.68066728816074,-37.2086313911891,-1.86858636176938));
#37157=CARTESIAN_POINT('Ctrl Pts',(6.85206832383192,-37.5526056149563,-3.71029995872546));
#37158=CARTESIAN_POINT('Ctrl Pts',(7.30894385843816,-38.934044247035,-7.16936247490972));
#37159=CARTESIAN_POINT('Ctrl Pts',(7.57843851746451,-39.9547842114019,-8.73699595769907));
#37160=CARTESIAN_POINT('Ctrl Pts',(8.20241985394517,-42.5289010478592,-11.3730256982207));
#37161=CARTESIAN_POINT('Ctrl Pts',(8.54561121045842,-44.0622129909516,-12.4235805192282));
#37162=CARTESIAN_POINT('Ctrl Pts',(9.29108967262445,-47.4509287397228,-13.8529470821541));
#37163=CARTESIAN_POINT('Ctrl Pts',(9.67429759302972,-49.2633553783174,-14.2204718555978));
#37164=CARTESIAN_POINT('Ctrl Pts',(10.0639675197015,-51.0877106274639,-14.2198708430667));
#37165=CARTESIAN_POINT('Ctrl Pts',(4.07974739676214,-37.6428571267913,1.59674356901121));
#37166=CARTESIAN_POINT('Ctrl Pts',(4.08878543442164,-37.6357352735241,1.48722870478183));
#37167=CARTESIAN_POINT('Ctrl Pts',(4.09782235978292,-37.6286148219883,1.37773695066217));
#37168=CARTESIAN_POINT('Ctrl Pts',(4.13634016856563,-37.5982610631587,0.910971509107631));
#37169=CARTESIAN_POINT('Ctrl Pts',(4.16555128479876,-37.5697581824064,0.486453085745287));
#37170=CARTESIAN_POINT('Ctrl Pts',(4.32354021342829,-37.5462016739366,-1.86860431100168));
#37171=CARTESIAN_POINT('Ctrl Pts',(4.4953270828591,-37.8928601802674,-3.70979114472325));
#37172=CARTESIAN_POINT('Ctrl Pts',(4.95177211903725,-39.2713030320329,-7.1701426146724));
#37173=CARTESIAN_POINT('Ctrl Pts',(5.22153084805404,-40.2938806509721,-8.73670574473919));
#37174=CARTESIAN_POINT('Ctrl Pts',(5.84541678127527,-42.8673335718894,-11.3734544105259));
#37175=CARTESIAN_POINT('Ctrl Pts',(6.18876436215512,-44.4017327311681,-12.4221714958474));
#37176=CARTESIAN_POINT('Ctrl Pts',(6.93406856614598,-47.7892355626836,-13.8545909095384));
#37177=CARTESIAN_POINT('Ctrl Pts',(7.31741049756717,-49.6024712046782,-14.2195188100435));
#37178=CARTESIAN_POINT('Ctrl Pts',(7.70702829356537,-51.4265873271607,-14.2201291128084));
#37179=CARTESIAN_POINT('Ctrl Pts',(4.10743210000891,-40.0109749372547,1.47327592501252));
#37180=CARTESIAN_POINT('Ctrl Pts',(4.1164697777016,-40.0038533676368,1.36376542254105));
#37181=CARTESIAN_POINT('Ctrl Pts',(4.12550704640513,-39.9967323274759,1.25426345348145));
#37182=CARTESIAN_POINT('Ctrl Pts',(4.16402492604217,-39.9663798684617,0.787522958349925));
#37183=CARTESIAN_POINT('Ctrl Pts',(4.19346755033784,-39.9410897350393,0.40456563479037));
#37184=CARTESIAN_POINT('Ctrl Pts',(4.34979992137194,-39.9175526247724,-1.55405138009188));
#37185=CARTESIAN_POINT('Ctrl Pts',(4.51601802193031,-40.2059756280632,-3.10057294641101));
#37186=CARTESIAN_POINT('Ctrl Pts',(4.93510316562684,-41.3475424919559,-5.98227484334182));
#37187=CARTESIAN_POINT('Ctrl Pts',(5.18267423522826,-42.200696259442,-7.29352824388607));
#37188=CARTESIAN_POINT('Ctrl Pts',(5.74316333527085,-44.3399748842863,-9.49167634237164));
#37189=CARTESIAN_POINT('Ctrl Pts',(6.05234484886441,-45.6216384820368,-10.3690524867785));
#37190=CARTESIAN_POINT('Ctrl Pts',(6.71201694059813,-48.4365247491788,-11.5624766483359));
#37191=CARTESIAN_POINT('Ctrl Pts',(7.05586981550236,-49.9564645931953,-11.8682745706448));
#37192=CARTESIAN_POINT('Ctrl Pts',(7.3997535864146,-51.4707901907297,-11.8690397849987));
#37193=CARTESIAN_POINT('Ctrl Pts',(3.67196736957011,-42.3391654916811,1.35541211815626));
#37194=CARTESIAN_POINT('Ctrl Pts',(3.68100470380343,-42.3320441927047,1.24590577742079));
#37195=CARTESIAN_POINT('Ctrl Pts',(3.69004230091196,-42.3249225963454,1.1363940615723));
#37196=CARTESIAN_POINT('Ctrl Pts',(3.72856024471116,-42.2945713543822,0.669677370090017));
#37197=CARTESIAN_POINT('Ctrl Pts',(3.75821708810019,-42.2723018011526,0.326360253170795));
#37198=CARTESIAN_POINT('Ctrl Pts',(3.91292097417106,-42.2484605261848,-1.25364232211669));
#37199=CARTESIAN_POINT('Ctrl Pts',(4.07389626035863,-42.4817920098941,-2.51864171287277));
#37200=CARTESIAN_POINT('Ctrl Pts',(4.45721661075379,-43.39654424225,-4.84795915808115));
#37201=CARTESIAN_POINT('Ctrl Pts',(4.68364919432174,-44.0882505573296,-5.91517020464685));
#37202=CARTESIAN_POINT('Ctrl Pts',(5.18357269341173,-45.8127425618315,-7.6945754034162));
#37203=CARTESIAN_POINT('Ctrl Pts',(5.46015465229401,-46.8532451029695,-8.40795287035928));
#37204=CARTESIAN_POINT('Ctrl Pts',(6.03800997041407,-49.1210183946462,-9.37372383743011));
#37205=CARTESIAN_POINT('Ctrl Pts',(6.34416967429075,-50.3610047224884,-9.62254086013458));
#37206=CARTESIAN_POINT('Ctrl Pts',(6.64437068472131,-51.5794202324977,-9.62369151535376));
#37207=CARTESIAN_POINT('Ctrl Pts',(2.79008834334054,-44.5379552064474,1.24768171633317));
#37208=CARTESIAN_POINT('Ctrl Pts',(2.79912536382142,-44.530834154704,1.13817917737408));
#37209=CARTESIAN_POINT('Ctrl Pts',(2.8081632617768,-44.5237120559476,1.02865855746206));
#37210=CARTESIAN_POINT('Ctrl Pts',(2.84668126057998,-44.4933619015011,0.56196361206819));
#37211=CARTESIAN_POINT('Ctrl Pts',(2.8765268015416,-44.473804678848,0.254842414703475));
#37212=CARTESIAN_POINT('Ctrl Pts',(3.02969285881099,-44.449347365471,-0.978922014671594));
#37213=CARTESIAN_POINT('Ctrl Pts',(3.18595276923174,-44.632848509077,-1.98636136649783));
#37214=CARTESIAN_POINT('Ctrl Pts',(3.53647788527045,-45.3395640713789,-3.81078790537893));
#37215=CARTESIAN_POINT('Ctrl Pts',(3.74363351928522,-45.8840038433848,-4.65460264911906));
#37216=CARTESIAN_POINT('Ctrl Pts',(4.18815021744348,-47.2290373705203,-6.05121512491345));
#37217=CARTESIAN_POINT('Ctrl Pts',(4.43495195217142,-48.0492213058189,-6.61423873300717));
#37218=CARTESIAN_POINT('Ctrl Pts',(4.93795009682242,-49.8164110494284,-7.37244739485694));
#37219=CARTESIAN_POINT('Ctrl Pts',(5.2096609439022,-50.8005446234324,-7.56862230191897));
#37220=CARTESIAN_POINT('Ctrl Pts',(5.46990934942727,-51.7483027430073,-7.57037421505991));
#37221=CARTESIAN_POINT('',(0.,0.,0.));
#37222=CARTESIAN_POINT('Origin',(46.,55.1862915010152,2.));
#37223=CARTESIAN_POINT('',(46.,66.5,-2.));
#37224=CARTESIAN_POINT('Origin',(46.,66.5,2.));
#37225=CARTESIAN_POINT('',(46.,76.5,-2.));
#37226=CARTESIAN_POINT('',(46.,55.1862915010152,-2.));
#37227=CARTESIAN_POINT('Origin',(46.,76.5,2.));
#37228=CARTESIAN_POINT('Origin',(42.0000000000001,-56.5,14.5));
#37229=CARTESIAN_POINT('',(46.0000000000001,-56.5,-14.5));
#37230=CARTESIAN_POINT('Origin',(42.,-56.5,-14.5));
#37231=CARTESIAN_POINT('',(46.0000000000001,-56.5,-24.5));
#37232=CARTESIAN_POINT('',(46.0000000000001,-56.5,14.5));
#37233=CARTESIAN_POINT('Origin',(42.,-56.5,-24.5));
#37234=CARTESIAN_POINT('Origin',(-62.,46.68,-3.68653347947321));
#37235=CARTESIAN_POINT('',(52.,46.68,-6.18653347947322));
#37236=CARTESIAN_POINT('Origin',(52.,46.68,-3.68653347947321));
#37237=CARTESIAN_POINT('',(62.,46.68,-6.18653347947322));
#37238=CARTESIAN_POINT('',(-62.,46.68,-6.18653347947322));
#37239=CARTESIAN_POINT('Origin',(62.,46.68,-3.68653347947321));
#37240=CARTESIAN_POINT('Origin',(-62.,25.68,-3.68653347947321));
#37241=CARTESIAN_POINT('',(52.,25.68,-6.18653347947322));
#37242=CARTESIAN_POINT('Origin',(52.,25.68,-3.68653347947321));
#37243=CARTESIAN_POINT('',(62.,25.68,-6.18653347947322));
#37244=CARTESIAN_POINT('',(-62.,25.68,-6.18653347947322));
#37245=CARTESIAN_POINT('Origin',(62.,25.68,-3.68653347947321));
#37246=CARTESIAN_POINT('Origin',(-62.,46.68,-3.68653347947321));
#37247=CARTESIAN_POINT('',(-62.,46.68,-6.18653347947322));
#37248=CARTESIAN_POINT('Origin',(-62.,46.68,-3.68653347947321));
#37249=CARTESIAN_POINT('',(-52.,46.68,-6.18653347947322));
#37250=CARTESIAN_POINT('',(-62.,46.68,-6.18653347947322));
#37251=CARTESIAN_POINT('Origin',(-52.,46.68,-3.68653347947321));
#37252=CARTESIAN_POINT('Origin',(-62.,25.68,-3.68653347947321));
#37253=CARTESIAN_POINT('',(-62.,25.68,-6.18653347947322));
#37254=CARTESIAN_POINT('Origin',(-62.,25.68,-3.68653347947321));
#37255=CARTESIAN_POINT('',(-52.,25.68,-6.18653347947322));
#37256=CARTESIAN_POINT('',(-62.,25.68,-6.18653347947322));
#37257=CARTESIAN_POINT('Origin',(-52.,25.68,-3.68653347947321));
#37258=CARTESIAN_POINT('Origin',(-26.3106350946109,-8.00000000000001,-14.5));
#37259=CARTESIAN_POINT('',(-29.3106350946109,-8.00000000000001,-14.5));
#37260=CARTESIAN_POINT('Origin',(-26.3106350946109,-8.00000000000001,-14.5));
#37261=CARTESIAN_POINT('',(-29.3106350946109,-8.00000000000001,-24.5));
#37262=CARTESIAN_POINT('',(-29.3106350946109,-8.00000000000001,-14.5));
#37263=CARTESIAN_POINT('Origin',(-26.3106350946109,-8.00000000000001,-24.5));
#37264=CARTESIAN_POINT('Origin',(-26.3106350946109,-33.,-14.5));
#37265=CARTESIAN_POINT('',(-29.3106350946109,-33.,-14.5));
#37266=CARTESIAN_POINT('Origin',(-26.3106350946109,-33.,-14.5));
#37267=CARTESIAN_POINT('',(-29.3106350946109,-33.,-24.5));
#37268=CARTESIAN_POINT('',(-29.3106350946109,-33.,-14.5));
#37269=CARTESIAN_POINT('Origin',(-26.3106350946109,-33.,-24.5));
#37270=CARTESIAN_POINT('Origin',(-4.66,-45.5,-14.5));
#37271=CARTESIAN_POINT('',(-7.66000000000001,-45.5,-14.5));
#37272=CARTESIAN_POINT('Origin',(-4.66,-45.5,-14.5));
#37273=CARTESIAN_POINT('',(-7.66000000000001,-45.5,-24.5));
#37274=CARTESIAN_POINT('',(-7.66000000000001,-45.5,-14.5));
#37275=CARTESIAN_POINT('Origin',(-4.66,-45.5,-24.5));
#37276=CARTESIAN_POINT('Origin',(16.990635094611,-33.,-14.5));
#37277=CARTESIAN_POINT('',(13.990635094611,-33.,-14.5));
#37278=CARTESIAN_POINT('Origin',(16.990635094611,-33.,-14.5));
#37279=CARTESIAN_POINT('',(13.990635094611,-33.,-24.5));
#37280=CARTESIAN_POINT('',(13.990635094611,-33.,-14.5));
#37281=CARTESIAN_POINT('Origin',(16.990635094611,-33.,-24.5));
#37282=CARTESIAN_POINT('Origin',(16.990635094611,-8.00000000000001,-14.5));
#37283=CARTESIAN_POINT('',(13.990635094611,-8.00000000000001,-14.5));
#37284=CARTESIAN_POINT('Origin',(16.990635094611,-8.00000000000001,-14.5));
#37285=CARTESIAN_POINT('',(13.990635094611,-8.00000000000001,-24.5));
#37286=CARTESIAN_POINT('',(13.990635094611,-8.00000000000001,-14.5));
#37287=CARTESIAN_POINT('Origin',(16.990635094611,-8.00000000000001,-24.5));
#37288=CARTESIAN_POINT('Origin',(-4.66,4.49999999999999,-14.5));
#37289=CARTESIAN_POINT('',(-7.66,4.49999999999999,-14.5));
#37290=CARTESIAN_POINT('Origin',(-4.66,4.49999999999999,-14.5));
#37291=CARTESIAN_POINT('',(-7.66,4.49999999999999,-24.5));
#37292=CARTESIAN_POINT('',(-7.66,4.49999999999999,-14.5));
#37293=CARTESIAN_POINT('Origin',(-4.66,4.49999999999999,-24.5));
#37294=CARTESIAN_POINT('Origin',(-4.66,-20.5,-14.5));
#37295=CARTESIAN_POINT('',(-22.16,-20.5,-14.5));
#37296=CARTESIAN_POINT('Origin',(-4.66,-20.5,-14.5));
#37297=CARTESIAN_POINT('',(-22.16,-20.5,-24.5));
#37298=CARTESIAN_POINT('',(-22.16,-20.5,-14.5));
#37299=CARTESIAN_POINT('Origin',(-4.66,-20.5,-24.5));
#37300=CARTESIAN_POINT('Origin',(0.,0.,14.5));
#37301=CARTESIAN_POINT('',(-61.9999999999999,59.68,14.5));
#37302=CARTESIAN_POINT('',(-51.9999999999999,59.68,14.5));
#37303=CARTESIAN_POINT('',(-61.9999999999999,59.68,14.5));
#37304=CARTESIAN_POINT('',(-51.9999999999999,66.5,14.5));
#37305=CARTESIAN_POINT('',(-51.9999999999999,-66.5,14.5));
#37306=CARTESIAN_POINT('',(52.0000000000001,66.5,14.5));
#37307=CARTESIAN_POINT('',(-51.9999999999999,66.5,14.5));
#37308=CARTESIAN_POINT('',(52.0000000000001,59.68,14.5));
#37309=CARTESIAN_POINT('',(52.0000000000001,-66.5,14.5));
#37310=CARTESIAN_POINT('',(62.0000000000001,59.68,14.5));
#37311=CARTESIAN_POINT('',(-61.9999999999999,59.68,14.5));
#37312=CARTESIAN_POINT('',(62.0000000000001,76.5,14.5));
#37313=CARTESIAN_POINT('',(62.0000000000001,-76.5,14.5));
#37314=CARTESIAN_POINT('',(-61.9999999999999,76.5,14.5));
#37315=CARTESIAN_POINT('',(-61.9999999999999,76.5,14.5));
#37316=CARTESIAN_POINT('',(-61.9999999999999,-76.5,14.5));
#37317=CARTESIAN_POINT('Origin',(0.,0.,14.5));
#37318=CARTESIAN_POINT('',(62.0000000000001,54.68,14.5));
#37319=CARTESIAN_POINT('',(52.0000000000001,54.68,14.5));
#37320=CARTESIAN_POINT('',(-61.9999999999999,54.68,14.5));
#37321=CARTESIAN_POINT('',(52.0000000000001,53.68,14.5));
#37322=CARTESIAN_POINT('',(52.0000000000001,-66.5,14.5));
#37323=CARTESIAN_POINT('',(62.0000000000001,53.68,14.5));
#37324=CARTESIAN_POINT('',(-61.9999999999999,53.68,14.5));
#37325=CARTESIAN_POINT('',(62.0000000000001,-76.5,14.5));
#37326=CARTESIAN_POINT('Origin',(0.,0.,14.5));
#37327=CARTESIAN_POINT('',(52.0000000000001,17.68,14.5));
#37328=CARTESIAN_POINT('',(62.0000000000001,17.68,14.5));
#37329=CARTESIAN_POINT('',(-61.9999999999999,17.68,14.5));
#37330=CARTESIAN_POINT('',(62.0000000000001,18.68,14.5));
#37331=CARTESIAN_POINT('',(62.0000000000001,-76.5,14.5));
#37332=CARTESIAN_POINT('',(52.0000000000001,18.68,14.5));
#37333=CARTESIAN_POINT('',(-61.9999999999999,18.68,14.5));
#37334=CARTESIAN_POINT('',(52.0000000000001,-66.5,14.5));
#37335=CARTESIAN_POINT('Origin',(0.,0.,14.5));
#37336=CARTESIAN_POINT('',(-61.9999999999999,17.68,14.5));
#37337=CARTESIAN_POINT('',(-51.9999999999999,17.68,14.5));
#37338=CARTESIAN_POINT('',(-61.9999999999999,17.68,14.5));
#37339=CARTESIAN_POINT('',(-51.9999999999999,18.68,14.5));
#37340=CARTESIAN_POINT('',(-51.9999999999999,-66.5,14.5));
#37341=CARTESIAN_POINT('',(-61.9999999999999,18.68,14.5));
#37342=CARTESIAN_POINT('',(-61.9999999999999,18.68,14.5));
#37343=CARTESIAN_POINT('',(-61.9999999999999,-76.5,14.5));
#37344=CARTESIAN_POINT('Origin',(0.,0.,14.5));
#37345=CARTESIAN_POINT('',(-51.9999999999999,54.68,14.5));
#37346=CARTESIAN_POINT('',(-61.9999999999999,54.68,14.5));
#37347=CARTESIAN_POINT('',(-61.9999999999999,54.68,14.5));
#37348=CARTESIAN_POINT('',(-61.9999999999999,53.68,14.5));
#37349=CARTESIAN_POINT('',(-61.9999999999999,-76.5,14.5));
#37350=CARTESIAN_POINT('',(-51.9999999999999,53.68,14.5));
#37351=CARTESIAN_POINT('',(-61.9999999999999,53.68,14.5));
#37352=CARTESIAN_POINT('',(-51.9999999999999,-66.5,14.5));
#37353=CARTESIAN_POINT('Origin',(62.,-76.5,-14.5));
#37354=CARTESIAN_POINT('',(62.,76.5,-21.5));
#37355=CARTESIAN_POINT('',(62.,76.5,-14.5));
#37356=CARTESIAN_POINT('Origin',(62.0000000000001,57.18,14.5));
#37357=CARTESIAN_POINT('Origin',(62.0000000000001,36.18,14.5));
#37358=CARTESIAN_POINT('',(62.0000000000001,12.68,14.5));
#37359=CARTESIAN_POINT('Origin',(62.0000000000001,15.18,14.5));
#37360=CARTESIAN_POINT('',(62.0000000000001,-76.5,14.5));
#37361=CARTESIAN_POINT('',(62.0000000000001,-76.5,14.5));
#37362=CARTESIAN_POINT('',(62.,-76.5,-21.5));
#37363=CARTESIAN_POINT('',(62.,-76.5,-14.5));
#37364=CARTESIAN_POINT('',(62.,-76.5,-21.5));
#37365=CARTESIAN_POINT('Origin',(0.,0.,14.5));
#37366=CARTESIAN_POINT('',(52.0000000000001,12.68,14.5));
#37367=CARTESIAN_POINT('',(-61.9999999999999,12.68,14.5));
#37368=CARTESIAN_POINT('',(52.0000000000001,-66.5,14.5));
#37369=CARTESIAN_POINT('',(52.0000000000001,-66.5,14.5));
#37370=CARTESIAN_POINT('',(-51.9999999999999,-66.5,14.5));
#37371=CARTESIAN_POINT('',(-51.9999999999999,-66.5,14.5));
#37372=CARTESIAN_POINT('',(-51.9999999999999,12.68,14.5));
#37373=CARTESIAN_POINT('',(-51.9999999999999,-66.5,14.5));
#37374=CARTESIAN_POINT('',(-61.9999999999999,12.68,14.5));
#37375=CARTESIAN_POINT('',(-61.9999999999999,12.68,14.5));
#37376=CARTESIAN_POINT('',(-61.9999999999999,-76.5,14.5));
#37377=CARTESIAN_POINT('',(-61.9999999999999,-76.5,14.5));
#37378=CARTESIAN_POINT('',(-61.9999999999999,-76.5,14.5));
#37379=CARTESIAN_POINT('Origin',(-62.,-76.5,-14.5));
#37380=CARTESIAN_POINT('',(-62.,-76.5,-21.5));
#37381=CARTESIAN_POINT('',(-62.,-76.5,-14.5));
#37382=CARTESIAN_POINT('Origin',(-61.9999999999999,15.18,14.5));
#37383=CARTESIAN_POINT('Origin',(-61.9999999999999,36.18,14.5));
#37384=CARTESIAN_POINT('Origin',(-61.9999999999999,57.18,14.5));
#37385=CARTESIAN_POINT('',(-62.,76.5,-21.5));
#37386=CARTESIAN_POINT('',(-62.,76.5,-14.5));
#37387=CARTESIAN_POINT('',(-62.,76.5,-21.5));
#37388=CARTESIAN_POINT('Origin',(-62.,-76.5,-14.5));
#37389=CARTESIAN_POINT('',(-62.,-76.5,-21.5));
#37390=CARTESIAN_POINT('Origin',(-62.,76.5,-14.5));
#37391=CARTESIAN_POINT('',(62.,76.5,-21.5));
#37392=CARTESIAN_POINT('Origin',(52.,-66.5,-14.5));
#37393=CARTESIAN_POINT('Origin',(52.0000000000001,57.18,14.5));
#37394=CARTESIAN_POINT('',(52.,66.5,-14.5));
#37395=CARTESIAN_POINT('',(52.,66.5,-14.5));
#37396=CARTESIAN_POINT('',(52.,-66.5,-14.5));
#37397=CARTESIAN_POINT('',(52.,-66.5,-14.5));
#37398=CARTESIAN_POINT('',(52.,-66.5,-14.5));
#37399=CARTESIAN_POINT('Origin',(52.0000000000001,15.18,14.5));
#37400=CARTESIAN_POINT('Origin',(52.0000000000001,36.18,14.5));
#37401=CARTESIAN_POINT('Origin',(-52.,66.5,-14.5));
#37402=CARTESIAN_POINT('',(-52.,66.5,-14.5));
#37403=CARTESIAN_POINT('',(-52.,66.5,-14.5));
#37404=CARTESIAN_POINT('',(-52.,66.5,-14.5));
#37405=CARTESIAN_POINT('Origin',(-52.,-66.5,-14.5));
#37406=CARTESIAN_POINT('Origin',(-51.9999999999999,57.18,14.5));
#37407=CARTESIAN_POINT('Origin',(-51.9999999999999,36.18,14.5));
#37408=CARTESIAN_POINT('Origin',(-51.9999999999999,15.18,14.5));
#37409=CARTESIAN_POINT('',(-52.,-66.5,-14.5));
#37410=CARTESIAN_POINT('',(-52.,-66.5,-14.5));
#37411=CARTESIAN_POINT('',(-52.,-66.5,-14.5));
#37412=CARTESIAN_POINT('Origin',(-52.,-66.5,-14.5));
#37413=CARTESIAN_POINT('',(-52.,-66.5,-14.5));
#37414=CARTESIAN_POINT('Origin',(0.,0.,-14.5));
#37415=CARTESIAN_POINT('Origin',(0.,0.,-24.5));
#37416=CARTESIAN_POINT('',(59.,73.5,-24.5));
#37417=CARTESIAN_POINT('',(-59.,73.5,-24.5));
#37418=CARTESIAN_POINT('',(-62.,73.5,-24.5));
#37419=CARTESIAN_POINT('',(59.,-73.5,-24.5));
#37420=CARTESIAN_POINT('',(59.,76.5,-24.5));
#37421=CARTESIAN_POINT('',(-59.,-73.5,-24.5));
#37422=CARTESIAN_POINT('',(62.,-73.5,-24.5));
#37423=CARTESIAN_POINT('',(-59.,-76.5,-24.5));
#37424=CARTESIAN_POINT('Origin',(-61.9999999999999,36.18,14.5));
#37425=CARTESIAN_POINT('Origin',(-61.9999999999999,15.18,14.5));
#37426=CARTESIAN_POINT('Origin',(-61.9999999999999,57.18,14.5));
#37427=CARTESIAN_POINT('Origin',(-61.9999999999999,36.18,14.5));
#37428=CARTESIAN_POINT('Origin',(-61.9999999999999,15.18,14.5));
#37429=CARTESIAN_POINT('Origin',(-61.9999999999999,57.18,14.5));
#37430=CARTESIAN_POINT('Origin',(59.,0.,-21.5));
#37431=CARTESIAN_POINT('Origin',(59.0000000000003,-73.5000000000003,-21.5000000000003));
#37432=CARTESIAN_POINT('Origin',(59.0000000000012,73.5000000000012,-21.5000000000012));
#37433=CARTESIAN_POINT('Origin',(4.93038065763132E-29,73.5,-21.5));
#37434=CARTESIAN_POINT('Origin',(-59.0000000000004,73.5000000000004,-21.5000000000004));
#37435=CARTESIAN_POINT('Origin',(4.93038065763132E-29,-73.5,-21.5));
#37436=CARTESIAN_POINT('Origin',(-59.000000000001,-73.500000000001,-21.500000000001));
#37437=CARTESIAN_POINT('Origin',(-59.,0.,-21.5));
#37438=CARTESIAN_POINT('',(0.,0.,0.));
#37439=CARTESIAN_POINT('Origin',(4.9,-3.75,22.7));
#37440=CARTESIAN_POINT('',(4.9,-3.25,0.5));
#37441=CARTESIAN_POINT('',(4.9,3.25,0.5));
#37442=CARTESIAN_POINT('',(4.9,3.75,0.5));
#37443=CARTESIAN_POINT('',(4.9,3.25,22.2));
#37444=CARTESIAN_POINT('',(4.9,3.25,22.7));
#37445=CARTESIAN_POINT('',(4.9,-3.25,22.2));
#37446=CARTESIAN_POINT('',(4.9,-3.75,22.2));
#37447=CARTESIAN_POINT('',(4.9,-3.25,22.7));
#37448=CARTESIAN_POINT('Origin',(-4.9,3.75,22.7));
#37449=CARTESIAN_POINT('',(-4.4,3.75,22.2));
#37450=CARTESIAN_POINT('',(4.4,3.75,22.2));
#37451=CARTESIAN_POINT('',(-4.9,3.75,22.2));
#37452=CARTESIAN_POINT('',(4.4,3.75,0.5));
#37453=CARTESIAN_POINT('',(4.4,3.75,22.7));
#37454=CARTESIAN_POINT('',(-4.4,3.75,0.5));
#37455=CARTESIAN_POINT('',(-4.9,3.75,0.5));
#37456=CARTESIAN_POINT('',(-4.4,3.75,22.7));
#37457=CARTESIAN_POINT('Origin',(-4.9,-3.75,22.7));
#37458=CARTESIAN_POINT('',(-4.9,-3.25,22.2));
#37459=CARTESIAN_POINT('',(-4.9,3.25,22.2));
#37460=CARTESIAN_POINT('',(-4.9,-3.75,22.2));
#37461=CARTESIAN_POINT('',(-4.9,3.25,0.5));
#37462=CARTESIAN_POINT('',(-4.9,3.25,22.7));
#37463=CARTESIAN_POINT('',(-4.9,-3.25,0.5));
#37464=CARTESIAN_POINT('',(-4.9,-3.75,0.5));
#37465=CARTESIAN_POINT('',(-4.9,-3.25,22.7));
#37466=CARTESIAN_POINT('Origin',(-4.9,-3.75,22.7));
#37467=CARTESIAN_POINT('',(4.4,-3.75,22.2));
#37468=CARTESIAN_POINT('',(-4.4,-3.75,22.2));
#37469=CARTESIAN_POINT('',(-4.9,-3.75,22.2));
#37470=CARTESIAN_POINT('',(-4.4,-3.75,0.5));
#37471=CARTESIAN_POINT('',(-4.4,-3.75,22.7));
#37472=CARTESIAN_POINT('',(4.4,-3.75,0.5));
#37473=CARTESIAN_POINT('',(4.9,-3.75,0.5));
#37474=CARTESIAN_POINT('',(4.4,-3.75,22.7));
#37475=CARTESIAN_POINT('Origin',(0.,0.,22.7));
#37476=CARTESIAN_POINT('',(4.4,-3.25,22.7));
#37477=CARTESIAN_POINT('',(4.4,3.25,22.7));
#37478=CARTESIAN_POINT('',(4.4,0.,22.7));
#37479=CARTESIAN_POINT('',(-4.4,3.25,22.7));
#37480=CARTESIAN_POINT('',(0.,3.25,22.7));
#37481=CARTESIAN_POINT('',(-4.4,-3.25,22.7));
#37482=CARTESIAN_POINT('',(-4.4,0.,22.7));
#37483=CARTESIAN_POINT('',(1.43822737166444E-16,-3.25,22.7));
#37484=CARTESIAN_POINT('Origin',(0.,0.,0.));
#37485=CARTESIAN_POINT('',(-4.4,-3.25,0.));
#37486=CARTESIAN_POINT('',(-4.4,3.25,0.));
#37487=CARTESIAN_POINT('',(-4.4,3.75,0.));
#37488=CARTESIAN_POINT('',(4.4,3.25,0.));
#37489=CARTESIAN_POINT('',(4.9,3.25,0.));
#37490=CARTESIAN_POINT('',(4.4,-3.25,0.));
#37491=CARTESIAN_POINT('',(4.4,-3.75,0.));
#37492=CARTESIAN_POINT('',(-4.9,-3.25,0.));
#37493=CARTESIAN_POINT('Origin',(4.4,-3.75,0.5));
#37494=CARTESIAN_POINT('Origin',(4.4,3.25,0.5));
#37495=CARTESIAN_POINT('Origin',(4.4,-3.25,0.5));
#37496=CARTESIAN_POINT('Origin',(4.4,3.25,0.5));
#37497=CARTESIAN_POINT('Origin',(4.4,3.25,0.5));
#37498=CARTESIAN_POINT('Origin',(4.4,3.25,0.5));
#37499=CARTESIAN_POINT('Origin',(4.4,-3.25,0.5));
#37500=CARTESIAN_POINT('Origin',(4.4,-3.25,0.5));
#37501=CARTESIAN_POINT('Origin',(4.4,-3.25,0.5));
#37502=CARTESIAN_POINT('Origin',(-4.9,3.25,0.5));
#37503=CARTESIAN_POINT('Origin',(-4.4,3.25,0.5));
#37504=CARTESIAN_POINT('Origin',(4.4,3.25,22.7));
#37505=CARTESIAN_POINT('Origin',(4.4,3.25,22.2));
#37506=CARTESIAN_POINT('Origin',(4.4,0.,22.2));
#37507=CARTESIAN_POINT('Origin',(4.4,-3.25,22.2));
#37508=CARTESIAN_POINT('Origin',(4.4,3.25,22.2));
#37509=CARTESIAN_POINT('Origin',(4.4,-3.25,22.7));
#37510=CARTESIAN_POINT('Origin',(4.4,-3.25,22.2));
#37511=CARTESIAN_POINT('Origin',(-4.9,-3.25,0.5));
#37512=CARTESIAN_POINT('Origin',(-4.4,-3.25,0.5));
#37513=CARTESIAN_POINT('Origin',(-4.4,-3.75,0.5));
#37514=CARTESIAN_POINT('Origin',(-4.4,3.25,0.5));
#37515=CARTESIAN_POINT('Origin',(-4.4,-3.25,0.5));
#37516=CARTESIAN_POINT('Origin',(-4.4,3.25,0.5));
#37517=CARTESIAN_POINT('Origin',(-4.4,3.25,0.5));
#37518=CARTESIAN_POINT('Origin',(4.4,3.25,22.2));
#37519=CARTESIAN_POINT('Origin',(4.4,3.25,22.2));
#37520=CARTESIAN_POINT('Origin',(4.4,-3.25,22.2));
#37521=CARTESIAN_POINT('Origin',(4.4,-3.25,22.2));
#37522=CARTESIAN_POINT('Origin',(-4.4,-3.25,0.5));
#37523=CARTESIAN_POINT('Origin',(-4.4,-3.25,0.5));
#37524=CARTESIAN_POINT('Origin',(-4.4,3.25,22.7));
#37525=CARTESIAN_POINT('Origin',(-4.4,3.25,22.2));
#37526=CARTESIAN_POINT('Origin',(0.,3.25,22.2));
#37527=CARTESIAN_POINT('Origin',(-4.4,3.25,22.2));
#37528=CARTESIAN_POINT('Origin',(1.43822737166444E-16,-3.25,22.2));
#37529=CARTESIAN_POINT('Origin',(-4.4,-3.25,22.2));
#37530=CARTESIAN_POINT('Origin',(-4.4,-3.25,22.7));
#37531=CARTESIAN_POINT('Origin',(-4.4,-3.25,22.2));
#37532=CARTESIAN_POINT('Origin',(-4.4,3.25,22.2));
#37533=CARTESIAN_POINT('Origin',(-4.4,3.25,22.2));
#37534=CARTESIAN_POINT('Origin',(-4.4,-3.25,22.2));
#37535=CARTESIAN_POINT('Origin',(-4.4,-3.25,22.2));
#37536=CARTESIAN_POINT('Origin',(-4.4,0.,22.2));
#37537=CARTESIAN_POINT('',(0.,0.,0.));
#37538=CARTESIAN_POINT('Origin',(-21.650635094611,12.5,1.));
#37539=CARTESIAN_POINT('',(-18.650635094611,12.5,1.));
#37540=CARTESIAN_POINT('Origin',(-21.650635094611,12.5,1.));
#37541=CARTESIAN_POINT('',(-18.650635094611,12.5,-1.));
#37542=CARTESIAN_POINT('',(-18.650635094611,12.5,1.));
#37543=CARTESIAN_POINT('Origin',(-21.650635094611,12.5,-1.));
#37544=CARTESIAN_POINT('Origin',(-21.650635094611,-12.5,1.));
#37545=CARTESIAN_POINT('',(-18.650635094611,-12.5,1.));
#37546=CARTESIAN_POINT('Origin',(-21.650635094611,-12.5,1.));
#37547=CARTESIAN_POINT('',(-18.650635094611,-12.5,-1.));
#37548=CARTESIAN_POINT('',(-18.650635094611,-12.5,1.));
#37549=CARTESIAN_POINT('Origin',(-21.650635094611,-12.5,-1.));
#37550=CARTESIAN_POINT('Origin',(3.46944695195361E-15,-25.,1.));
#37551=CARTESIAN_POINT('',(3.,-25.,1.));
#37552=CARTESIAN_POINT('Origin',(3.46944695195361E-15,-25.,1.));
#37553=CARTESIAN_POINT('',(3.,-25.,-1.));
#37554=CARTESIAN_POINT('',(3.,-25.,1.));
#37555=CARTESIAN_POINT('Origin',(3.46944695195361E-15,-25.,-1.));
#37556=CARTESIAN_POINT('Origin',(21.650635094611,-12.5,1.));
#37557=CARTESIAN_POINT('',(24.650635094611,-12.5,1.));
#37558=CARTESIAN_POINT('Origin',(21.650635094611,-12.5,1.));
#37559=CARTESIAN_POINT('',(24.650635094611,-12.5,-1.));
#37560=CARTESIAN_POINT('',(24.650635094611,-12.5,1.));
#37561=CARTESIAN_POINT('Origin',(21.650635094611,-12.5,-1.));
#37562=CARTESIAN_POINT('Origin',(21.650635094611,12.5,1.));
#37563=CARTESIAN_POINT('',(24.650635094611,12.5,1.));
#37564=CARTESIAN_POINT('Origin',(21.650635094611,12.5,1.));
#37565=CARTESIAN_POINT('',(24.650635094611,12.5,-1.));
#37566=CARTESIAN_POINT('',(24.650635094611,12.5,1.));
#37567=CARTESIAN_POINT('Origin',(21.650635094611,12.5,-1.));
#37568=CARTESIAN_POINT('Origin',(0.,25.,1.));
#37569=CARTESIAN_POINT('',(3.,25.,1.));
#37570=CARTESIAN_POINT('Origin',(0.,25.,1.));
#37571=CARTESIAN_POINT('',(3.,25.,-1.));
#37572=CARTESIAN_POINT('',(3.,25.,1.));
#37573=CARTESIAN_POINT('Origin',(0.,25.,-1.));
#37574=CARTESIAN_POINT('Origin',(0.,0.,1.));
#37575=CARTESIAN_POINT('',(7.6,-9.30731567351989E-16,1.));
#37576=CARTESIAN_POINT('Origin',(0.,0.,1.));
#37577=CARTESIAN_POINT('',(7.6,-9.30731567351989E-16,-1.));
#37578=CARTESIAN_POINT('',(7.6,-9.30731567351989E-16,1.));
#37579=CARTESIAN_POINT('Origin',(0.,0.,-1.));
#37580=CARTESIAN_POINT('Origin',(0.,0.,1.));
#37581=CARTESIAN_POINT('',(30.,-3.67394039744206E-15,-1.));
#37582=CARTESIAN_POINT('Origin',(0.,0.,-1.));
#37583=CARTESIAN_POINT('',(30.,-3.67394039744206E-15,1.));
#37584=CARTESIAN_POINT('',(30.,-3.67394039744206E-15,1.));
#37585=CARTESIAN_POINT('Origin',(0.,0.,1.));
#37586=CARTESIAN_POINT('Origin',(0.,0.,1.));
#37587=CARTESIAN_POINT('Origin',(0.,0.,-1.));
#37588=CARTESIAN_POINT('',(0.,0.,0.));
#37589=CARTESIAN_POINT('Origin',(-18.1865334794732,10.5,1.));
#37590=CARTESIAN_POINT('',(-15.6865334794732,10.5,1.));
#37591=CARTESIAN_POINT('Origin',(-18.1865334794732,10.5,1.));
#37592=CARTESIAN_POINT('',(-15.6865334794732,10.5,-1.));
#37593=CARTESIAN_POINT('',(-15.6865334794732,10.5,1.));
#37594=CARTESIAN_POINT('Origin',(-18.1865334794732,10.5,-1.));
#37595=CARTESIAN_POINT('Origin',(-18.1865334794732,-10.5,1.));
#37596=CARTESIAN_POINT('',(-15.6865334794732,-10.5,1.));
#37597=CARTESIAN_POINT('Origin',(-18.1865334794732,-10.5,1.));
#37598=CARTESIAN_POINT('',(-15.6865334794732,-10.5,-1.));
#37599=CARTESIAN_POINT('',(-15.6865334794732,-10.5,1.));
#37600=CARTESIAN_POINT('Origin',(-18.1865334794732,-10.5,-1.));
#37601=CARTESIAN_POINT('Origin',(6.93889390390723E-15,-21.,1.));
#37602=CARTESIAN_POINT('',(2.50000000000001,-21.,1.));
#37603=CARTESIAN_POINT('Origin',(6.93889390390723E-15,-21.,1.));
#37604=CARTESIAN_POINT('',(2.50000000000001,-21.,-1.));
#37605=CARTESIAN_POINT('',(2.50000000000001,-21.,1.));
#37606=CARTESIAN_POINT('Origin',(6.93889390390723E-15,-21.,-1.));
#37607=CARTESIAN_POINT('Origin',(18.1865334794732,-10.5,1.));
#37608=CARTESIAN_POINT('',(20.6865334794732,-10.5,1.));
#37609=CARTESIAN_POINT('Origin',(18.1865334794732,-10.5,1.));
#37610=CARTESIAN_POINT('',(20.6865334794732,-10.5,-0.99999999999998));
#37611=CARTESIAN_POINT('',(20.6865334794732,-10.5,1.));
#37612=CARTESIAN_POINT('Origin',(18.1865334794732,-10.5,-0.99999999999998));
#37613=CARTESIAN_POINT('Origin',(18.1865334794732,10.5,1.));
#37614=CARTESIAN_POINT('',(20.6865334794732,10.5,1.));
#37615=CARTESIAN_POINT('Origin',(18.1865334794732,10.5,1.));
#37616=CARTESIAN_POINT('',(20.6865334794732,10.5,-0.99999999999998));
#37617=CARTESIAN_POINT('',(20.6865334794732,10.5,1.));
#37618=CARTESIAN_POINT('Origin',(18.1865334794732,10.5,-0.99999999999998));
#37619=CARTESIAN_POINT('Origin',(0.,21.,1.));
#37620=CARTESIAN_POINT('',(2.5,21.,1.));
#37621=CARTESIAN_POINT('Origin',(0.,21.,1.));
#37622=CARTESIAN_POINT('',(2.5,21.,-1.));
#37623=CARTESIAN_POINT('',(2.5,21.,1.));
#37624=CARTESIAN_POINT('Origin',(0.,21.,-1.));
#37625=CARTESIAN_POINT('Origin',(0.,0.,1.));
#37626=CARTESIAN_POINT('',(7.6,-9.30731567351989E-16,1.));
#37627=CARTESIAN_POINT('Origin',(0.,0.,1.));
#37628=CARTESIAN_POINT('',(7.6,-9.30731567351988E-16,-1.));
#37629=CARTESIAN_POINT('',(7.6,-9.30731567351989E-16,1.));
#37630=CARTESIAN_POINT('Origin',(0.,0.,-1.));
#37631=CARTESIAN_POINT('Origin',(0.,0.,1.));
#37632=CARTESIAN_POINT('',(27.5,-3.36777869765522E-15,-1.));
#37633=CARTESIAN_POINT('Origin',(0.,0.,-1.));
#37634=CARTESIAN_POINT('',(27.5,-3.36777869765522E-15,1.));
#37635=CARTESIAN_POINT('',(27.5,-3.36777869765522E-15,1.));
#37636=CARTESIAN_POINT('Origin',(0.,0.,1.));
#37637=CARTESIAN_POINT('Origin',(0.,0.,1.));
#37638=CARTESIAN_POINT('Origin',(0.,0.,-1.));
#37639=CARTESIAN_POINT('',(0.,0.,0.));
#37640=CARTESIAN_POINT('Origin',(0.,0.,10.));
#37641=CARTESIAN_POINT('',(3.97500000000002,1.13607475990613E-16,9.49999999999999));
#37642=CARTESIAN_POINT('Origin',(6.93889390390723E-15,-2.08166817117217E-14,
9.49999999999999));
#37643=CARTESIAN_POINT('',(3.47500000000001,5.66883636178462E-17,10.));
#37644=CARTESIAN_POINT('',(3.47500000000001,5.66883636178462E-17,10.));
#37645=CARTESIAN_POINT('Origin',(0.,0.,10.));
#37646=CARTESIAN_POINT('Origin',(1.38777878078145E-14,-1.38777878078145E-14,
-2.5));
#37647=CARTESIAN_POINT('',(3.00000000000003,-1.363379816016E-14,-4.49999999999999));
#37648=CARTESIAN_POINT('Origin',(2.77555756156289E-14,-4.16333634234434E-14,
-4.49999999999999));
#37649=CARTESIAN_POINT('',(5.00000000000002,-1.37962218169974E-14,-2.5));
#37650=CARTESIAN_POINT('Origin',(3.00000000000001,-1.38288482133242E-14,
-2.5));
#37651=CARTESIAN_POINT('',(-4.99999999999999,-4.20318857506523E-14,-2.5));
#37652=CARTESIAN_POINT('Origin',(1.38777878078145E-14,-1.38777878078145E-14,
-2.5));
#37653=CARTESIAN_POINT('Origin',(1.38777878078145E-14,-1.38777878078145E-14,
-2.5));
#37654=CARTESIAN_POINT('Origin',(2.77555756156289E-14,-4.16333634234434E-14,
-4.49999999999999));
#37655=CARTESIAN_POINT('',(-4.99999999999998,-4.33784388330273E-14,-2.22044604925031E-15));
#37656=CARTESIAN_POINT('Origin',(0.,0.,0.));
#37657=CARTESIAN_POINT('',(-4.99999999999998,-4.29395762134078E-14,-4.49999999999999));
#37658=CARTESIAN_POINT('Origin',(0.,0.,10.));
#37659=CARTESIAN_POINT('',(3.97500000000001,1.04009522852078E-15,1.11022302462516E-15));
#37660=CARTESIAN_POINT('Origin',(0.,0.,0.));
#37661=CARTESIAN_POINT('',(3.97500000000001,6.48449626995507E-17,10.));
#37662=CARTESIAN_POINT('Origin',(0.,0.,10.));
#37663=CARTESIAN_POINT('Origin',(2.77555756156289E-14,-4.16333634234434E-14,
-4.49999999999999));
#37664=CARTESIAN_POINT('Origin',(0.,0.,0.));
#37665=CARTESIAN_POINT('',(0.,0.,0.));
#37666=CARTESIAN_POINT('Origin',(0.,0.,-18.5));
#37667=CARTESIAN_POINT('',(-2.5,-3.06161699786838E-16,-3.5));
#37668=CARTESIAN_POINT('Origin',(0.,0.,-3.5));
#37669=CARTESIAN_POINT('',(-2.5,-3.06161699786838E-16,-18.5));
#37670=CARTESIAN_POINT('',(-2.5,-3.06161699786838E-16,-18.5));
#37671=CARTESIAN_POINT('Origin',(0.,0.,-18.5));
#37672=CARTESIAN_POINT('Origin',(4.,-2.3094010767585,-3.5));
#37673=CARTESIAN_POINT('',(4.,-2.3094010767585,0.));
#37674=CARTESIAN_POINT('',(4.,2.3094010767585,0.));
#37675=CARTESIAN_POINT('',(4.,-2.3094010767585,0.));
#37676=CARTESIAN_POINT('',(4.,-2.3094010767585,-3.5));
#37677=CARTESIAN_POINT('',(4.,-2.3094010767585,-3.5));
#37678=CARTESIAN_POINT('',(4.,2.3094010767585,-3.5));
#37679=CARTESIAN_POINT('',(4.,-2.3094010767585,-3.5));
#37680=CARTESIAN_POINT('',(4.,2.3094010767585,-3.5));
#37681=CARTESIAN_POINT('Origin',(3.25260651745651E-16,-4.61880215351701,
-3.5));
#37682=CARTESIAN_POINT('',(3.25260651745651E-16,-4.61880215351701,0.));
#37683=CARTESIAN_POINT('',(3.25260651745651E-16,-4.61880215351701,0.));
#37684=CARTESIAN_POINT('',(3.25260651745651E-16,-4.61880215351701,-3.5));
#37685=CARTESIAN_POINT('',(3.25260651745651E-16,-4.61880215351701,-3.5));
#37686=CARTESIAN_POINT('',(3.25260651745651E-16,-4.61880215351701,-3.5));
#37687=CARTESIAN_POINT('Origin',(-4.,-2.3094010767585,-3.5));
#37688=CARTESIAN_POINT('',(-4.,-2.3094010767585,0.));
#37689=CARTESIAN_POINT('',(-4.,-2.3094010767585,0.));
#37690=CARTESIAN_POINT('',(-4.,-2.3094010767585,-3.5));
#37691=CARTESIAN_POINT('',(-4.,-2.3094010767585,-3.5));
#37692=CARTESIAN_POINT('',(-4.,-2.3094010767585,-3.5));
#37693=CARTESIAN_POINT('Origin',(-4.,2.3094010767585,-3.5));
#37694=CARTESIAN_POINT('',(-4.,2.3094010767585,0.));
#37695=CARTESIAN_POINT('',(-4.,2.3094010767585,0.));
#37696=CARTESIAN_POINT('',(-4.,2.3094010767585,-3.5));
#37697=CARTESIAN_POINT('',(-4.,2.3094010767585,-3.5));
#37698=CARTESIAN_POINT('',(-4.,2.3094010767585,-3.5));
#37699=CARTESIAN_POINT('Origin',(0.,4.61880215351701,-3.5));
#37700=CARTESIAN_POINT('',(0.,4.61880215351701,0.));
#37701=CARTESIAN_POINT('',(0.,4.61880215351701,0.));
#37702=CARTESIAN_POINT('',(0.,4.61880215351701,-3.5));
#37703=CARTESIAN_POINT('',(0.,4.61880215351701,-3.5));
#37704=CARTESIAN_POINT('',(0.,4.61880215351701,-3.5));
#37705=CARTESIAN_POINT('Origin',(4.,2.3094010767585,-3.5));
#37706=CARTESIAN_POINT('',(4.,2.3094010767585,0.));
#37707=CARTESIAN_POINT('',(4.,2.3094010767585,-3.5));
#37708=CARTESIAN_POINT('Origin',(0.,0.,-3.5));
#37709=CARTESIAN_POINT('Origin',(0.,0.,0.));
#37710=CARTESIAN_POINT('Origin',(0.,0.,-18.5));
#37711=CARTESIAN_POINT('',(0.,0.,0.));
#37712=CARTESIAN_POINT('Origin',(8.,0.,-5.));
#37713=CARTESIAN_POINT('',(2.00000000000001,0.,-5.));
#37714=CARTESIAN_POINT('',(6.00000000000001,0.,-5.));
#37715=CARTESIAN_POINT('',(8.,0.,-5.));
#37716=CARTESIAN_POINT('',(6.00000000000001,0.,0.));
#37717=CARTESIAN_POINT('',(6.00000000000001,0.,-5.));
#37718=CARTESIAN_POINT('',(2.00000000000001,0.,0.));
#37719=CARTESIAN_POINT('',(8.,0.,0.));
#37720=CARTESIAN_POINT('',(2.00000000000001,0.,-5.));
#37721=CARTESIAN_POINT('Origin',(0.,0.,-5.));
#37722=CARTESIAN_POINT('',(0.,23.,0.));
#37723=CARTESIAN_POINT('',(0.,2.,0.));
#37724=CARTESIAN_POINT('',(0.,0.,0.));
#37725=CARTESIAN_POINT('',(0.,23.,-5.));
#37726=CARTESIAN_POINT('',(0.,23.,-5.));
#37727=CARTESIAN_POINT('',(0.,2.,-5.));
#37728=CARTESIAN_POINT('',(0.,0.,-5.));
#37729=CARTESIAN_POINT('',(0.,2.,-5.));
#37730=CARTESIAN_POINT('Origin',(0.,25.,-5.));
#37731=CARTESIAN_POINT('',(24.,25.,0.));
#37732=CARTESIAN_POINT('',(2.,25.,0.));
#37733=CARTESIAN_POINT('',(0.,25.,0.));
#37734=CARTESIAN_POINT('',(24.,25.,-5.));
#37735=CARTESIAN_POINT('',(24.,25.,-5.));
#37736=CARTESIAN_POINT('',(2.,25.,-5.));
#37737=CARTESIAN_POINT('',(0.,25.,-5.));
#37738=CARTESIAN_POINT('',(2.,25.,-5.));
#37739=CARTESIAN_POINT('Origin',(26.,25.,-5.));
#37740=CARTESIAN_POINT('',(26.,-20.,-5.));
#37741=CARTESIAN_POINT('',(26.,23.,-5.));
#37742=CARTESIAN_POINT('',(26.,25.,-5.));
#37743=CARTESIAN_POINT('',(26.,23.,0.));
#37744=CARTESIAN_POINT('',(26.,23.,-5.));
#37745=CARTESIAN_POINT('',(26.,-20.,0.));
#37746=CARTESIAN_POINT('',(26.,25.,0.));
#37747=CARTESIAN_POINT('',(26.,-20.,-5.));
#37748=CARTESIAN_POINT('Origin',(26.,-20.,-5.));
#37749=CARTESIAN_POINT('',(18.,-20.,0.));
#37750=CARTESIAN_POINT('',(26.,-20.,0.));
#37751=CARTESIAN_POINT('',(18.,-20.,-5.));
#37752=CARTESIAN_POINT('',(18.,-20.,-5.));
#37753=CARTESIAN_POINT('',(26.,-20.,-5.));
#37754=CARTESIAN_POINT('Origin',(18.,-20.,-5.));
#37755=CARTESIAN_POINT('',(18.,10.,0.));
#37756=CARTESIAN_POINT('',(18.,-20.,0.));
#37757=CARTESIAN_POINT('',(18.,10.,-5.));
#37758=CARTESIAN_POINT('',(18.,10.,-5.));
#37759=CARTESIAN_POINT('',(18.,-20.,-5.));
#37760=CARTESIAN_POINT('Origin',(18.,12.,-5.));
#37761=CARTESIAN_POINT('',(10.,12.,-5.));
#37762=CARTESIAN_POINT('',(16.,12.,-5.));
#37763=CARTESIAN_POINT('',(18.,12.,-5.));
#37764=CARTESIAN_POINT('',(16.,12.,0.));
#37765=CARTESIAN_POINT('',(16.,12.,0.));
#37766=CARTESIAN_POINT('',(10.,12.,0.));
#37767=CARTESIAN_POINT('',(18.,12.,0.));
#37768=CARTESIAN_POINT('',(10.,12.,-5.));
#37769=CARTESIAN_POINT('Origin',(8.,12.,-5.));
#37770=CARTESIAN_POINT('',(8.,2.,-5.));
#37771=CARTESIAN_POINT('',(8.,9.99999999999998,-5.));
#37772=CARTESIAN_POINT('',(8.,12.,-5.));
#37773=CARTESIAN_POINT('',(8.,9.99999999999998,0.));
#37774=CARTESIAN_POINT('',(8.,9.99999999999998,0.));
#37775=CARTESIAN_POINT('',(8.,2.,0.));
#37776=CARTESIAN_POINT('',(8.,12.,0.));
#37777=CARTESIAN_POINT('',(8.,2.,-5.));
#37778=CARTESIAN_POINT('Origin',(0.,0.,-5.));
#37779=CARTESIAN_POINT('',(24.5,24.5,-5.));
#37780=CARTESIAN_POINT('',(16.,12.,-5.));
#37781=CARTESIAN_POINT('',(8.,9.99999999999998,-5.));
#37782=CARTESIAN_POINT('',(3.00000000000003,-3.00000000000001,-5.));
#37783=CARTESIAN_POINT('',(0.999999999999998,1.,-5.));
#37784=CARTESIAN_POINT('',(-11.5,11.4999999999999,-5.));
#37785=CARTESIAN_POINT('Origin',(0.,0.,0.));
#37786=CARTESIAN_POINT('',(26.,23.,0.));
#37787=CARTESIAN_POINT('',(2.,25.,0.));
#37788=CARTESIAN_POINT('',(0.,2.,0.));
#37789=CARTESIAN_POINT('',(6.00000000000001,0.,0.));
#37790=CARTESIAN_POINT('',(-0.999999999999961,0.999999999999954,0.));
#37791=CARTESIAN_POINT('',(13.9999999999999,14.0000000000001,0.));
#37792=CARTESIAN_POINT('Origin',(26.,23.,-5.));
#37793=CARTESIAN_POINT('Origin',(2.,25.,-5.));
#37794=CARTESIAN_POINT('Origin',(16.,12.,-5.));
#37795=CARTESIAN_POINT('Origin',(8.,9.99999999999998,-5.));
#37796=CARTESIAN_POINT('Origin',(6.00000000000001,0.,-5.));
#37797=CARTESIAN_POINT('Origin',(0.,2.,-5.));
#37798=CARTESIAN_POINT('',(0.,0.,0.));
#37799=CARTESIAN_POINT('Origin',(0.,0.,0.));
#37800=CARTESIAN_POINT('',(-7.5,-9.1848509936055E-16,-10.));
#37801=CARTESIAN_POINT('Origin',(0.,-1.38777878078145E-14,-10.));
#37802=CARTESIAN_POINT('',(-7.5,-9.18485099360515E-16,1.12412678993994E-28));
#37803=CARTESIAN_POINT('',(-7.5,-9.18485099360515E-16,1.12412678993994E-28));
#37804=CARTESIAN_POINT('Origin',(0.,0.,0.));
#37805=CARTESIAN_POINT('Origin',(0.,0.,0.));
#37806=CARTESIAN_POINT('',(-17.5,-2.14313189850787E-15,2.62296250985986E-28));
#37807=CARTESIAN_POINT('Origin',(0.,0.,0.));
#37808=CARTESIAN_POINT('',(-17.5,-2.1431318985079E-15,-10.));
#37809=CARTESIAN_POINT('',(-17.5,-2.14313189850787E-15,2.62296250985986E-28));
#37810=CARTESIAN_POINT('Origin',(0.,-1.38777878078145E-14,-10.));
#37811=CARTESIAN_POINT('Origin',(0.,7.5,0.));
#37812=CARTESIAN_POINT('Origin',(0.,7.5,-10.));
#37813=CARTESIAN_POINT('',(0.,0.,0.));
#37814=CARTESIAN_POINT('',(-5.99999999999988,29.6605322777956,24.2152735740756));
#37815=CARTESIAN_POINT('',(4.65999999999978,-20.4999999999999,-24.5));
#37816=CARTESIAN_POINT('',(4.66000000000008,-20.4999999999999,16.85));
#37817=CARTESIAN_POINT('',(63.0000000000001,36.18,14.4999999999995));
#37818=CARTESIAN_POINT('',(1.7650811368064E-13,6.24500451351651E-14,29.));
#37819=CARTESIAN_POINT('',(-41.9999999999996,-56.5,53.5000000000003));
#37820=CARTESIAN_POINT('',(13.0067743311234,-8.33842698228136,5.49999999999992));
#37821=CARTESIAN_POINT('',(-67.4999999999999,57.18,14.5000000000005));
#37822=CARTESIAN_POINT('',(-88.,51.5,-14.5));
#37823=CARTESIAN_POINT('',(4.66,-20.5,-25.5));
#37824=CARTESIAN_POINT('',(-51.9999999999999,36.18,14.5000000000004));
#37825=CARTESIAN_POINT('',(-62.9999999999999,36.18,14.5000000000002));
#37826=CARTESIAN_POINT('',(-45.9999999999998,76.5000000000001,27.0000000000003));
#37827=CARTESIAN_POINT('',(-67.5,46.6800000000001,-3.68653347947288));
#37828=CARTESIAN_POINT('',(-67.5,25.6800000000001,-3.68653347947306));
#37829=CARTESIAN_POINT('',(-67.4999999999999,15.18,14.5000000000001));
#37830=CARTESIAN_POINT('',(-67.4999999999998,25.6799999999999,32.6865334794734));
#37831=CARTESIAN_POINT('',(-67.4999999999998,46.68,32.6865334794735));
#37832=CARTESIAN_POINT('',(67.5000000000002,46.68,32.6865334794727));
#37833=CARTESIAN_POINT('',(67.5000000000002,25.68,32.6865334794727));
#37834=CARTESIAN_POINT('',(67.5000000000001,15.18,14.4999999999995));
#37835=CARTESIAN_POINT('',(67.5,25.6800000000001,-3.68653347947373));
#37836=CARTESIAN_POINT('',(67.5,46.6800000000001,-3.68653347947359));
#37837=CARTESIAN_POINT('',(67.5000000000002,57.18,14.4999999999997));
#37838=CARTESIAN_POINT('',(4.66000000000038,4.50000000000005,57.));
#37839=CARTESIAN_POINT('',(26.3106350946114,-8.,56.9999999999998));
#37840=CARTESIAN_POINT('',(26.3106350946113,-33.0000000000001,56.9999999999997));
#37841=CARTESIAN_POINT('',(4.66000000000022,-45.5,56.9999999999999));
#37842=CARTESIAN_POINT('',(-16.9906350946107,-32.9999999999998,57.0000000000001));
#37843=CARTESIAN_POINT('',(-16.9906350946105,-7.99999999999971,57.0000000000001));
#37844=CARTESIAN_POINT('',(4.65999999999979,4.49999999999999,-30.));
#37845=CARTESIAN_POINT('',(26.3106350946109,-7.99999999999988,-30.));
#37846=CARTESIAN_POINT('',(26.310635094611,-32.9999999999999,-30.));
#37847=CARTESIAN_POINT('',(4.66000000000004,-45.5,-30.));
#37848=CARTESIAN_POINT('',(-16.990635094611,-33.,-30.));
#37849=CARTESIAN_POINT('',(-16.9906350946109,-7.99999999999994,-30.));
#37850=CARTESIAN_POINT('',(88.,51.5,-19.5));
#37851=CARTESIAN_POINT('',(4.66000000000028,-20.5,43.5));
#37852=CARTESIAN_POINT('',(52.0000000000001,36.18,14.4999999999996));
#37853=CARTESIAN_POINT('',(4.6599999999999,-20.5,-14.5));
#37854=UNCERTAINTY_MEASURE_WITH_UNIT(LENGTH_MEASURE(0.01),#37882,
'DISTANCE_ACCURACY_VALUE',
'Maximum model space distance between geometric entities at asserted c
onnectivities');
#37855=UNCERTAINTY_MEASURE_WITH_UNIT(LENGTH_MEASURE(0.01),#37882,
'DISTANCE_ACCURACY_VALUE',
'Maximum model space distance between geometric entities at asserted c
onnectivities');
#37856=UNCERTAINTY_MEASURE_WITH_UNIT(LENGTH_MEASURE(0.01),#37882,
'DISTANCE_ACCURACY_VALUE',
'Maximum model space distance between geometric entities at asserted c
onnectivities');
#37857=UNCERTAINTY_MEASURE_WITH_UNIT(LENGTH_MEASURE(0.01),#37882,
'DISTANCE_ACCURACY_VALUE',
'Maximum model space distance between geometric entities at asserted c
onnectivities');
#37858=UNCERTAINTY_MEASURE_WITH_UNIT(LENGTH_MEASURE(0.01),#37882,
'DISTANCE_ACCURACY_VALUE',
'Maximum model space distance between geometric entities at asserted c
onnectivities');
#37859=UNCERTAINTY_MEASURE_WITH_UNIT(LENGTH_MEASURE(0.01),#37882,
'DISTANCE_ACCURACY_VALUE',
'Maximum model space distance between geometric entities at asserted c
onnectivities');
#37860=UNCERTAINTY_MEASURE_WITH_UNIT(LENGTH_MEASURE(0.01),#37882,
'DISTANCE_ACCURACY_VALUE',
'Maximum model space distance between geometric entities at asserted c
onnectivities');
#37861=UNCERTAINTY_MEASURE_WITH_UNIT(LENGTH_MEASURE(0.01),#37882,
'DISTANCE_ACCURACY_VALUE',
'Maximum model space distance between geometric entities at asserted c
onnectivities');
#37862=UNCERTAINTY_MEASURE_WITH_UNIT(LENGTH_MEASURE(0.01),#37882,
'DISTANCE_ACCURACY_VALUE',
'Maximum model space distance between geometric entities at asserted c
onnectivities');
#37863=UNCERTAINTY_MEASURE_WITH_UNIT(LENGTH_MEASURE(0.01),#37882,
'DISTANCE_ACCURACY_VALUE',
'Maximum model space distance between geometric entities at asserted c
onnectivities');
#37864=UNCERTAINTY_MEASURE_WITH_UNIT(LENGTH_MEASURE(0.01),#37882,
'DISTANCE_ACCURACY_VALUE',
'Maximum model space distance between geometric entities at asserted c
onnectivities');
#37865=UNCERTAINTY_MEASURE_WITH_UNIT(LENGTH_MEASURE(0.01),#37882,
'DISTANCE_ACCURACY_VALUE',
'Maximum model space distance between geometric entities at asserted c
onnectivities');
#37866=UNCERTAINTY_MEASURE_WITH_UNIT(LENGTH_MEASURE(0.01),#37882,
'DISTANCE_ACCURACY_VALUE',
'Maximum model space distance between geometric entities at asserted c
onnectivities');
#37867=UNCERTAINTY_MEASURE_WITH_UNIT(LENGTH_MEASURE(0.01),#37882,
'DISTANCE_ACCURACY_VALUE',
'Maximum model space distance between geometric entities at asserted c
onnectivities');
#37868=(
GEOMETRIC_REPRESENTATION_CONTEXT(3)
GLOBAL_UNCERTAINTY_ASSIGNED_CONTEXT((#37854))
GLOBAL_UNIT_ASSIGNED_CONTEXT((#37882,#37884,#37885))
REPRESENTATION_CONTEXT('','3D')
);
#37869=(
GEOMETRIC_REPRESENTATION_CONTEXT(3)
GLOBAL_UNCERTAINTY_ASSIGNED_CONTEXT((#37855))
GLOBAL_UNIT_ASSIGNED_CONTEXT((#37882,#37884,#37885))
REPRESENTATION_CONTEXT('','3D')
);
#37870=(
GEOMETRIC_REPRESENTATION_CONTEXT(3)
GLOBAL_UNCERTAINTY_ASSIGNED_CONTEXT((#37856))
GLOBAL_UNIT_ASSIGNED_CONTEXT((#37882,#37884,#37885))
REPRESENTATION_CONTEXT('','3D')
);
#37871=(
GEOMETRIC_REPRESENTATION_CONTEXT(3)
GLOBAL_UNCERTAINTY_ASSIGNED_CONTEXT((#37857))
GLOBAL_UNIT_ASSIGNED_CONTEXT((#37882,#37884,#37885))
REPRESENTATION_CONTEXT('','3D')
);
#37872=(
GEOMETRIC_REPRESENTATION_CONTEXT(3)
GLOBAL_UNCERTAINTY_ASSIGNED_CONTEXT((#37858))
GLOBAL_UNIT_ASSIGNED_CONTEXT((#37882,#37884,#37885))
REPRESENTATION_CONTEXT('','3D')
);
#37873=(
GEOMETRIC_REPRESENTATION_CONTEXT(3)
GLOBAL_UNCERTAINTY_ASSIGNED_CONTEXT((#37859))
GLOBAL_UNIT_ASSIGNED_CONTEXT((#37882,#37884,#37885))
REPRESENTATION_CONTEXT('','3D')
);
#37874=(
GEOMETRIC_REPRESENTATION_CONTEXT(3)
GLOBAL_UNCERTAINTY_ASSIGNED_CONTEXT((#37860))
GLOBAL_UNIT_ASSIGNED_CONTEXT((#37882,#37884,#37885))
REPRESENTATION_CONTEXT('','3D')
);
#37875=(
GEOMETRIC_REPRESENTATION_CONTEXT(3)
GLOBAL_UNCERTAINTY_ASSIGNED_CONTEXT((#37861))
GLOBAL_UNIT_ASSIGNED_CONTEXT((#37882,#37884,#37885))
REPRESENTATION_CONTEXT('','3D')
);
#37876=(
GEOMETRIC_REPRESENTATION_CONTEXT(3)
GLOBAL_UNCERTAINTY_ASSIGNED_CONTEXT((#37862))
GLOBAL_UNIT_ASSIGNED_CONTEXT((#37882,#37884,#37885))
REPRESENTATION_CONTEXT('','3D')
);
#37877=(
GEOMETRIC_REPRESENTATION_CONTEXT(3)
GLOBAL_UNCERTAINTY_ASSIGNED_CONTEXT((#37863))
GLOBAL_UNIT_ASSIGNED_CONTEXT((#37882,#37884,#37885))
REPRESENTATION_CONTEXT('','3D')
);
#37878=(
GEOMETRIC_REPRESENTATION_CONTEXT(3)
GLOBAL_UNCERTAINTY_ASSIGNED_CONTEXT((#37864))
GLOBAL_UNIT_ASSIGNED_CONTEXT((#37882,#37884,#37885))
REPRESENTATION_CONTEXT('','3D')
);
#37879=(
GEOMETRIC_REPRESENTATION_CONTEXT(3)
GLOBAL_UNCERTAINTY_ASSIGNED_CONTEXT((#37865))
GLOBAL_UNIT_ASSIGNED_CONTEXT((#37882,#37884,#37885))
REPRESENTATION_CONTEXT('','3D')
);
#37880=(
GEOMETRIC_REPRESENTATION_CONTEXT(3)
GLOBAL_UNCERTAINTY_ASSIGNED_CONTEXT((#37866))
GLOBAL_UNIT_ASSIGNED_CONTEXT((#37882,#37884,#37885))
REPRESENTATION_CONTEXT('','3D')
);
#37881=(
GEOMETRIC_REPRESENTATION_CONTEXT(3)
GLOBAL_UNCERTAINTY_ASSIGNED_CONTEXT((#37867))
GLOBAL_UNIT_ASSIGNED_CONTEXT((#37882,#37884,#37885))
REPRESENTATION_CONTEXT('','3D')
);
#37882=(
LENGTH_UNIT()
NAMED_UNIT(*)
SI_UNIT(.MILLI.,.METRE.)
);
#37883=(
LENGTH_UNIT()
NAMED_UNIT(*)
SI_UNIT($,.METRE.)
);
#37884=(
NAMED_UNIT(*)
PLANE_ANGLE_UNIT()
SI_UNIT($,.RADIAN.)
);
#37885=(
NAMED_UNIT(*)
SI_UNIT($,.STERADIAN.)
SOLID_ANGLE_UNIT()
);
#37886=SHAPE_DEFINITION_REPRESENTATION(#37899,#37953);
#37887=SHAPE_DEFINITION_REPRESENTATION(#37900,#37954);
#37888=SHAPE_DEFINITION_REPRESENTATION(#37901,#37955);
#37889=SHAPE_DEFINITION_REPRESENTATION(#37902,#37956);
#37890=SHAPE_DEFINITION_REPRESENTATION(#37903,#37957);
#37891=SHAPE_DEFINITION_REPRESENTATION(#37904,#37958);
#37892=SHAPE_DEFINITION_REPRESENTATION(#37905,#37959);
#37893=SHAPE_DEFINITION_REPRESENTATION(#37906,#37960);
#37894=SHAPE_DEFINITION_REPRESENTATION(#37907,#37961);
#37895=SHAPE_DEFINITION_REPRESENTATION(#37908,#37962);
#37896=SHAPE_DEFINITION_REPRESENTATION(#37909,#37963);
#37897=SHAPE_DEFINITION_REPRESENTATION(#37910,#37964);
#37898=SHAPE_DEFINITION_REPRESENTATION(#37911,#37965);
#37899=PRODUCT_DEFINITION_SHAPE('',$,#37967);
#37900=PRODUCT_DEFINITION_SHAPE('',$,#37968);
#37901=PRODUCT_DEFINITION_SHAPE('',$,#37969);
#37902=PRODUCT_DEFINITION_SHAPE('',$,#37970);
#37903=PRODUCT_DEFINITION_SHAPE('',$,#37971);
#37904=PRODUCT_DEFINITION_SHAPE('',$,#37972);
#37905=PRODUCT_DEFINITION_SHAPE('',$,#37973);
#37906=PRODUCT_DEFINITION_SHAPE('',$,#37974);
#37907=PRODUCT_DEFINITION_SHAPE('',$,#37975);
#37908=PRODUCT_DEFINITION_SHAPE('',$,#37976);
#37909=PRODUCT_DEFINITION_SHAPE('',$,#37977);
#37910=PRODUCT_DEFINITION_SHAPE('',$,#37978);
#37911=PRODUCT_DEFINITION_SHAPE('',$,#37979);
#37912=PRODUCT_DEFINITION_SHAPE($,$,#134);
#37913=PRODUCT_DEFINITION_SHAPE($,$,#135);
#37914=PRODUCT_DEFINITION_SHAPE($,$,#136);
#37915=PRODUCT_DEFINITION_SHAPE($,$,#137);
#37916=PRODUCT_DEFINITION_SHAPE($,$,#138);
#37917=PRODUCT_DEFINITION_SHAPE($,$,#139);
#37918=PRODUCT_DEFINITION_SHAPE($,$,#140);
#37919=PRODUCT_DEFINITION_SHAPE($,$,#141);
#37920=PRODUCT_DEFINITION_SHAPE($,$,#142);
#37921=PRODUCT_DEFINITION_SHAPE($,$,#143);
#37922=PRODUCT_DEFINITION_SHAPE($,$,#144);
#37923=PRODUCT_DEFINITION_SHAPE($,$,#145);
#37924=PRODUCT_DEFINITION_SHAPE($,$,#146);
#37925=PRODUCT_DEFINITION_SHAPE($,$,#147);
#37926=PRODUCT_DEFINITION_SHAPE($,$,#148);
#37927=PRODUCT_DEFINITION_SHAPE($,$,#149);
#37928=PRODUCT_DEFINITION_SHAPE($,$,#150);
#37929=PRODUCT_DEFINITION_SHAPE($,$,#151);
#37930=PRODUCT_DEFINITION_SHAPE($,$,#152);
#37931=PRODUCT_DEFINITION_SHAPE($,$,#153);
#37932=PRODUCT_DEFINITION_SHAPE($,$,#154);
#37933=PRODUCT_DEFINITION_SHAPE($,$,#155);
#37934=PRODUCT_DEFINITION_SHAPE($,$,#156);
#37935=PRODUCT_DEFINITION_SHAPE($,$,#157);
#37936=PRODUCT_DEFINITION_SHAPE($,$,#158);
#37937=PRODUCT_DEFINITION_SHAPE($,$,#159);
#37938=PRODUCT_DEFINITION_SHAPE($,$,#160);
#37939=PRODUCT_DEFINITION_SHAPE($,$,#161);
#37940=PRODUCT_DEFINITION_SHAPE($,$,#162);
#37941=PRODUCT_DEFINITION_SHAPE($,$,#163);
#37942=PRODUCT_DEFINITION_SHAPE($,$,#164);
#37943=PRODUCT_DEFINITION_SHAPE($,$,#165);
#37944=PRODUCT_DEFINITION_SHAPE($,$,#166);
#37945=PRODUCT_DEFINITION_SHAPE($,$,#167);
#37946=PRODUCT_DEFINITION_SHAPE($,$,#168);
#37947=PRODUCT_DEFINITION_SHAPE($,$,#169);
#37948=PRODUCT_DEFINITION_SHAPE($,$,#170);
#37949=PRODUCT_DEFINITION_SHAPE($,$,#171);
#37950=PRODUCT_DEFINITION_SHAPE($,$,#172);
#37951=PRODUCT_DEFINITION_SHAPE($,$,#173);
#37952=PRODUCT_DEFINITION_SHAPE($,$,#174);
#37953=SHAPE_REPRESENTATION('',(#10964,#11849,#11850,#11851,#11852,#11853,
#11854,#11855,#11856,#11857,#11858,#11859,#11860,#11861,#11862,#11863,#11864,
#11865,#11866,#11867,#11868,#11869,#11870,#11871,#11872,#11873,#11874,#11875,
#11876,#11877,#11878,#11879,#11880,#11881,#11882,#11883,#11884,#11885,#11886,
#11887,#11888,#11889),#37868);
#37954=SHAPE_REPRESENTATION('',(#10965),#37869);
#37955=SHAPE_REPRESENTATION('',(#11041),#37870);
#37956=SHAPE_REPRESENTATION('',(#11080),#37871);
#37957=SHAPE_REPRESENTATION('',(#11110),#37872);
#37958=SHAPE_REPRESENTATION('',(#11607),#37873);
#37959=SHAPE_REPRESENTATION('',(#11689),#37874);
#37960=SHAPE_REPRESENTATION('',(#11740),#37875);
#37961=SHAPE_REPRESENTATION('',(#11767),#37876);
#37962=SHAPE_REPRESENTATION('',(#11794),#37877);
#37963=SHAPE_REPRESENTATION('',(#11810),#37878);
#37964=SHAPE_REPRESENTATION('',(#11823),#37879);
#37965=SHAPE_REPRESENTATION('',(#11840),#37880);
#37966=PRODUCT_DEFINITION_CONTEXT('part definition',#38007,'design');
#37967=PRODUCT_DEFINITION('MAS-619','MAS-619',#37980,#37966);
#37968=PRODUCT_DEFINITION('PS01','Body_A',#37981,#37966);
#37969=PRODUCT_DEFINITION('PS02','Worm_Shaft',#37982,#37966);
#37970=PRODUCT_DEFINITION('PS03','Worm_Wheel_Shaft',#37983,#37966);
#37971=PRODUCT_DEFINITION('PS05','Worm_Wheel',#37984,#37966);
#37972=PRODUCT_DEFINITION('PS06','Body_B',#37985,#37966);
#37973=PRODUCT_DEFINITION('PS08','Key',#37986,#37966);
#37974=PRODUCT_DEFINITION('PS10','Rear_Side_Flange',#37987,#37966);
#37975=PRODUCT_DEFINITION('PS04','Flange',#37988,#37966);
#37976=PRODUCT_DEFINITION('PS07','Oil_Bolt',#37989,#37966);
#37977=PRODUCT_DEFINITION('PS11','M5 Bolt',#37990,#37966);
#37978=PRODUCT_DEFINITION('PS09','Lifting_Plate',#37991,#37966);
#37979=PRODUCT_DEFINITION('PS12','Bush',#37992,#37966);
#37980=PRODUCT_DEFINITION_FORMATION('',$,#38009);
#37981=PRODUCT_DEFINITION_FORMATION('',$,#38010);
#37982=PRODUCT_DEFINITION_FORMATION('',$,#38011);
#37983=PRODUCT_DEFINITION_FORMATION('',$,#38012);
#37984=PRODUCT_DEFINITION_FORMATION('',$,#38013);
#37985=PRODUCT_DEFINITION_FORMATION('',$,#38014);
#37986=PRODUCT_DEFINITION_FORMATION('',$,#38015);
#37987=PRODUCT_DEFINITION_FORMATION('',$,#38016);
#37988=PRODUCT_DEFINITION_FORMATION('',$,#38017);
#37989=PRODUCT_DEFINITION_FORMATION('',$,#38018);
#37990=PRODUCT_DEFINITION_FORMATION('',$,#38019);
#37991=PRODUCT_DEFINITION_FORMATION('',$,#38020);
#37992=PRODUCT_DEFINITION_FORMATION('',$,#38021);
#37993=PRODUCT_RELATED_PRODUCT_CATEGORY('MAS-619','MAS-619',(#38009));
#37994=PRODUCT_RELATED_PRODUCT_CATEGORY('Body_A','Body_A',(#38010));
#37995=PRODUCT_RELATED_PRODUCT_CATEGORY('Worm_Shaft','Worm_Shaft',(#38011));
#37996=PRODUCT_RELATED_PRODUCT_CATEGORY('Worm_Wheel_Shaft',
'Worm_Wheel_Shaft',(#38012));
#37997=PRODUCT_RELATED_PRODUCT_CATEGORY('Worm_Wheel','Worm_Wheel',(#38013));
#37998=PRODUCT_RELATED_PRODUCT_CATEGORY('Body_B','Body_B',(#38014));
#37999=PRODUCT_RELATED_PRODUCT_CATEGORY('Key','Key',(#38015));
#38000=PRODUCT_RELATED_PRODUCT_CATEGORY('Rear_Side_Flange',
'Rear_Side_Flange',(#38016));
#38001=PRODUCT_RELATED_PRODUCT_CATEGORY('Flange','Flange',(#38017));
#38002=PRODUCT_RELATED_PRODUCT_CATEGORY('Oil_Bolt','Oil_Bolt',(#38018));
#38003=PRODUCT_RELATED_PRODUCT_CATEGORY('M5 Bolt','M5 Bolt',(#38019));
#38004=PRODUCT_RELATED_PRODUCT_CATEGORY('Lifting_Plate','Lifting_Plate',
(#38020));
#38005=PRODUCT_RELATED_PRODUCT_CATEGORY('Bush','Bush',(#38021));
#38006=APPLICATION_PROTOCOL_DEFINITION('international standard',
'automotive_design',2009,#38007);
#38007=APPLICATION_CONTEXT(
'Core Data for Automotive Mechanical Design Process');
#38008=PRODUCT_CONTEXT('part definition',#38007,'mechanical');
#38009=PRODUCT('MAS-619','MAS-619','STEP AP214',(#38008));
#38010=PRODUCT('PS01','Body_A',$,(#38008));
#38011=PRODUCT('PS02','Worm_Shaft',$,(#38008));
#38012=PRODUCT('PS03','Worm_Wheel_Shaft',$,(#38008));
#38013=PRODUCT('PS05','Worm_Wheel',$,(#38008));
#38014=PRODUCT('PS06','Body_B',$,(#38008));
#38015=PRODUCT('PS08','Key',$,(#38008));
#38016=PRODUCT('PS10','Rear_Side_Flange',$,(#38008));
#38017=PRODUCT('PS04','Flange',$,(#38008));
#38018=PRODUCT('PS07','Oil_Bolt',$,(#38008));
#38019=PRODUCT('PS11','M5 Bolt',$,(#38008));
#38020=PRODUCT('PS09','Lifting_Plate',$,(#38008));
#38021=PRODUCT('PS12','Bush',$,(#38008));
#38022=PRESENTATION_STYLE_ASSIGNMENT((#38024));
#38023=PRESENTATION_STYLE_ASSIGNMENT((#38025));
#38024=SURFACE_STYLE_USAGE(.BOTH.,#38026);
#38025=SURFACE_STYLE_USAGE(.BOTH.,#38027);
#38026=SURFACE_SIDE_STYLE('',(#38028));
#38027=SURFACE_SIDE_STYLE('',(#38029));
#38028=SURFACE_STYLE_FILL_AREA(#38030);
#38029=SURFACE_STYLE_FILL_AREA(#38031);
#38030=FILL_AREA_STYLE('Steel - Satin',(#38032));
#38031=FILL_AREA_STYLE('Opaque(202,209,238)',(#38033));
#38032=FILL_AREA_STYLE_COLOUR('Steel - Satin',#38034);
#38033=FILL_AREA_STYLE_COLOUR('Opaque(202,209,238)',#38035);
#38034=COLOUR_RGB('Steel - Satin', 0.66274510, 0.83137255, 0.94901961);
#38035=COLOUR_RGB('Opaque(202,209,238)', 0.66274510, 0.83137255, 0.94901961);
ENDSEC;
END-ISO-10303-21;
